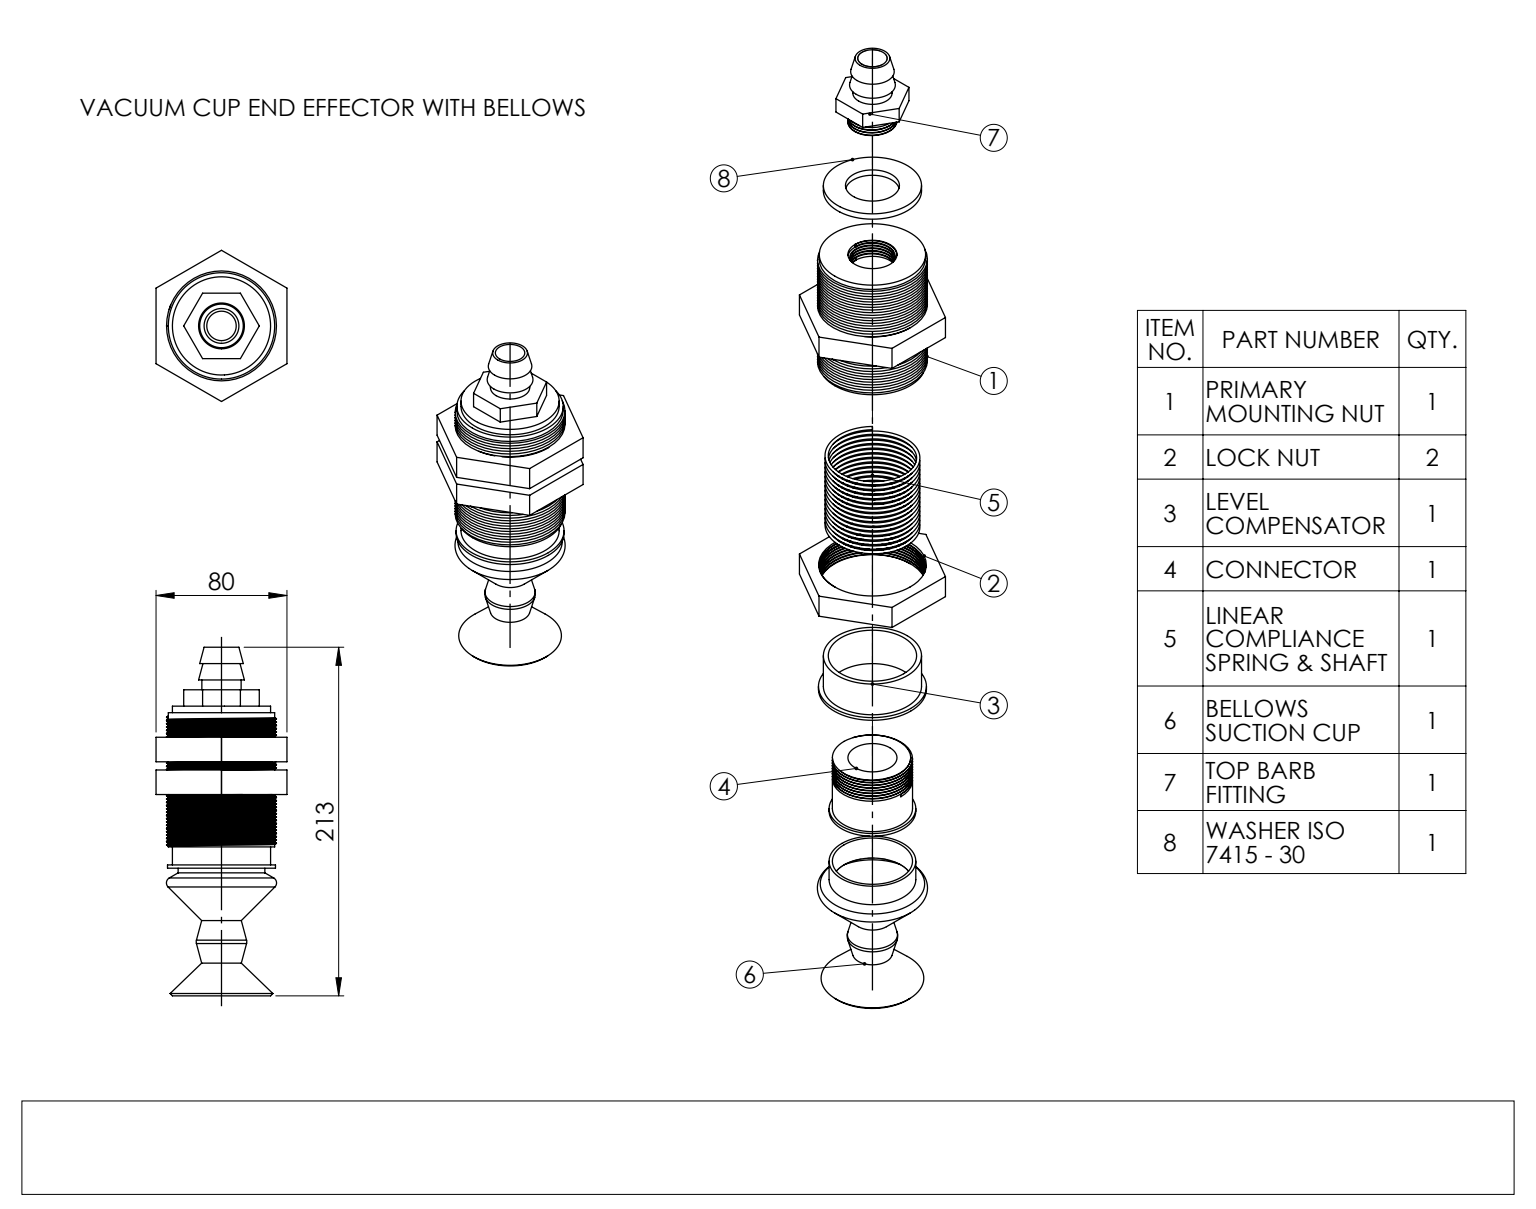
ISO-10303-21;
HEADER;
FILE_DESCRIPTION (('STEP AP214'),
    '1' );
FILE_NAME ('BR-007',
    '2026-10-02T18:08:48',
    ( '' ),
    ( '' ),
    'SwSTEP 2.0',
    'SolidWorks 2026',
    '' );
FILE_SCHEMA (( 'AUTOMOTIVE_DESIGN' ));
ENDSEC;

DATA;
#1 = CARTESIAN_POINT ( 'NONE',  ( -2.584737979205441561E-13, 22.74218749999999645, -30.02300923189239512 ) ) ;
#2 = CARTESIAN_POINT ( 'NONE',  ( 20.75514604977249178, 32.07500000273117990, 28.56700777964553950 ) ) ;
#3 = CARTESIAN_POINT ( 'NONE',  ( 7.236395654485760609, 11.52499999726880375, -22.27133577429736633 ) ) ;
#4 = ORIENTED_EDGE ( 'NONE', *, *, #32426, .T. ) ;
#5 = CARTESIAN_POINT ( 'NONE',  ( 0.04044903254992426173, 37.93006916759064495, -30.02300923189239867 ) ) ;
#6 = B_SPLINE_CURVE_WITH_KNOTS ( 'NONE', 3,
 ( #2746, #31563, #23520, #5150, #31895, #33979, #26595, #13563, #7891, #10812, #8061, #21292, #8391, #3092, #18876, #13210, #18378, #13388, #5322, #18546, #24026, #325, #29325, #15802, #5827, #26258, #31732, #495, #23687, #16306, #152, #15636, #2584, #10642 ),
 .UNSPECIFIED., .F., .F.,
 ( 4, 2, 2, 2, 2, 2, 2, 2, 2, 2, 2, 2, 2, 2, 2, 2, 4 ),
 ( 6.762863467562367515E-16, 0.001783076374787156146, 0.003566152749573635750, 0.007132305499146594091, 0.008023843686539834652, 0.008915381873933073478, 0.01069845824871955460, 0.01248153462350603572, 0.01426461099829251858, 0.01604768737307899970, 0.01783076374786548429, 0.02139691649743844307, 0.02228845468483168710, 0.02317999287222492766, 0.02496306924701141225, 0.02674614562179789337, 0.02852922199658437796 ),
 .UNSPECIFIED. ) ;
#7 = CARTESIAN_POINT ( 'NONE',  ( -32.50000000000000000, 22.50000000546238610, 0.000000000000000000 ) ) ;
#8 = CARTESIAN_POINT ( 'NONE',  ( -2.584737979205441561E-13, 43.36718749999999289, -30.02300923189239512 ) ) ;
#9 = CARTESIAN_POINT ( 'NONE',  ( -23.09401076758502924, 96.00000000000002842, 5.354274672883389237E-15 ) ) ;
#10 = CARTESIAN_POINT ( 'NONE',  ( -2.162160676586881955E-15, 52.87500000273119838, -35.31076352940723240 ) ) ;
#11 = CARTESIAN_POINT ( 'NONE',  ( -2.092463501923844636E-15, 58.00000000546235412, -34.17252228774368916 ) ) ;
#12 = PRODUCT ( 'top barb fitting', 'top barb fitting', '', ( #25356 ) ) ;
#13 = CARTESIAN_POINT ( 'NONE',  ( 15.14183272437242067, 5.449999994537614967, 20.84094480462498211 ) ) ;
#14 = CARTESIAN_POINT ( 'NONE',  ( -2.162160676586881955E-15, 42.62500000273119838, -35.31076352940723240 ) ) ;
#15 = CARTESIAN_POINT ( 'NONE',  ( -4.635254915624208216, 72.40000000000001990, 14.26584774442730463 ) ) ;
#16 = CARTESIAN_POINT ( 'NONE',  ( 33.58253175000000113, 68.47500000273119269, -10.91162601494193751 ) ) ;
#17 =( REPRESENTATION_RELATIONSHIP ('NONE','NONE', #5873, #19696 ) REPRESENTATION_RELATIONSHIP_WITH_TRANSFORMATION ( #15926 )SHAPE_REPRESENTATION_RELATIONSHIP( ) );
#18 = CARTESIAN_POINT ( 'NONE',  ( 13.91687918246660871, 74.00000000000008527, 0.9182373085827880699 ) ) ;
#19 = CARTESIAN_POINT ( 'NONE',  ( 10.37757302488624767, 61.72500000273119269, 31.93888565452638417 ) ) ;
#20 = CARTESIAN_POINT ( 'NONE',  ( 28.01184896238290278, 23.45833333333333215, -7.505752307973347470 ) ) ;
#21 = CARTESIAN_POINT ( 'NONE',  ( 6.277390505771533514E-15, 44.49999999999999289, 34.17252228774368916 ) ) ;
#22 = CARTESIAN_POINT ( 'NONE',  ( 14.47279130897151589, 4.324999997268801799, 19.92008829642072953 ) ) ;
#23 = CARTESIAN_POINT ( 'NONE',  ( -10.37757302488624411, 12.97500000273119092, -31.93888565452638417 ) ) ;
#24 = CARTESIAN_POINT ( 'NONE',  ( -10.04305231718579172, 66.10000000546239107, -30.90933677959248982 ) ) ;
#25 = CARTESIAN_POINT ( 'NONE',  ( -13.94119854578892514, 33.62201416574269075, 24.22776226481266448 ) ) ;
#26 = LINE ( 'NONE', #5703, #33612 ) ;
#27 = CARTESIAN_POINT ( 'NONE',  ( 15.00000000000000355, 75.15000000546237402, 4.873795443493592394 ) ) ;
#28 = CARTESIAN_POINT ( 'NONE',  ( 0.000000000000000000, 82.00000000000001421, 0.000000000000000000 ) ) ;
#29 = CARTESIAN_POINT ( 'NONE',  ( 20.75514604977249178, 76.07500000273118701, 28.56700777964553950 ) ) ;
#30 = EDGE_LOOP ( 'NONE', ( #10708, #16576, #32789, #18480 ) ) ;
#31 = DIRECTION ( 'NONE',  ( 0.000000000000000000, -1.000000000000000000, 0.000000000000000000 ) ) ;
#32 = CARTESIAN_POINT ( 'NONE',  ( -26.07999730980477437, 56.11458333333332860, 6.988114217768305103 ) ) ;
#33 = EDGE_CURVE ( 'NONE', #10375, #21334, #32773, .T. ) ;
#34 = CARTESIAN_POINT ( 'NONE',  ( 20.75514604977248467, 54.42500000273117422, -28.56700777964554305 ) ) ;
#35 = CARTESIAN_POINT ( 'NONE',  ( 33.58253175000000113, 14.37500000273118950, -4.112674001490185761E-15 ) ) ;
#36 = CARTESIAN_POINT ( 'NONE',  ( 10.37757302488624056, 4.775000002731191628, -31.93888565452638417 ) ) ;
#37 = CARTESIAN_POINT ( 'NONE',  ( -6.988114217767819270, 38.35416666666666430, 26.07999730980490583 ) ) ;
#38 = CARTESIAN_POINT ( 'NONE',  ( 30.02300923189239867, 28.47694416759064495, 0.04044903254992252006 ) ) ;
#39 = CARTESIAN_POINT ( 'NONE',  ( 7.543491769121922985, 16.00482666574268720, 28.00173670424535644 ) ) ;
#40 = CARTESIAN_POINT ( 'NONE',  ( -26.29305231718578995, 76.70000000546238539, 19.10302069950538595 ) ) ;
#41 =( BOUNDED_CURVE ( )  B_SPLINE_CURVE ( 2, ( #27655, #11863, #29882, #19433, #17198, #32453, #30382, #1391, #9453, #17026, #24905, #17535, #22341 ),
 .UNSPECIFIED., .F., .T. ) 
 B_SPLINE_CURVE_WITH_KNOTS ( ( 3, 2, 2, 2, 2, 2, 3 ),
 ( 0.2756410256410256610, 0.2769230769230769384, 0.2794871794871794934, 0.2820512820512820484, 0.2846153846153846034, 0.2871794871794871584, 0.2884615384615384914 ),
 .UNSPECIFIED. ) 
 CURVE ( )  GEOMETRIC_REPRESENTATION_ITEM ( )  RATIONAL_B_SPLINE_CURVE ( ( 0.9755282581475768211, 0.9755282581475768211, 1.000000000000000000, 0.9510565162951535312, 1.000000000000000000, 0.9510565162951535312, 1.000000000000000000, 0.9510565162951535312, 1.000000000000000000, 0.9510565162951535312, 1.000000000000000000, 0.9755282581475762660, 0.9755282581475768211 ) ) 
 REPRESENTATION_ITEM ( '' )  );
#42 = CARTESIAN_POINT ( 'NONE',  ( 1.353501352685244852, 52.00000000000004263, -32.52334280248234677 ) ) ;
#43 = CARTESIAN_POINT ( 'NONE',  ( 27.16883889988623935, 38.32500000273120122, -19.73931689729374384 ) ) ;
#44 = CARTESIAN_POINT ( 'NONE',  ( -14.01125832528328985, 48.51784749907601935, -24.18731323226223040 ) ) ;
#45 = CARTESIAN_POINT ( 'NONE',  ( -14.47279130897151589, 9.324999997268816898, -19.92008829642072598 ) ) ;
#46 = CARTESIAN_POINT ( 'NONE',  ( -5.147494310547430452, 2.051254287009222299, -32.49999999999999289 ) ) ;
#47 = ORIENTED_EDGE ( 'NONE', *, *, #4310, .T. ) ;
#48 = CARTESIAN_POINT ( 'NONE',  ( -33.58253175000000113, 53.27500000273117564, -10.91162601494193218 ) ) ;
#49 = CARTESIAN_POINT ( 'NONE',  ( -12.13525491562420910, 70.45000000546237118, 8.816778784387098611 ) ) ;
#50 = CARTESIAN_POINT ( 'NONE',  ( -24.22776226481240514, 43.65923583425730925, 13.94119854578937812 ) ) ;
#51 = CARTESIAN_POINT ( 'NONE',  ( 10.37757302488624056, 76.77500000273118985, -31.93888565452638417 ) ) ;
#52 = VERTEX_POINT ( 'NONE', #19751 ) ;
#53 = CARTESIAN_POINT ( 'NONE',  ( -10.37757302488624411, 22.72500000273118559, -31.93888565452638417 ) ) ;
#54 = CARTESIAN_POINT ( 'NONE',  ( 15.01150461594596308, 19.59114583333332149, -26.00068869287367335 ) ) ;
#55 = EDGE_LOOP ( 'NONE', ( #23841, #28367, #25851, #31674 ) ) ;
#56 = LINE ( 'NONE', #23253, #28638 ) ;
#57 = CARTESIAN_POINT ( 'NONE',  ( -2.162160676586881955E-15, 60.62500000273117706, -35.31076352940723240 ) ) ;
#58 = CARTESIAN_POINT ( 'NONE',  ( -7.505752307973343918, 46.66145833333332860, -28.01184896238290989 ) ) ;
#59 = CARTESIAN_POINT ( 'NONE',  ( -5.147494310547423346, 66.94874572391552192, 32.50000000000000000 ) ) ;
#60 = CARTESIAN_POINT ( 'NONE',  ( 14.47279130897151767, 8.824999997268804464, 19.92008829642072953 ) ) ;
#61 = CARTESIAN_POINT ( 'NONE',  ( 27.16883889988624290, 1.925000002731186433, 19.73931689729373673 ) ) ;
#62 = CARTESIAN_POINT ( 'NONE',  ( -1.778240108872766143E-15, 8.000000005462370112, -32.49999999999999289 ) ) ;
#63 = CARTESIAN_POINT ( 'NONE',  ( 7.543491769121922985, 64.12982666574268364, 28.00173670424535644 ) ) ;
#64 = B_SPLINE_CURVE_WITH_KNOTS ( 'NONE', 3,
 ( #12577, #7079, #6739, #22702, #12751, #9302, #25452, #17563, #30235, #33154 ),
 .UNSPECIFIED., .F., .F.,
 ( 4, 2, 2, 2, 4 ),
 ( 0.000000000000000000, 0.006590582801587737370, 0.01318116560317547474, 0.01977174840476321124, 0.02636233120635094948 ),
 .UNSPECIFIED. ) ;
#65 = CARTESIAN_POINT ( 'NONE',  ( -15.00000000000000000, 80.25000000546239676, 0.000000000000000000 ) ) ;
#66 = CARTESIAN_POINT ( 'NONE',  ( 1.093617666956751375E-13, 66.00000000546238255, -32.50000000000000711 ) ) ;
#67 = CARTESIAN_POINT ( 'NONE',  ( -5.147494310547423346, 4.448745718453162468, 32.50000000000000000 ) ) ;
#68 = CARTESIAN_POINT ( 'NONE',  ( -10.04305231718579172, 13.59999999999998721, -30.90933677959248982 ) ) ;
#69 = CARTESIAN_POINT ( 'NONE',  ( 27.95245687107223276, 61.41406250000000711, -2.463307335887066074E-13 ) ) ;
#70 = CARTESIAN_POINT ( 'NONE',  ( -15.14183272437242600, 17.04999999453762527, 20.84094480462497856 ) ) ;
#71 = CARTESIAN_POINT ( 'NONE',  ( 9.270509831248423538, 73.55000000546237970, -12.75976212528059861 ) ) ;
#72 = CARTESIAN_POINT ( 'NONE',  ( 24.20753774853731244, 30.19010416666665719, -13.97622843553632599 ) ) ;
#73 = CARTESIAN_POINT ( 'NONE',  ( 6.486482029760649416E-15, 29.62500000273120193, 35.31076352940723240 ) ) ;
#74 = CARTESIAN_POINT ( 'NONE',  ( -27.16883889988624290, 70.92500000273120975, -19.73931689729374028 ) ) ;
#75 = AXIS2_PLACEMENT_3D ( 'NONE', #28014, #5016, #30577 ) ;
#76 = CARTESIAN_POINT ( 'NONE',  ( -33.58253175000000113, 33.37500000273117706, 0.000000000000000000 ) ) ;
#77 = CARTESIAN_POINT ( 'NONE',  ( -2.162160676586882350E-15, 12.87500000273117884, -35.31076352940722529 ) ) ;
#78 = PRODUCT_DEFINITION ( 'UNKNOWN', '', #3307, #996 ) ;
#79 = CARTESIAN_POINT ( 'NONE',  ( -10.04305231718579172, 63.59999999999998721, -30.90933677959248982 ) ) ;
#80 = CARTESIAN_POINT ( 'NONE',  ( 13.94119854578937812, 56.54986083425731636, 24.22776226481240514 ) ) ;
#81 = CARTESIAN_POINT ( 'NONE',  ( -27.16883889988623935, 75.32500000273117280, 19.73931689729374739 ) ) ;
#82 = CARTESIAN_POINT ( 'NONE',  ( 3.880418787951153803, 7.551254281546842861, 24.49999999999999645 ) ) ;
#83 = CARTESIAN_POINT ( 'NONE',  ( -20.08610463437157989, 55.69999999999998863, -27.64615127144129758 ) ) ;
#84 = CARTESIAN_POINT ( 'NONE',  ( 1.507698388325705758E-15, 17.12499999726880517, -24.62258325217400312 ) ) ;
#85 = CARTESIAN_POINT ( 'NONE',  ( 33.58253175000000113, 58.12500000273118417, -4.112674001490185761E-15 ) ) ;
#86 = CARTESIAN_POINT ( 'NONE',  ( -7.236395654485757944, 9.724999997268806595, -22.27133577429736988 ) ) ;
#87 = ORIENTED_EDGE ( 'NONE', *, *, #10321, .T. ) ;
#88 = CARTESIAN_POINT ( 'NONE',  ( 10.37757302488624767, 71.97500000273120691, 31.93888565452638417 ) ) ;
#89 = CARTESIAN_POINT ( 'NONE',  ( 33.58253175000000113, 6.225000002731185589, -10.91162601494193574 ) ) ;
#90 = CARTESIAN_POINT ( 'NONE',  ( -7.236395654485763274, 16.52499999726880731, 22.27133577429736633 ) ) ;
#91 = CARTESIAN_POINT ( 'NONE',  ( -0.04044903254992426173, 15.58631916759064495, 27.95245687107223276 ) ) ;
#92 = EDGE_LOOP ( 'NONE', ( #2130, #17184, #1564 ) ) ;
#93 = CARTESIAN_POINT ( 'NONE',  ( 6.486482029760649416E-15, 43.62500000273116285, 35.31076352940723240 ) ) ;
#94 = ORIENTED_EDGE ( 'NONE', *, *, #21026, .F. ) ;
#95 = CARTESIAN_POINT ( 'NONE',  ( 7.505752307972854531, 43.51041666666666430, -28.01184896238303423 ) ) ;
#96 = DIRECTION ( 'NONE',  ( 0.000000000000000000, -1.000000000000000000, 0.000000000000000000 ) ) ;
#97 = CARTESIAN_POINT ( 'NONE',  ( -20.08610463437157989, 4.200000005462371178, -27.64615127144129758 ) ) ;
#98 = CARTESIAN_POINT ( 'NONE',  ( -20.75514604977248112, 77.42500000273119554, 28.56700777964554661 ) ) ;
#99 = CARTESIAN_POINT ( 'NONE',  ( 28.01184896238304134, 16.86979166666666075, 7.505752307972846538 ) ) ;
#100 = CARTESIAN_POINT ( 'NONE',  ( 1.577395562988744260E-15, 2.500000000000008882, -25.76082449383753925 ) ) ;
#101 = CARTESIAN_POINT ( 'NONE',  ( 27.16883889988623935, 12.57500000273120655, -19.73931689729374384 ) ) ;
#102 = CARTESIAN_POINT ( 'NONE',  ( 26.29305231718578995, 59.20000000000000284, -19.10302069950538240 ) ) ;
#103 = CARTESIAN_POINT ( 'NONE',  ( 10.04305231718578817, 73.90000000546237402, -30.90933677959249337 ) ) ;
#104 = CARTESIAN_POINT ( 'NONE',  ( -7.543491769121917656, 31.47357666574268364, -28.00173670424536354 ) ) ;
#105 = CARTESIAN_POINT ( 'NONE',  ( -11.25946833292375793, 75.57500000273120122, 8.180482586598737171 ) ) ;
#106 = CARTESIAN_POINT ( 'NONE',  ( 28.01184896238304134, 37.49479166666666430, 7.505752307972846538 ) ) ;
#107 = CARTESIAN_POINT ( 'NONE',  ( 0.000000000000000000, 82.00000000000001421, 0.000000000000000000 ) ) ;
#108 = CARTESIAN_POINT ( 'NONE',  ( -24.50000000000000000, 12.90000000000000036, -7.960532557706207157 ) ) ;
#109 = CARTESIAN_POINT ( 'NONE',  ( 32.50000000000000711, 4.899999999999989697, 10.55989012756945122 ) ) ;
#110 = CARTESIAN_POINT ( 'NONE',  ( 2.757615341152813402E-15, -45.51763809020504681, 0.000000000000000000 ) ) ;
#111 = CARTESIAN_POINT ( 'NONE',  ( -24.18731323226221974, 61.40847249907603356, 14.01125832528330406 ) ) ;
#112 = CARTESIAN_POINT ( 'NONE',  ( 27.16883889988624290, 47.92500000273120264, 19.73931689729373673 ) ) ;
#113 = CARTESIAN_POINT ( 'NONE',  ( 27.16883889988623935, 52.57500000273117280, -19.73931689729374384 ) ) ;
#114 = CARTESIAN_POINT ( 'NONE',  ( -27.16883889988623935, 33.57500000273120122, 19.73931689729374739 ) ) ;
#115 = CARTESIAN_POINT ( 'NONE',  ( 0.000000000000000000, 16.99999999999998579, -15.00000000000000000 ) ) ;
#116 = CARTESIAN_POINT ( 'NONE',  ( 26.07999730980477437, 16.58333333333333215, -6.988114217768290004 ) ) ;
#117 = CARTESIAN_POINT ( 'NONE',  ( 5.147494310547434893, 15.05125428700922541, 32.49999999999999289 ) ) ;
#118 = CARTESIAN_POINT ( 'NONE',  ( -1.778240108872766143E-15, 22.00000000546237899, -32.49999999999999289 ) ) ;
#119 = DIRECTION ( 'NONE',  ( -0.000000000000000000, 1.000000000000000000, -0.000000000000000000 ) ) ;
#120 = CARTESIAN_POINT ( 'NONE',  ( 6.486482029760649416E-15, 15.62500000273117884, 35.31076352940723240 ) ) ;
#121 = DIRECTION ( 'NONE',  ( -0.000000000000000000, 1.000000000000000000, -0.000000000000000000 ) ) ;
#122 = CARTESIAN_POINT ( 'NONE',  ( 0.000000000000000000, -21.99999999999999645, 0.000000000000000000 ) ) ;
#123 = ADVANCED_FACE ( 'NONE', ( #17350, #12018 ), #22832, .T. ) ;
#124 = CARTESIAN_POINT ( 'NONE',  ( -10.04305231718578462, 40.39999999999999147, 30.90933677959249337 ) ) ;
#125 = CARTESIAN_POINT ( 'NONE',  ( 24.22776226481265383, 22.45013916574269075, 13.94119854578893580 ) ) ;
#126 = CARTESIAN_POINT ( 'NONE',  ( 20.08610463437157279, 33.80000000546235839, -27.64615127144129758 ) ) ;
#127 = CARTESIAN_POINT ( 'NONE',  ( 5.779280353836490358E-15, 12.49999999999999112, 32.49999999999999289 ) ) ;
#128 = CARTESIAN_POINT ( 'NONE',  ( 10.37757302488624056, 26.52500000273119696, -31.93888565452638417 ) ) ;
#129 = CARTESIAN_POINT ( 'NONE',  ( -19.09188309203694445, 42.93750000000000000, -19.09188309203661049 ) ) ;
#130 = EDGE_LOOP ( 'NONE', ( #13807, #32440, #5639, #27881 ) ) ;
#131 = CARTESIAN_POINT ( 'NONE',  ( -33.58253175000000113, 63.02500000273118985, -10.91162601494193218 ) ) ;
#132 = EDGE_CURVE ( 'NONE', #774, #12058, #32938, .T. ) ;
#133 = ORIENTED_EDGE ( 'NONE', *, *, #14029, .F. ) ;
#134 = CARTESIAN_POINT ( 'NONE',  ( -15.04653450569291984, 63.99777750092396644, 25.98046417659859486 ) ) ;
#135 = CARTESIAN_POINT ( 'NONE',  ( -30.02300923189239867, 16.44569416759064140, -0.04044903254991731589 ) ) ;
#136 = CIRCLE ( 'NONE', #19335, 15.31593959127081384 ) ;
#137 = CARTESIAN_POINT ( 'NONE',  ( -20.75514604977248112, 3.425000002731186655, 28.56700777964554661 ) ) ;
#138 = CARTESIAN_POINT ( 'NONE',  ( -23.41746825000000243, 1.524999997268801755, -7.608796670333730638 ) ) ;
#139 = CARTESIAN_POINT ( 'NONE',  ( 33.58253175000000113, 32.37500000273119127, -4.112674001490185761E-15 ) ) ;
#140 = CARTESIAN_POINT ( 'NONE',  ( -32.50000000000000000, 36.40000000546236691, -10.55989012756945478 ) ) ;
#141 =( BOUNDED_CURVE ( )  B_SPLINE_CURVE ( 2, ( #20409, #30859, #4610, #33262, #20067, #17493, #25204, #17837, #11988, #19888, #1681, #4780, #33084 ),
 .UNSPECIFIED., .F., .T. ) 
 B_SPLINE_CURVE_WITH_KNOTS ( ( 3, 2, 2, 2, 2, 2, 3 ),
 ( 0.2243589743589743668, 0.2256410256410256443, 0.2282051282051281993, 0.2307692307692307820, 0.2333333333333333370, 0.2358974358974358920, 0.2371794871794871973 ),
 .UNSPECIFIED. ) 
 CURVE ( )  GEOMETRIC_REPRESENTATION_ITEM ( )  RATIONAL_B_SPLINE_CURVE ( ( 0.9755282581475768211, 0.9755282581475768211, 1.000000000000000000, 0.9510565162951535312, 1.000000000000000000, 0.9510565162951535312, 1.000000000000000000, 0.9510565162951535312, 1.000000000000000000, 0.9510565162951535312, 1.000000000000000000, 0.9755282581475764880, 0.9755282581475768211 ) ) 
 REPRESENTATION_ITEM ( '' )  );
#142 = CARTESIAN_POINT ( 'NONE',  ( -15.00000000000000000, 72.09999999999999432, 4.873795443493597723 ) ) ;
#143 = DIRECTION ( 'NONE',  ( -1.224646799147353454E-16, 1.000000000000000000, -0.000000000000000000 ) ) ;
#144 = CARTESIAN_POINT ( 'NONE',  ( 20.08610463437158344, 76.69999999999998863, 27.64615127144129403 ) ) ;
#145 = CARTESIAN_POINT ( 'NONE',  ( 27.16883889988623935, 50.57500000273118701, -19.73931689729374384 ) ) ;
#146 =( LENGTH_UNIT ( ) NAMED_UNIT ( * ) SI_UNIT ( .MILLI., .METRE. ) );
#147 = CARTESIAN_POINT ( 'NONE',  ( 6.277390505771533514E-15, 20.49999999999999289, 34.17252228774368916 ) ) ;
#148 = CARTESIAN_POINT ( 'NONE',  ( -32.50000000000000000, 18.09999999999998010, 10.55989012756946366 ) ) ;
#149 = CARTESIAN_POINT ( 'NONE',  ( 7.570916362186213000, 8.399999999999991473, -23.30088464923126423 ) ) ;
#150 = CARTESIAN_POINT ( 'NONE',  ( 20.75514604977248467, 68.42500000273120975, -28.56700777964554305 ) ) ;
#151 = CARTESIAN_POINT ( 'NONE',  ( -32.50000000000000000, 78.10000000000002274, 10.55989012756946366 ) ) ;
#152 = CARTESIAN_POINT ( 'NONE',  ( 11.86847005202517380, 74.00000000000004263, -7.471229617278120294 ) ) ;
#153 = CARTESIAN_POINT ( 'NONE',  ( 27.16883889988623935, 56.57500000273118701, -19.73931689729374384 ) ) ;
#154 = CARTESIAN_POINT ( 'NONE',  ( 20.08610463437158344, 72.70000000000000284, 27.64615127144129403 ) ) ;
#155 = CARTESIAN_POINT ( 'NONE',  ( -10.37757302488623701, 13.52500000273118630, 31.93888565452638417 ) ) ;
#156 = CARTESIAN_POINT ( 'NONE',  ( 0.04044903254993986036, 31.05506916759064495, -27.95245687107223986 ) ) ;
#157 = CARTESIAN_POINT ( 'NONE',  ( -6.410174973103736740, 66.99999999999995737, -32.88179426022560392 ) ) ;
#158 = AXIS2_PLACEMENT_3D ( 'NONE', #33870, #18769, #28713 ) ;
#159 = CARTESIAN_POINT ( 'NONE',  ( 33.58253175000000113, 2.475000002731187809, -10.91162601494193574 ) ) ;
#160 = CARTESIAN_POINT ( 'NONE',  ( -33.58253175000000113, 33.02500000273118275, -10.91162601494193218 ) ) ;
#161 = FACE_OUTER_BOUND ( 'NONE', #7601, .T. ) ;
#162 = CARTESIAN_POINT ( 'NONE',  ( 12.90513655866702081, 52.00000000000000711, 31.00393344628893288 ) ) ;
#163 = CARTESIAN_POINT ( 'NONE',  ( 8.601468415847520532, 79.57500000273117280, 11.83890561707634603 ) ) ;
#164 = CARTESIAN_POINT ( 'NONE',  ( -7.543491769121917656, 48.66107666574268364, -28.00173670424536354 ) ) ;
#165 = CARTESIAN_POINT ( 'NONE',  ( 20.08610463437158344, 53.20000000546237118, 27.64615127144129403 ) ) ;
#166 = CARTESIAN_POINT ( 'NONE',  ( 8.601468415847516980, 76.67500000273118133, -11.83890561707634781 ) ) ;
#167 = LINE ( 'NONE', #25929, #20571 ) ;
#168 = CARTESIAN_POINT ( 'NONE',  ( 27.95245687107222921, 20.16406249999999645, -2.463307335887066074E-13 ) ) ;
#169 = CARTESIAN_POINT ( 'NONE',  ( -23.41746825000000243, 8.024999997268801977, -7.608796670333730638 ) ) ;
#170 = CARTESIAN_POINT ( 'NONE',  ( 10.04305231718578817, 69.90000000546237402, -30.90933677959249337 ) ) ;
#171 = CARTESIAN_POINT ( 'NONE',  ( 15.01150461594596308, 19.59114583333332149, -26.00068869287367335 ) ) ;
#172 = CARTESIAN_POINT ( 'NONE',  ( 10.37757302488624767, 25.97500000273118914, 31.93888565452638417 ) ) ;
#173 = CARTESIAN_POINT ( 'NONE',  ( -4.523095164977117273E-15, 14.62499999726882649, 24.62258325217400312 ) ) ;
#174 = EDGE_LOOP ( 'NONE', ( #26748, #4103, #22808, #13833 ) ) ;
#175 = CARTESIAN_POINT ( 'NONE',  ( -0.04044903254990864921, 43.08631916759065916, 30.02300923189239867 ) ) ;
#176 = CARTESIAN_POINT ( 'NONE',  ( -20.08610463437156923, 14.80000000546238503, 27.64615127144130113 ) ) ;
#177 = CARTESIAN_POINT ( 'NONE',  ( -26.00068869287368756, 53.10677083333331439, -15.01150461594595775 ) ) ;
#178 = CARTESIAN_POINT ( 'NONE',  ( 31.22091420962414787, -23.06066017177981209, 3.823459265327032686E-15 ) ) ;
#179 = CARTESIAN_POINT ( 'NONE',  ( -33.58253175000000113, 53.37500000273118417, 0.000000000000000000 ) ) ;
#180 = CARTESIAN_POINT ( 'NONE',  ( -20.08610463437156923, 54.80000000546237260, 27.64615127144130113 ) ) ;
#181 = EDGE_CURVE ( 'NONE', #2430, #476, #12819, .T. ) ;
#182 = DIRECTION ( 'NONE',  ( -0.000000000000000000, -1.000000000000000000, -0.000000000000000000 ) ) ;
#183 = CARTESIAN_POINT ( 'NONE',  ( 6.486482029760649416E-15, 41.62500000273116996, 35.31076352940723240 ) ) ;
#184 = CARTESIAN_POINT ( 'NONE',  ( 12.13525491562420910, 73.45000000546237118, -8.816778784387098611 ) ) ;
#185 = CARTESIAN_POINT ( 'NONE',  ( 10.37757302488624056, 68.77500000273117564, -31.93888565452638417 ) ) ;
#186 = CARTESIAN_POINT ( 'NONE',  ( -32.50000000000000000, 0.6000000054623972900, 10.55989012756946366 ) ) ;
#187 = AXIS2_PLACEMENT_3D ( 'NONE', #2552, #20584, #13357 ) ;
#188 = CARTESIAN_POINT ( 'NONE',  ( 10.37757302488624056, 60.52500000273118275, -31.93888565452638417 ) ) ;
#189 = CARTESIAN_POINT ( 'NONE',  ( -7.505752307973343918, 26.03645833333333215, -28.01184896238290989 ) ) ;
#190 = CARTESIAN_POINT ( 'NONE',  ( 32.50000000000000000, 44.99999999999998579, -3.980102097228898626E-15 ) ) ;
#191 = CARTESIAN_POINT ( 'NONE',  ( -7.236395654485763274, 6.024999997268825958, 22.27133577429736633 ) ) ;
#192 = CARTESIAN_POINT ( 'NONE',  ( 20.75514604977249178, 14.07500000273119944, 28.56700777964553950 ) ) ;
#193 = CYLINDRICAL_SURFACE ( 'NONE', #6349, 32.50000000000000000 ) ;
#194 = CARTESIAN_POINT ( 'NONE',  ( 7.025853678916867295, 36.62982666574267654, 26.06988505166722803 ) ) ;
#195 = CARTESIAN_POINT ( 'NONE',  ( -4.300734207923759378, 74.97500000273119269, -13.23629886949340495 ) ) ;
#196 = CARTESIAN_POINT ( 'NONE',  ( -1.714505518806294835E-15, 102.0000000000000284, -14.00000000000000178 ) ) ;
#197 = CARTESIAN_POINT ( 'NONE',  ( -1.778240108872766143E-15, 21.50000000000000000, -32.49999999999999289 ) ) ;
#198 = CARTESIAN_POINT ( 'NONE',  ( -33.58253175000000113, 73.27500000273118985, -10.91162601494193218 ) ) ;
#199 = ORIENTED_EDGE ( 'NONE', *, *, #10938, .T. ) ;
#200 = FACE_OUTER_BOUND ( 'NONE', #19419, .T. ) ;
#201 = CARTESIAN_POINT ( 'NONE',  ( 19.09188309203694800, 58.40625000000000711, 19.09188309203660694 ) ) ;
#202 = CARTESIAN_POINT ( 'NONE',  ( 27.16883889988623935, 52.32500000273120122, -19.73931689729374384 ) ) ;
#203 = CARTESIAN_POINT ( 'NONE',  ( 33.58253175000000113, 16.37500000273119127, -4.112674001490185761E-15 ) ) ;
#204 = CARTESIAN_POINT ( 'NONE',  ( 33.58253175000000113, 6.475000002731178483, -10.91162601494193751 ) ) ;
#205 = CARTESIAN_POINT ( 'NONE',  ( -19.09188309203694445, 42.93750000000000000, -19.09188309203661049 ) ) ;
#206 = CARTESIAN_POINT ( 'NONE',  ( -20.47846945139902175, 34.06288166759063785, -20.53372385742072481 ) ) ;
#207 = CARTESIAN_POINT ( 'NONE',  ( -25.98046417659831420, 16.72097249907602290, 15.04653450569339945 ) ) ;
#208 = CARTESIAN_POINT ( 'NONE',  ( -26.29305231718579350, 76.30000000546237970, -19.10302069950537884 ) ) ;
#209 = CARTESIAN_POINT ( 'NONE',  ( 33.29860495311163504, 51.99999999999997868, -1.751800823569056309 ) ) ;
#210 = CLOSED_SHELL ( 'NONE', ( #8729, #14117, #31790, #11042, #12512, #8597, #17021, #15792, #28040, #1353, #2874, #26985, #12292, #25228, #17408, #25082, #11130, #24622, #12986, #14394, #9494, #16184, #21021, #7313, #8316, #7903, #7462, #29778, #24071, #10707, #8891, #2660, #1384, #1595, #31267, #2291, #15122, #887, #228, #13989, #650, #29273, #23959 ) ) ;
#211 = CARTESIAN_POINT ( 'NONE',  ( 33.58253175000000113, 40.12500000273119838, -4.112674001490185761E-15 ) ) ;
#212 = CARTESIAN_POINT ( 'NONE',  ( 19.11951029504797006, 43.21836833240935505, 19.06425588902558133 ) ) ;
#213 = CIRCLE ( 'NONE', #1854, 31.22091420962414787 ) ;
#214 = CARTESIAN_POINT ( 'NONE',  ( -4.523095164977116484E-15, 12.12499999726881406, 24.62258325217400312 ) ) ;
#215 = DIRECTION ( 'NONE',  ( 1.224646799147353454E-16, -1.000000000000000000, 0.000000000000000000 ) ) ;
#216 = ORIENTED_EDGE ( 'NONE', *, *, #8928, .T. ) ;
#217 = CARTESIAN_POINT ( 'NONE',  ( 27.16883889988623935, 46.57500000273119412, -19.73931689729374384 ) ) ;
#218 = CARTESIAN_POINT ( 'NONE',  ( -24.18731323226248264, 44.23215250092398065, -14.01125832528284931 ) ) ;
#219 = CARTESIAN_POINT ( 'NONE',  ( 33.58253175000000823, 72.27500000273118985, 10.91162601494192863 ) ) ;
#220 = VERTEX_POINT ( 'NONE', #33464 ) ;
#221 = CARTESIAN_POINT ( 'NONE',  ( -33.58253175000000113, 25.22500000273119625, 10.91162601494193929 ) ) ;
#222 = CARTESIAN_POINT ( 'NONE',  ( 15.01150461594643204, 27.61197916666666430, 26.00068869287340334 ) ) ;
#223 = EDGE_CURVE ( 'NONE', #23252, #23800, #3174, .T. ) ;
#224 = EDGE_LOOP ( 'NONE', ( #22388, #1047, #13319, #25437 ) ) ;
#225 = FACE_OUTER_BOUND ( 'NONE', #13152, .T. ) ;
#226 = CARTESIAN_POINT ( 'NONE',  ( 27.16883889988624290, 61.92500000273118133, 19.73931689729373673 ) ) ;
#227 = CARTESIAN_POINT ( 'NONE',  ( -7.505752307972844761, 48.66666666666666430, 28.01184896238304134 ) ) ;
#228 = ADVANCED_FACE ( 'NONE', ( #2232 ), #22152, .F. ) ;
#229 = DIRECTION ( 'NONE',  ( 0.7202789989107551971, -0.6936844842780615084, 0.000000000000000000 ) ) ;
#230 = CARTESIAN_POINT ( 'NONE',  ( 23.41746824999999887, 7.224999997268826135, -7.608796670333727974 ) ) ;
#231 =( GEOMETRIC_REPRESENTATION_CONTEXT ( 3 ) GLOBAL_UNCERTAINTY_ASSIGNED_CONTEXT ( ( #25969 ) ) GLOBAL_UNIT_ASSIGNED_CONTEXT ( ( #31394, #13204, #25908 ) ) REPRESENTATION_CONTEXT ( 'NONE', 'WORKASPACE' ) );
#232 = CARTESIAN_POINT ( 'NONE',  ( 33.58253175000000823, 4.025000002731196957, 10.91162601494192863 ) ) ;
#233 = CARTESIAN_POINT ( 'NONE',  ( -27.16883889988624290, 31.17500000273118488, -19.73931689729374028 ) ) ;
#234 = CARTESIAN_POINT ( 'NONE',  ( 32.50000000000000000, 5.600000005462384856, -10.55989012756945833 ) ) ;
#235 = CARTESIAN_POINT ( 'NONE',  ( -30.02300923189239867, 61.69493083240936926, 0.04044903255044988294 ) ) ;
#236 = CARTESIAN_POINT ( 'NONE',  ( -33.58253175000000113, 79.37500000273118417, 0.000000000000000000 ) ) ;
#237 = AXIS2_PLACEMENT_3D ( 'NONE', #10911, #18810, #13315 ) ;
#238 = CARTESIAN_POINT ( 'NONE',  ( -26.29305231718579350, 31.79999999999999361, -19.10302069950537884 ) ) ;
#239 = CARTESIAN_POINT ( 'NONE',  ( -1.778240108872766143E-15, 69.49999999999998579, -32.49999999999999289 ) ) ;
#240 = CARTESIAN_POINT ( 'NONE',  ( 32.50000000000000000, 19.00000000000000355, -3.980102097228898626E-15 ) ) ;
#241 = CARTESIAN_POINT ( 'NONE',  ( 13.97622843553589966, 57.40364583333332860, -24.20753774853756113 ) ) ;
#242 = CARTESIAN_POINT ( 'NONE',  ( 7.236395654485755280, 2.724999997268801266, 22.27133577429736988 ) ) ;
#243 = CARTESIAN_POINT ( 'NONE',  ( -4.300734207923755825, 79.27500000273118985, 13.23629886949340673 ) ) ;
#244 = CARTESIAN_POINT ( 'NONE',  ( -27.95245687107222921, 32.19531250000000000, 2.498001805406602216E-13 ) ) ;
#245 =( BOUNDED_CURVE ( )  B_SPLINE_CURVE ( 2, ( #20282, #2248, #31077, #20802, #5337, #28338, #4995 ),
 .UNSPECIFIED., .F., .T. ) 
 B_SPLINE_CURVE_WITH_KNOTS ( ( 3, 2, 2, 3 ),
 ( 0.000000000000000000, 0.01111111111111111154, 0.02222222222222222307, 0.02777777777777777971 ),
 .UNSPECIFIED. ) 
 CURVE ( )  GEOMETRIC_REPRESENTATION_ITEM ( )  RATIONAL_B_SPLINE_CURVE ( ( 1.000000000000000000, 0.9510565162951535312, 1.000000000000000000, 0.9510565162951535312, 1.000000000000000000, 0.9755282581475768211, 0.9755282581475768211 ) ) 
 REPRESENTATION_ITEM ( '' )  );
#246 = CARTESIAN_POINT ( 'NONE',  ( 10.37757302488624767, 21.72500000273119980, 31.93888565452638417 ) ) ;
#247 = CARTESIAN_POINT ( 'NONE',  ( 33.58253175000000113, 76.12500000273118417, -4.112674001490185761E-15 ) ) ;
#248 = CARTESIAN_POINT ( 'NONE',  ( 27.16883889988623935, 38.57500000273118701, -19.73931689729374384 ) ) ;
#249 = CARTESIAN_POINT ( 'NONE',  ( -10.37757302488624411, 12.97500000273119092, -31.93888565452638417 ) ) ;
#250 = CARTESIAN_POINT ( 'NONE',  ( -20.08610463437156923, 64.29999999999996874, 27.64615127144130113 ) ) ;
#251 = CARTESIAN_POINT ( 'NONE',  ( -13.94119854578936923, 54.83111083425730214, -24.22776226481241224 ) ) ;
#252 = CARTESIAN_POINT ( 'NONE',  ( 27.16883889988623935, 70.32500000273117280, -19.73931689729374384 ) ) ;
#253 = LINE ( 'NONE', #21716, #27788 ) ;
#254 = CARTESIAN_POINT ( 'NONE',  ( -10.04305231718578462, 56.39999999999999147, 30.90933677959249337 ) ) ;
#255 = CARTESIAN_POINT ( 'NONE',  ( 15.00000000000000355, 79.15000000546238823, 4.873795443493592394 ) ) ;
#256 = CARTESIAN_POINT ( 'NONE',  ( 20.75514604977249178, 55.82500000273118701, 28.56700777964553950 ) ) ;
#257 = CARTESIAN_POINT ( 'NONE',  ( -14.47279130897151589, 7.824999997268807128, -19.92008829642072598 ) ) ;
#258 = ORIENTED_EDGE ( 'NONE', *, *, #24258, .F. ) ;
#259 = CARTESIAN_POINT ( 'NONE',  ( 10.37757302488624056, 70.77500000273118985, -31.93888565452638417 ) ) ;
#260 = CARTESIAN_POINT ( 'NONE',  ( 20.75514604977248467, 2.425000002731188875, -28.56700777964554305 ) ) ;
#261 = CARTESIAN_POINT ( 'NONE',  ( 23.41746825000000243, 19.02499999726880375, 7.608796670333735079 ) ) ;
#262 = CARTESIAN_POINT ( 'NONE',  ( 19.06425588902592239, 11.71913166759064318, 19.11951029504763611 ) ) ;
#263 = ORIENTED_EDGE ( 'NONE', *, *, #29784, .F. ) ;
#264 = CARTESIAN_POINT ( 'NONE',  ( 10.37757302488624767, 45.72500000273120691, 31.93888565452638417 ) ) ;
#265 = DIRECTION ( 'NONE',  ( 1.224646799147353454E-16, -1.000000000000000000, 0.000000000000000000 ) ) ;
#266 = ORIENTED_EDGE ( 'NONE', *, *, #7688, .T. ) ;
#267 = CARTESIAN_POINT ( 'NONE',  ( 28.01184896238290278, 44.08333333333332860, -7.505752307973347470 ) ) ;
#268 = CARTESIAN_POINT ( 'NONE',  ( 10.04305231718579705, 11.10000000546237864, 30.90933677959248982 ) ) ;
#269 = CARTESIAN_POINT ( 'NONE',  ( 10.04305231718578817, 5.900000005462382902, -30.90933677959249337 ) ) ;
#270 = CARTESIAN_POINT ( 'NONE',  ( -32.50000000000000000, 72.00000000000001421, 0.000000000000000000 ) ) ;
#271 = CARTESIAN_POINT ( 'NONE',  ( -28.01184896238304134, 25.46354166666666430, -7.505752307972844761 ) ) ;
#272 = CARTESIAN_POINT ( 'NONE',  ( 7.570916362186213000, 0.4000000000000114575, -23.30088464923126423 ) ) ;
#273 = CARTESIAN_POINT ( 'NONE',  ( -20.75514604977248112, 11.67500000273118843, 28.56700777964554661 ) ) ;
#274 = CARTESIAN_POINT ( 'NONE',  ( 32.50000000000000711, 60.89999999999999147, 10.55989012756945122 ) ) ;
#275 = CARTESIAN_POINT ( 'NONE',  ( -11.25946833292375793, 77.07500000273121543, 8.180482586598737171 ) ) ;
#276 = CARTESIAN_POINT ( 'NONE',  ( 32.50000000000000711, 73.40000000546235981, 10.55989012756945122 ) ) ;
#277 = CARTESIAN_POINT ( 'NONE',  ( -20.53372385742107653, 31.18711833240935150, -20.47846945139867003 ) ) ;
#278 = CARTESIAN_POINT ( 'NONE',  ( 13.91746825000000065, 76.27500000273118985, 4.522059556121114987 ) ) ;
#279 = CARTESIAN_POINT ( 'NONE',  ( -20.50609665441004736, 53.25000000000000000, -20.50609665440969565 ) ) ;
#280 = PRODUCT_CONTEXT ( 'NONE', #6136, 'mechanical' ) ;
#281 = FACE_OUTER_BOUND ( 'NONE', #10068, .T. ) ;
#282 = CARTESIAN_POINT ( 'NONE',  ( 4.445600272181915325E-13, 15.49999999999999822, -32.50000000000000000 ) ) ;
#283 = CARTESIAN_POINT ( 'NONE',  ( -20.08610463437156923, 4.300000000000009592, 27.64615127144130113 ) ) ;
#284 = DIRECTION ( 'NONE',  ( -1.224646799147353454E-16, 1.000000000000000000, -0.000000000000000000 ) ) ;
#285 = CARTESIAN_POINT ( 'NONE',  ( 6.950374756619257965, 62.69753499907601224, -26.09010956794244507 ) ) ;
#286 = CARTESIAN_POINT ( 'NONE',  ( -10.37757302488623701, 43.52500000273118275, 31.93888565452638417 ) ) ;
#287 = CARTESIAN_POINT ( 'NONE',  ( 15.00000000000000355, 71.15000000546237402, 4.873795443493592394 ) ) ;
#288 = CARTESIAN_POINT ( 'NONE',  ( 27.16883889988623935, 56.57500000273117990, -19.73931689729374384 ) ) ;
#289 = CARTESIAN_POINT ( 'NONE',  ( -27.16883889988624290, 35.17500000273118843, -19.73931689729374028 ) ) ;
#290 = CARTESIAN_POINT ( 'NONE',  ( 32.50000000000000000, 24.99999999999999289, -3.980102097228898626E-15 ) ) ;
#291 = CARTESIAN_POINT ( 'NONE',  ( -19.09188309203660694, 18.01562499999999645, 19.09188309203694800 ) ) ;
#292 = CARTESIAN_POINT ( 'NONE',  ( -19.82091636218621389, 9.199999999999985079, 14.40073868116558842 ) ) ;
#293 = ADVANCED_FACE ( 'NONE', ( #15638 ), #7725, .F. ) ;
#294 = CARTESIAN_POINT ( 'NONE',  ( 5.270191272235265068, 16.99999999999999645, -22.91526030449972851 ) ) ;
#295 = CARTESIAN_POINT ( 'NONE',  ( -26.29305231718578995, 76.20000000000000284, 19.10302069950538595 ) ) ;
#296 = CARTESIAN_POINT ( 'NONE',  ( -33.58253175000000113, 15.22500000273119447, 10.91162601494193929 ) ) ;
#297 = CARTESIAN_POINT ( 'NONE',  ( 14.47279130897151944, 0.9249999972688209837, -19.92008829642072598 ) ) ;
#298 = CARTESIAN_POINT ( 'NONE',  ( -32.50000000000000000, 39.89999999999999147, -10.55989012756945300 ) ) ;
#299 = CARTESIAN_POINT ( 'NONE',  ( -7.025853678916861966, 17.72357666574268720, -26.06988505166722803 ) ) ;
#300 = CARTESIAN_POINT ( 'NONE',  ( -2.092463501923844636E-15, 36.00000000546238255, -34.17252228774368916 ) ) ;
#301 = DIRECTION ( 'NONE',  ( 0.000000000000000000, 0.000000000000000000, -1.000000000000000000 ) ) ;
#302 = CARTESIAN_POINT ( 'NONE',  ( -20.75514604977248112, 21.42500000273119909, 28.56700777964554661 ) ) ;
#303 = CARTESIAN_POINT ( 'NONE',  ( 19.09188309203694800, 48.09375000000000000, 19.09188309203660694 ) ) ;
#304 = EDGE_LOOP ( 'NONE', ( #18948, #25383, #642, #30344 ) ) ;
#305 = CARTESIAN_POINT ( 'NONE',  ( 27.16883889988623935, 62.32500000273120833, -19.73931689729374384 ) ) ;
#306 = ORIENTED_EDGE ( 'NONE', *, *, #17553, .T. ) ;
#307 = CARTESIAN_POINT ( 'NONE',  ( -30.02300923189239512, 15.00781249999999467, 2.654126918244515359E-13 ) ) ;
#308 = CARTESIAN_POINT ( 'NONE',  ( -25.98046417659859486, 13.29465250092397532, -15.04653450569291628 ) ) ;
#309 = CARTESIAN_POINT ( 'NONE',  ( 10.37757302488624767, 3.725000002731182480, 31.93888565452638417 ) ) ;
#310 = ORIENTED_EDGE ( 'NONE', *, *, #3089, .T. ) ;
#311 = DIRECTION ( 'NONE',  ( -0.000000000000000000, -1.000000000000000000, -0.000000000000000000 ) ) ;
#312 = CARTESIAN_POINT ( 'NONE',  ( 20.75514604977248467, 26.67500000273118133, -28.56700777964554305 ) ) ;
#313 = CARTESIAN_POINT ( 'NONE',  ( -32.50000000000000000, 36.50000000546238255, 0.000000000000000000 ) ) ;
#314 = MECHANICAL_DESIGN_GEOMETRIC_PRESENTATION_REPRESENTATION (  '', ( #29900 ), #24959 ) ;
#315 = DIRECTION ( 'NONE',  ( -0.000000000000000000, -1.000000000000000000, -0.000000000000000000 ) ) ;
#316 = CARTESIAN_POINT ( 'NONE',  ( 5.779280353836490358E-15, 76.49999999999998579, 32.49999999999999289 ) ) ;
#317 = CARTESIAN_POINT ( 'NONE',  ( 10.37757302488624767, 39.97500000273118559, 31.93888565452638417 ) ) ;
#318 = SURFACE_SIDE_STYLE ('',( #28646 ) ) ;
#319 = ADVANCED_FACE ( 'NONE', ( #18042 ), #31233, .T. ) ;
#320 = CARTESIAN_POINT ( 'NONE',  ( -32.50000000000000000, 19.90000000000001279, -10.55989012756945478 ) ) ;
#321 = CARTESIAN_POINT ( 'NONE',  ( -32.50000000000000000, 23.90000000000000213, -10.55989012756945478 ) ) ;
#322 = CARTESIAN_POINT ( 'NONE',  ( -7.570916362186215665, 7.399999999999989697, 23.30088464923126423 ) ) ;
#323 = CARTESIAN_POINT ( 'NONE',  ( 27.16883889988623935, 68.32500000273117280, -19.73931689729374384 ) ) ;
#324 = CARTESIAN_POINT ( 'NONE',  ( -20.18813247507404185, 67.00000000000005684, 25.94218825114890237 ) ) ;
#325 = CARTESIAN_POINT ( 'NONE',  ( 6.987025175984479475, 74.00000000000002842, -12.51940829596972016 ) ) ;
#326 = CARTESIAN_POINT ( 'NONE',  ( -2.162160676586882350E-15, 54.87500000273119838, -35.31076352940722529 ) ) ;
#327 = CARTESIAN_POINT ( 'NONE',  ( -23.41746824999999887, 1.624999997268811169, -2.867812753649727150E-15 ) ) ;
#328 = ADVANCED_FACE ( 'NONE', ( #23862 ), #25917, .T. ) ;
#329 = CARTESIAN_POINT ( 'NONE',  ( 32.50000000000000000, 7.500000005462359454, -3.980102097228898626E-15 ) ) ;
#330 = CARTESIAN_POINT ( 'NONE',  ( 20.75514604977249178, 11.82500000273118346, 28.56700777964553950 ) ) ;
#331 = CARTESIAN_POINT ( 'NONE',  ( 13.94119854578937812, 25.61236083425731636, 24.22776226481240514 ) ) ;
#332 = CARTESIAN_POINT ( 'NONE',  ( 2.357955684373970406, 67.00000000000001421, -33.24972188832315823 ) ) ;
#333 = DIRECTION ( 'NONE',  ( -0.000000000000000000, -1.000000000000000000, -0.000000000000000000 ) ) ;
#334 = CARTESIAN_POINT ( 'NONE',  ( -33.58253175000000113, 37.12500000273118417, 0.000000000000000000 ) ) ;
#335 = CARTESIAN_POINT ( 'NONE',  ( 0.000000000000000000, 74.00000000000001421, 0.000000000000000000 ) ) ;
#336 = PLANE ( 'NONE',  #21046 ) ;
#337 = EDGE_CURVE ( 'NONE', #9595, #9120, #6660, .T. ) ;
#338 = CARTESIAN_POINT ( 'NONE',  ( -4.300734207923759378, 76.47500000273116427, -13.23629886949340495 ) ) ;
#339 = CARTESIAN_POINT ( 'NONE',  ( 30.02300923189239867, 42.78868083240935505, -0.04044903255044467877 ) ) ;
#340 = CARTESIAN_POINT ( 'NONE',  ( 32.50000000000000000, 51.60000000546239107, -10.55989012756945833 ) ) ;
#341 = CARTESIAN_POINT ( 'NONE',  ( -13.91746824999999887, 75.37500000273116996, 0.000000000000000000 ) ) ;
#342 = SURFACE_STYLE_FILL_AREA ( #7570 ) ;
#343 = CARTESIAN_POINT ( 'NONE',  ( 13.97622843553633665, 13.86197916666666430, 24.20753774853730889 ) ) ;
#344 =( BOUNDED_CURVE ( )  B_SPLINE_CURVE ( 2, ( #18329, #28774, #33583, #26207, #28942, #8342, #10762, #18832, #29443, #10593, #13679, #5610, #16585 ),
 .UNSPECIFIED., .F., .T. ) 
 B_SPLINE_CURVE_WITH_KNOTS ( ( 3, 2, 2, 2, 2, 2, 3 ),
 ( 0.2628205128205128305, 0.2641025641025641080, 0.2666666666666666630, 0.2692307692307692180, 0.2717948717948717730, 0.2743589743589743835, 0.2756410256410256610 ),
 .UNSPECIFIED. ) 
 CURVE ( )  GEOMETRIC_REPRESENTATION_ITEM ( )  RATIONAL_B_SPLINE_CURVE ( ( 0.9755282581475768211, 0.9755282581475768211, 1.000000000000000000, 0.9510565162951535312, 1.000000000000000000, 0.9510565162951535312, 1.000000000000000000, 0.9510565162951535312, 1.000000000000000000, 0.9510565162951535312, 1.000000000000000000, 0.9755282581475768211, 0.9755282581475768211 ) ) 
 REPRESENTATION_ITEM ( '' )  );
#345 = CARTESIAN_POINT ( 'NONE',  ( -2.092463501923844636E-15, 68.00000000546236834, -34.17252228774368916 ) ) ;
#346 = CARTESIAN_POINT ( 'NONE',  ( -7.505752307972844761, 21.16666666666666430, 28.01184896238304134 ) ) ;
#347 = CARTESIAN_POINT ( 'NONE',  ( -20.75514604977248112, 27.67500000273118133, 28.56700777964554661 ) ) ;
#348 =( BOUNDED_CURVE ( )  B_SPLINE_CURVE ( 2, ( #28685, #12736, #2613, #13, #28179, #10501, #4666, #28512, #9994, #20980, #17898, #2090, #20467 ),
 .UNSPECIFIED., .F., .T. ) 
 B_SPLINE_CURVE_WITH_KNOTS ( ( 3, 2, 2, 2, 2, 2, 3 ),
 ( 0.1944444444444444475, 0.2000000000000000111, 0.2111111111111111105, 0.2222222222222222099, 0.2333333333333333370, 0.2444444444444444364, 0.2500000000000000000 ),
 .UNSPECIFIED. ) 
 CURVE ( )  GEOMETRIC_REPRESENTATION_ITEM ( )  RATIONAL_B_SPLINE_CURVE ( ( 0.9755282581475768211, 0.9755282581475768211, 1.000000000000000000, 0.9510565162951535312, 1.000000000000000000, 0.9510565162951535312, 1.000000000000000000, 0.9510565162951535312, 1.000000000000000000, 0.9510565162951535312, 1.000000000000000000, 0.9755282581475767101, 0.9755282581475768211 ) ) 
 REPRESENTATION_ITEM ( '' )  );
#349 = CYLINDRICAL_SURFACE ( 'NONE', #12439, 32.50000000000000000 ) ;
#350 = ORIENTED_EDGE ( 'NONE', *, *, #18271, .F. ) ;
#351 = CARTESIAN_POINT ( 'NONE',  ( -26.02091320914849959, 36.78423583425730214, 14.97647472619947528 ) ) ;
#352 = CARTESIAN_POINT ( 'NONE',  ( -20.08610463437157989, 16.20000000546237118, -27.64615127144129758 ) ) ;
#353 = CARTESIAN_POINT ( 'NONE',  ( -28.01184896238304134, 52.96354166666666430, -7.505752307972844761 ) ) ;
#354 = CARTESIAN_POINT ( 'NONE',  ( -10.04305231718579172, 35.59999999999999432, -30.90933677959248982 ) ) ;
#355 = CARTESIAN_POINT ( 'NONE',  ( 6.486482029760649416E-15, 51.87500000273119127, 35.31076352940723240 ) ) ;
#356 = CARTESIAN_POINT ( 'NONE',  ( -20.08610463437157989, 58.20000000546238539, -27.64615127144129758 ) ) ;
#357 = CARTESIAN_POINT ( 'NONE',  ( -11.25946833292375793, 77.17500000273119554, -8.180482586598733619 ) ) ;
#358 = CARTESIAN_POINT ( 'NONE',  ( -20.75514604977248823, 32.82500000273118701, -28.56700777964554305 ) ) ;
#359 = CARTESIAN_POINT ( 'NONE',  ( 5.779280353836490358E-15, 54.49999999999999289, 32.49999999999999289 ) ) ;
#360 = CARTESIAN_POINT ( 'NONE',  ( 10.37757302488624056, 60.77500000273117564, -31.93888565452638417 ) ) ;
#361 =( LENGTH_UNIT ( ) NAMED_UNIT ( * ) SI_UNIT ( .MILLI., .METRE. ) );
#362 = CARTESIAN_POINT ( 'NONE',  ( -2.162160676586882350E-15, 52.62500000273117706, -35.31076352940722529 ) ) ;
#363 = CARTESIAN_POINT ( 'NONE',  ( 7.505752307972854531, 22.88541666666666430, -28.01184896238303423 ) ) ;
#364 = CARTESIAN_POINT ( 'NONE',  ( -10.04305231718579172, 37.59999999999999432, -30.90933677959248982 ) ) ;
#365 = CARTESIAN_POINT ( 'NONE',  ( -23.41746825000000243, 7.524999997268816188, -7.608796670333730638 ) ) ;
#366 = CARTESIAN_POINT ( 'NONE',  ( 27.16883889988624290, 8.175000002731191984, 19.73931689729373673 ) ) ;
#367 = CARTESIAN_POINT ( 'NONE',  ( 32.50000000000000711, 35.40000000546237402, 10.55989012756945122 ) ) ;
#368 = CARTESIAN_POINT ( 'NONE',  ( -0.04044903255042732459, 35.05430583240935505, -27.95245687107223986 ) ) ;
#369 = CARTESIAN_POINT ( 'NONE',  ( -4.300734207923759378, 72.97500000273119269, -13.23629886949340495 ) ) ;
#370 = CARTESIAN_POINT ( 'NONE',  ( -10.37757302488623701, 71.77500000273117564, 31.93888565452638417 ) ) ;
#371 = CARTESIAN_POINT ( 'NONE',  ( -4.000000000000003553, 0.000000000000000000, 16.50000000000002842 ) ) ;
#372 = CARTESIAN_POINT ( 'NONE',  ( 27.16883889988623935, 68.57500000273118701, -19.73931689729374384 ) ) ;
#373 = ORIENTED_EDGE ( 'NONE', *, *, #30700, .F. ) ;
#374 = CIRCLE ( 'NONE', #19015, 10.72870458603808075 ) ;
#375 = CARTESIAN_POINT ( 'NONE',  ( 7.236395654485755280, 18.72499999726881370, 22.27133577429736988 ) ) ;
#376 = CARTESIAN_POINT ( 'NONE',  ( -24.20753774853730889, 62.84635416666667851, 13.97622843553633842 ) ) ;
#377 = CARTESIAN_POINT ( 'NONE',  ( -33.58253175000000113, 55.22500000273117848, 10.91162601494193929 ) ) ;
#378 = CARTESIAN_POINT ( 'NONE',  ( -20.75514604977248823, 15.07500000273116747, -28.56700777964554305 ) ) ;
#379 = CARTESIAN_POINT ( 'NONE',  ( 33.58253175000000113, 4.475000002731183812, -10.91162601494193751 ) ) ;
#380 = CARTESIAN_POINT ( 'NONE',  ( -27.95245687107223276, 42.50781249999998579, 2.498001805406602216E-13 ) ) ;
#381 = CARTESIAN_POINT ( 'NONE',  ( 0.04044903254992426173, 31.05506916759064495, -30.02300923189239867 ) ) ;
#382 = AXIS2_PLACEMENT_3D ( 'NONE', #6259, #3850, #8998 ) ;
#383 = CARTESIAN_POINT ( 'NONE',  ( -20.47846945139866648, 23.45274333240935150, 20.53372385742108008 ) ) ;
#384 = CARTESIAN_POINT ( 'NONE',  ( -2.092463501923844636E-15, 74.00000000546236834, -34.17252228774368916 ) ) ;
#385 = CARTESIAN_POINT ( 'NONE',  ( -10.04305231718578462, 56.90000000546238823, 30.90933677959249337 ) ) ;
#386 = CARTESIAN_POINT ( 'NONE',  ( 20.75514604977248467, 40.42500000273118133, -28.56700777964554305 ) ) ;
#387 = CARTESIAN_POINT ( 'NONE',  ( -19.06425588902558133, 44.07774333240935505, 19.11951029504797006 ) ) ;
#388 = FACE_OUTER_BOUND ( 'NONE', #6392, .T. ) ;
#389 = CYLINDRICAL_SURFACE ( 'NONE', #32540, 24.50000000000000000 ) ;
#390 = VERTEX_POINT ( 'NONE', #7896 ) ;
#391 = CARTESIAN_POINT ( 'NONE',  ( 6.486482029760649416E-15, 47.87500000273117706, 35.31076352940723240 ) ) ;
#392 = CARTESIAN_POINT ( 'NONE',  ( 5.147494310547426899, 51.44874571845315359, -32.50000000000000000 ) ) ;
#393 = CARTESIAN_POINT ( 'NONE',  ( 26.09010956794232428, 52.39621500092398065, -6.950374756619718042 ) ) ;
#394 = CARTESIAN_POINT ( 'NONE',  ( 33.58253175000000113, 68.37500000273119838, -4.112674001490185761E-15 ) ) ;
#395 = ORIENTED_EDGE ( 'NONE', *, *, #27322, .F. ) ;
#396 = CARTESIAN_POINT ( 'NONE',  ( -33.58253175000000113, 19.22500000273118204, 10.91162601494193929 ) ) ;
#397 = CARTESIAN_POINT ( 'NONE',  ( -7.505752307972844761, 28.04166666666666075, 28.01184896238304134 ) ) ;
#398 = ORIENTED_EDGE ( 'NONE', *, *, #26853, .F. ) ;
#399 = CARTESIAN_POINT ( 'NONE',  ( 33.58253175000000113, 60.12500000273119127, -4.112674001490185761E-15 ) ) ;
#400 = CARTESIAN_POINT ( 'NONE',  ( -15.01150461594595775, 45.37239583333333570, 26.00068869287368756 ) ) ;
#401 = CONICAL_SURFACE ( 'NONE', #22876, 24.50000000000000000, 0.7853981633974463916 ) ;
#402 = CARTESIAN_POINT ( 'NONE',  ( 26.29305231718578995, 19.70000000546237473, -19.10302069950538240 ) ) ;
#403 = CARTESIAN_POINT ( 'NONE',  ( 24.50000000000000355, 16.09999999999998366, -7.960532557706203605 ) ) ;
#404 = CARTESIAN_POINT ( 'NONE',  ( -18.94512977948575738, 7.924999997268811214, -13.76444248337723231 ) ) ;
#405 = CARTESIAN_POINT ( 'NONE',  ( 10.37757302488624767, 29.97500000273117848, 31.93888565452638417 ) ) ;
#406 = CARTESIAN_POINT ( 'NONE',  ( -1.053607264507113999E-13, 64.50000000000000000, 32.50000000000000711 ) ) ;
#407 = CARTESIAN_POINT ( 'NONE',  ( -26.02091320914878025, 65.41888916574268364, -14.97647472619899389 ) ) ;
#408 = CARTESIAN_POINT ( 'NONE',  ( -1.137977401836464321E-14, 52.00000000000000711, 46.18802153517007270 ) ) ;
#409 = CARTESIAN_POINT ( 'NONE',  ( 11.25946833292375793, 78.07500000273121543, -8.180482586598735395 ) ) ;
#410 = CARTESIAN_POINT ( 'NONE',  ( 5.779280353836490358E-15, 4.500000000000003553, 32.49999999999999289 ) ) ;
#411 = CARTESIAN_POINT ( 'NONE',  ( -10.04305231718578462, 16.40000000000001279, 30.90933677959249337 ) ) ;
#412 = CARTESIAN_POINT ( 'NONE',  ( -6.988114217767819270, 62.41666666666666430, 26.07999730980490583 ) ) ;
#413 = CARTESIAN_POINT ( 'NONE',  ( -18.94512977948576093, 2.324999997268817342, 13.76444248337722698 ) ) ;
#414 = CARTESIAN_POINT ( 'NONE',  ( -8.960552108402742093E-16, 78.37500000273116996, -14.63369212191046387 ) ) ;
#415 = CARTESIAN_POINT ( 'NONE',  ( -6.988114217767819270, 31.47916666666666075, 26.07999730980490583 ) ) ;
#416 = CARTESIAN_POINT ( 'NONE',  ( 20.75514604977248467, 24.42500000273119554, -28.56700777964554305 ) ) ;
#417 = CARTESIAN_POINT ( 'NONE',  ( -20.75514604977248112, 71.42500000273119554, 28.56700777964554661 ) ) ;
#418 = CARTESIAN_POINT ( 'NONE',  ( 33.58253175000000113, 36.37500000273118417, -4.112674001490185761E-15 ) ) ;
#419 = CARTESIAN_POINT ( 'NONE',  ( -10.37757302488623701, 17.77500000273118985, 31.93888565452638417 ) ) ;
#420 = CARTESIAN_POINT ( 'NONE',  ( -26.06988505166735237, 54.40142333425730925, -7.025853678916388567 ) ) ;
#421 = CARTESIAN_POINT ( 'NONE',  ( 10.37757302488624056, 72.52500000273120406, -31.93888565452638417 ) ) ;
#422 = CARTESIAN_POINT ( 'NONE',  ( 32.50000000000000000, 3.600000005462360431, -10.55989012756945833 ) ) ;
#423 = EDGE_CURVE ( 'NONE', #5175, #29096, #19145, .T. ) ;
#424 = CARTESIAN_POINT ( 'NONE',  ( 20.08610463437157279, 51.29999999999997584, -27.64615127144129758 ) ) ;
#425 = CYLINDRICAL_SURFACE ( 'NONE', #30310, 32.50000000000000000 ) ;
#426 = CARTESIAN_POINT ( 'NONE',  ( 33.58253175000000823, 58.02500000273117564, 10.91162601494192685 ) ) ;
#427 = EDGE_CURVE ( 'NONE', #23800, #20505, #26160, .T. ) ;
#428 = CARTESIAN_POINT ( 'NONE',  ( 18.94512977948575738, 14.92499999726881654, 13.76444248337723408 ) ) ;
#429 = CIRCLE ( 'NONE', #33304, 4.000000000000014211 ) ;
#430 = EDGE_LOOP ( 'NONE', ( #16909, #1055, #4151, #23333 ) ) ;
#431 = CARTESIAN_POINT ( 'NONE',  ( -33.58253175000000113, 67.37500000273121259, 0.000000000000000000 ) ) ;
#432 = CARTESIAN_POINT ( 'NONE',  ( 1.836970198721029589E-15, 86.00000000000001421, -15.00000000000000000 ) ) ;
#433 = CARTESIAN_POINT ( 'NONE',  ( 23.41746825000000243, 2.724999997268822138, -7.608796670333727974 ) ) ;
#434 = CARTESIAN_POINT ( 'NONE',  ( 27.95245687107223986, 25.03944416759064495, 0.04044903254993640479 ) ) ;
#435 = ORIENTED_EDGE ( 'NONE', *, *, #9249, .F. ) ;
#436 = CARTESIAN_POINT ( 'NONE',  ( -20.75514604977248823, 38.82500000273120122, -28.56700777964554305 ) ) ;
#437 = CARTESIAN_POINT ( 'NONE',  ( -10.04305231718579172, 42.10000000546237686, -30.90933677959248982 ) ) ;
#438 = VERTEX_POINT ( 'NONE', #27093 ) ;
#439 = CARTESIAN_POINT ( 'NONE',  ( -28.01184896238304134, 46.08854166666666430, -7.505752307972844761 ) ) ;
#440 = CARTESIAN_POINT ( 'NONE',  ( 32.50000000000000000, 11.60000000546236976, -10.55989012756945833 ) ) ;
#441 = CARTESIAN_POINT ( 'NONE',  ( -4.223320258572819786E-15, 3.499999999999996891, 24.50000000000000000 ) ) ;
#442 = CARTESIAN_POINT ( 'NONE',  ( -7.505752307973343918, 19.16145833333332860, -28.01184896238290989 ) ) ;
#443 = CARTESIAN_POINT ( 'NONE',  ( -15.14183272437241889, 0.7000000000000070610, -20.84094480462497856 ) ) ;
#444 = CARTESIAN_POINT ( 'NONE',  ( 33.58253175000000113, 10.47500000273119802, -10.91162601494193751 ) ) ;
#445 =( BOUNDED_CURVE ( )  B_SPLINE_CURVE ( 2, ( #6317, #10970, #27082, #6487, #8556, #26754, #24016, #26913, #19534, #11627, #31888, #19040, #21445 ),
 .UNSPECIFIED., .F., .T. ) 
 B_SPLINE_CURVE_WITH_KNOTS ( ( 3, 2, 2, 2, 2, 2, 3 ),
 ( 0.5192307692307692735, 0.5205128205128205510, 0.5230769230769231060, 0.5256410256410256610, 0.5282051282051282159, 0.5307692307692307709, 0.5320512820512820484 ),
 .UNSPECIFIED. ) 
 CURVE ( )  GEOMETRIC_REPRESENTATION_ITEM ( )  RATIONAL_B_SPLINE_CURVE ( ( 0.9755282581475768211, 0.9755282581475768211, 1.000000000000000000, 0.9510565162951535312, 1.000000000000000000, 0.9510565162951535312, 1.000000000000000000, 0.9510565162951535312, 1.000000000000000000, 0.9510565162951535312, 1.000000000000000000, 0.9755282581475768211, 0.9755282581475768211 ) ) 
 REPRESENTATION_ITEM ( '' )  );
#446 = CARTESIAN_POINT ( 'NONE',  ( 26.29305231718579350, 60.79999999999999005, 19.10302069950537529 ) ) ;
#447 = CARTESIAN_POINT ( 'NONE',  ( 11.25946833292375793, 78.07500000273121543, -8.180482586598735395 ) ) ;
#448 = CARTESIAN_POINT ( 'NONE',  ( 3.000384657911015469E-15, 0.000000000000000000, -24.50000000000000000 ) ) ;
#449 = CARTESIAN_POINT ( 'NONE',  ( -7.468012846824272799, 36.91628499907601224, 28.02196122052058413 ) ) ;
#450 = CARTESIAN_POINT ( 'NONE',  ( -11.25946833292375793, 77.57500000273121543, 8.180482586598737171 ) ) ;
#451 = CARTESIAN_POINT ( 'NONE',  ( -26.00068869287340334, 49.09635416666666430, 15.01150461594643559 ) ) ;
#452 = CONTEXT_DEPENDENT_SHAPE_REPRESENTATION ( #10566, #17237 ) ;
#453 = LINE ( 'NONE', #5276, #30284 ) ;
#454 = CARTESIAN_POINT ( 'NONE',  ( 32.50000000000000000, 65.10000000000000853, -10.55989012756945833 ) ) ;
#455 = CARTESIAN_POINT ( 'NONE',  ( -33.58253175000000113, 79.37500000273118417, 0.000000000000000000 ) ) ;
#456 = CARTESIAN_POINT ( 'NONE',  ( -5.147494310547430452, 54.05125428700921475, -32.49999999999999289 ) ) ;
#457 = CARTESIAN_POINT ( 'NONE',  ( 26.06988505166722803, 63.27045166574269075, -7.025853678916862854 ) ) ;
#458 = CARTESIAN_POINT ( 'NONE',  ( -10.37757302488624411, 44.72500000273119269, -31.93888565452638417 ) ) ;
#459 = CARTESIAN_POINT ( 'NONE',  ( 2.688165632520823219E-15, 79.37500000273116996, 14.63369212191046387 ) ) ;
#460 = CARTESIAN_POINT ( 'NONE',  ( -2.162160676586881955E-15, 56.87500000273117706, -35.31076352940723240 ) ) ;
#461 = CARTESIAN_POINT ( 'NONE',  ( 20.75514604977249178, 36.07500000273117990, 28.56700777964553950 ) ) ;
#462 = CARTESIAN_POINT ( 'NONE',  ( 20.08610463437157279, 23.80000000546236194, -27.64615127144129758 ) ) ;
#463 = CARTESIAN_POINT ( 'NONE',  ( 19.09188309203694800, 24.03124999999999645, 19.09188309203660694 ) ) ;
#464 = DIRECTION ( 'NONE',  ( -1.000000000000000000, 0.000000000000000000, 0.000000000000000000 ) ) ;
#465 = CARTESIAN_POINT ( 'NONE',  ( -32.50000000000000000, 44.40000000546238113, -10.55989012756945300 ) ) ;
#466 = CARTESIAN_POINT ( 'NONE',  ( 26.29305231718579350, 74.80000000000002558, 19.10302069950537529 ) ) ;
#467 = CARTESIAN_POINT ( 'NONE',  ( 20.75514604977248467, 6.425000002731192872, -28.56700777964554305 ) ) ;
#468 = CARTESIAN_POINT ( 'NONE',  ( -14.47279130897152299, 5.924999997268808549, 19.92008829642072243 ) ) ;
#469 = CARTESIAN_POINT ( 'NONE',  ( -24.50000000000000000, 10.74999999453762811, -3.000384657911015469E-15 ) ) ;
#470 = CARTESIAN_POINT ( 'NONE',  ( -19.06425588902558133, 26.89024333240934439, 19.11951029504797006 ) ) ;
#471 = CARTESIAN_POINT ( 'NONE',  ( -15.00000000000000000, 76.25000000546239676, 0.000000000000000000 ) ) ;
#472 = CARTESIAN_POINT ( 'NONE',  ( 20.75514604977248467, 20.42500000273120264, -28.56700777964554305 ) ) ;
#473 = CARTESIAN_POINT ( 'NONE',  ( -13.97622843553588901, 48.80989583333332860, 24.20753774853756823 ) ) ;
#474 = ORIENTED_EDGE ( 'NONE', *, *, #17841, .F. ) ;
#475 = CARTESIAN_POINT ( 'NONE',  ( -10.37757302488624411, 60.72500000273119269, -31.93888565452638417 ) ) ;
#476 = VERTEX_POINT ( 'NONE', #13893 ) ;
#477 = CARTESIAN_POINT ( 'NONE',  ( 28.01184896238304134, 16.86979166666666075, 7.505752307972846538 ) ) ;
#478 = CARTESIAN_POINT ( 'NONE',  ( -7.543491769121417612, 15.72954833425730925, 28.00173670424549499 ) ) ;
#479 = CARTESIAN_POINT ( 'NONE',  ( 27.16883889988623935, 2.325000002731183901, -19.73931689729374384 ) ) ;
#480 = EDGE_CURVE ( 'NONE', #3734, #23926, #32237, .T. ) ;
#481 = ORIENTED_EDGE ( 'NONE', *, *, #22056, .T. ) ;
#482 = CARTESIAN_POINT ( 'NONE',  ( -18.94512977948576093, 1.824999997268816898, 13.76444248337722698 ) ) ;
#483 = CARTESIAN_POINT ( 'NONE',  ( -20.75514604977248112, 25.67500000273118488, 28.56700777964554661 ) ) ;
#484 =( BOUNDED_CURVE ( )  B_SPLINE_CURVE ( 2, ( #8782, #6212, #1213, #29708, #6384, #19601, #24574, #27149, #3642, #11694, #1046, #11526, #32454 ),
 .UNSPECIFIED., .F., .F. ) 
 B_SPLINE_CURVE_WITH_KNOTS ( ( 3, 2, 2, 2, 2, 2, 3 ),
 ( 0.9166666666666666297, 0.9222222222222222765, 0.9333333333333333481, 0.9444444444444444198, 0.9555555555555556024, 0.9666666666666666741, 0.9722222222222222099 ),
 .UNSPECIFIED. ) 
 CURVE ( )  GEOMETRIC_REPRESENTATION_ITEM ( )  RATIONAL_B_SPLINE_CURVE ( ( 0.9755282581475768211, 0.9755282581475765991, 1.000000000000000000, 0.9510565162951535312, 1.000000000000000000, 0.9510565162951535312, 1.000000000000000000, 0.9510565162951535312, 1.000000000000000000, 0.9510565162951535312, 1.000000000000000000, 0.9755282581475768211, 0.9755282581475768211 ) ) 
 REPRESENTATION_ITEM ( '' )  );
#485 = CARTESIAN_POINT ( 'NONE',  ( -26.29305231718579350, 32.30000000546237260, -19.10302069950537884 ) ) ;
#486 = CARTESIAN_POINT ( 'NONE',  ( -15.00000000000000000, 72.00000000000001421, 0.000000000000000000 ) ) ;
#487 = CARTESIAN_POINT ( 'NONE',  ( 26.29305231718579350, 52.80000000000001137, 19.10302069950537529 ) ) ;
#488 = CARTESIAN_POINT ( 'NONE',  ( -24.50000000000000711, 11.09999999999999787, 7.960532557706201828 ) ) ;
#489 = CARTESIAN_POINT ( 'NONE',  ( 10.37757302488624056, 44.77500000273118275, -31.93888565452638417 ) ) ;
#490 = CARTESIAN_POINT ( 'NONE',  ( 32.50000000000000000, 25.09999999999999432, -10.55989012756945833 ) ) ;
#491 = CARTESIAN_POINT ( 'NONE',  ( -2.092463501923844636E-15, 21.49999999999998934, -34.17252228774368916 ) ) ;
#492 = CARTESIAN_POINT ( 'NONE',  ( -24.50000000000000000, 5.000000000000004441, -3.000384657911015469E-15 ) ) ;
#493 = CARTESIAN_POINT ( 'NONE',  ( 20.75514604977248467, 64.42500000273116711, -28.56700777964554305 ) ) ;
#494 = CARTESIAN_POINT ( 'NONE',  ( -31.53731130704430541, 66.99999999999997158, -11.55439184653567253 ) ) ;
#495 = CARTESIAN_POINT ( 'NONE',  ( 10.52536686629071916, 74.00000000000000000, -9.403734997071314439 ) ) ;
#496 = CARTESIAN_POINT ( 'NONE',  ( 10.37757302488624056, 50.77500000273118985, -31.93888565452638417 ) ) ;
#497 = CARTESIAN_POINT ( 'NONE',  ( -23.41746824999999887, 5.624999997268814944, -2.867812753649727150E-15 ) ) ;
#498 = CARTESIAN_POINT ( 'NONE',  ( 6.001560367445586717E-15, 3.249999994537631665, 24.50000000000000000 ) ) ;
#499 = CARTESIAN_POINT ( 'NONE',  ( -27.16883889988623935, 5.325000002731172799, 19.73931689729374739 ) ) ;
#500 = CARTESIAN_POINT ( 'NONE',  ( -26.09010956794232428, 36.92746500092395934, 6.950374756619732253 ) ) ;
#501 = DIRECTION ( 'NONE',  ( -0.8660254037844385966, 0.000000000000000000, 0.5000000000000000000 ) ) ;
#502 = CARTESIAN_POINT ( 'NONE',  ( -4.374313548017133790, 52.00000000000000000, 33.03144926559792083 ) ) ;
#503 = CARTESIAN_POINT ( 'NONE',  ( -33.58253175000000113, 27.02500000273119696, -10.91162601494193218 ) ) ;
#504 = CARTESIAN_POINT ( 'NONE',  ( 10.04305231718578817, 65.40000000000000568, -30.90933677959249337 ) ) ;
#505 = CYLINDRICAL_SURFACE ( 'NONE', #10621, 24.50000000000000000 ) ;
#506 = PRODUCT_RELATED_PRODUCT_CATEGORY ( 'part', '', ( #32094 ) ) ;
#507 = CARTESIAN_POINT ( 'NONE',  ( 4.300734207923761154, 77.47500000273116427, 13.23629886949340495 ) ) ;
#508 = CARTESIAN_POINT ( 'NONE',  ( 26.02091320914876960, 53.38763916574269786, 14.97647472619900455 ) ) ;
#509 = CARTESIAN_POINT ( 'NONE',  ( 32.50000000000000000, 55.60000000546238397, -10.55989012756945833 ) ) ;
#510 = CARTESIAN_POINT ( 'NONE',  ( 11.25946833292375793, 72.17500000273119554, 8.180482586598731842 ) ) ;
#511 = CARTESIAN_POINT ( 'NONE',  ( 1.093617666956751375E-13, 61.50000000000000000, -32.50000000000000711 ) ) ;
#512 = CARTESIAN_POINT ( 'NONE',  ( 19.09188309203694800, 13.71874999999999467, 19.09188309203660694 ) ) ;
#513 = CARTESIAN_POINT ( 'NONE',  ( -10.04305231718578462, 70.90000000546237402, 30.90933677959249337 ) ) ;
#514 = CARTESIAN_POINT ( 'NONE',  ( -15.01150461594595775, 17.87239583333332149, 26.00068869287368756 ) ) ;
#515 = CARTESIAN_POINT ( 'NONE',  ( -4.523095164977117273E-15, 16.62499999726881583, 24.62258325217400312 ) ) ;
#516 = ORIENTED_EDGE ( 'NONE', *, *, #16090, .F. ) ;
#517 = CARTESIAN_POINT ( 'NONE',  ( 28.02196122052045268, 42.08371500092398065, -7.468012846824774620 ) ) ;
#518 = CARTESIAN_POINT ( 'NONE',  ( -20.08610463437157989, 18.20000000546239605, -27.64615127144129758 ) ) ;
#519 = CARTESIAN_POINT ( 'NONE',  ( 28.01184896238304134, 51.24479166666666430, 7.505752307972846538 ) ) ;
#520 = CARTESIAN_POINT ( 'NONE',  ( -26.00068869287340334, 66.28385416666662877, 15.01150461594643382 ) ) ;
#521 = CARTESIAN_POINT ( 'NONE',  ( -10.37757302488623701, 47.77500000273118985, 31.93888565452638417 ) ) ;
#522 = CARTESIAN_POINT ( 'NONE',  ( -32.50000000000000000, 56.40000000546238113, -10.55989012756945478 ) ) ;
#523 = CARTESIAN_POINT ( 'NONE',  ( 11.25946833292375793, 78.17500000273119554, 8.180482586598731842 ) ) ;
#524 = CARTESIAN_POINT ( 'NONE',  ( 33.58253175000000113, 36.22500000273119980, -10.91162601494193751 ) ) ;
#525 = CARTESIAN_POINT ( 'NONE',  ( 10.04305231718579705, 54.59999999999998010, 30.90933677959248982 ) ) ;
#526 = CARTESIAN_POINT ( 'NONE',  ( -27.16883889988623935, 61.57500000273119412, 19.73931689729374739 ) ) ;
#527 = CARTESIAN_POINT ( 'NONE',  ( 13.03261263866114206, 74.00000000000001421, 4.904499419084999090 ) ) ;
#528 = CARTESIAN_POINT ( 'NONE',  ( -10.37757302488623701, 57.52500000273118275, 31.93888565452638417 ) ) ;
#529 = CARTESIAN_POINT ( 'NONE',  ( 7.505752307973351023, 20.88020833333333215, 28.01184896238290278 ) ) ;
#530 = CARTESIAN_POINT ( 'NONE',  ( -32.50000000000000000, 41.89999999999999147, -10.55989012756945478 ) ) ;
#531 = CARTESIAN_POINT ( 'NONE',  ( -7.236395654485763274, 8.024999997268828622, 22.27133577429736633 ) ) ;
#532 = CARTESIAN_POINT ( 'NONE',  ( -10.37757302488624411, 4.975000002731183812, -31.93888565452638417 ) ) ;
#533 = CARTESIAN_POINT ( 'NONE',  ( 10.04305231718579705, 35.10000000546236976, 30.90933677959248982 ) ) ;
#534 = LINE ( 'NONE', #11021, #18280 ) ;
#535 = CARTESIAN_POINT ( 'NONE',  ( -27.16883889988624290, 71.17500000273119554, -19.73931689729374028 ) ) ;
#536 = CARTESIAN_POINT ( 'NONE',  ( 0.000000000000000000, 80.00000000000001421, -32.50000000000000000 ) ) ;
#537 = CARTESIAN_POINT ( 'NONE',  ( -33.58253175000000113, 67.47500000273117848, 10.91162601494193929 ) ) ;
#538 = ORIENTED_EDGE ( 'NONE', *, *, #24194, .T. ) ;
#539 = CARTESIAN_POINT ( 'NONE',  ( 14.47279130897151767, 17.42499999726882365, -19.92008829642072598 ) ) ;
#540 = CARTESIAN_POINT ( 'NONE',  ( -2.428612866367529427E-13, 60.55468749999999289, -27.95245687107222921 ) ) ;
#541 = CARTESIAN_POINT ( 'NONE',  ( 10.37757302488624056, 52.52500000273117564, -31.93888565452638417 ) ) ;
#542 = CARTESIAN_POINT ( 'NONE',  ( -20.75514604977248112, 11.67500000273118843, 28.56700777964554661 ) ) ;
#543 = CARTESIAN_POINT ( 'NONE',  ( 6.486482029760649416E-15, 5.875000002731183280, 35.31076352940723240 ) ) ;
#544 = CARTESIAN_POINT ( 'NONE',  ( -19.09188309203660694, 42.07812499999999289, 19.09188309203694800 ) ) ;
#545 =( BOUNDED_CURVE ( )  B_SPLINE_CURVE ( 2, ( #31536, #23134, #8029, #31023, #13353, #23827, #28284, #20753, #2715, #28961, #5457, #117, #10438 ),
 .UNSPECIFIED., .F., .T. ) 
 B_SPLINE_CURVE_WITH_KNOTS ( ( 3, 2, 2, 2, 2, 2, 3 ),
 ( 0.8012820512820513219, 0.8025641025641025994, 0.8051282051282051544, 0.8076923076923077094, 0.8102564102564102644, 0.8128205128205128194, 0.8141025641025640969 ),
 .UNSPECIFIED. ) 
 CURVE ( )  GEOMETRIC_REPRESENTATION_ITEM ( )  RATIONAL_B_SPLINE_CURVE ( ( 0.9755282581475768211, 0.9755282581475768211, 1.000000000000000000, 0.9510565162951535312, 1.000000000000000000, 0.9510565162951535312, 1.000000000000000000, 0.9510565162951535312, 1.000000000000000000, 0.9510565162951535312, 1.000000000000000000, 0.9755282581475768211, 0.9755282581475768211 ) ) 
 REPRESENTATION_ITEM ( '' )  );
#546 = CARTESIAN_POINT ( 'NONE',  ( -14.97647472619946285, 30.76861083425731280, -26.02091320914851025 ) ) ;
#547 = CARTESIAN_POINT ( 'NONE',  ( 7.468012846824281681, 18.01003499907601935, -28.02196122052058058 ) ) ;
#548 = CARTESIAN_POINT ( 'NONE',  ( -20.08610463437156923, 72.80000000546239391, 27.64615127144130113 ) ) ;
#549 = EDGE_CURVE ( 'NONE', #23152, #22342, #16936, .T. ) ;
#550 = CARTESIAN_POINT ( 'NONE',  ( -11.25946833292375793, 80.67500000273119554, -8.180482586598733619 ) ) ;
#551 =( BOUNDED_CURVE ( )  B_SPLINE_CURVE ( 2, ( #8336, #3034, #11096, #13507, #32180, #11259, #29937, #3529, #27205, #21735, #3205, #16579, #13673 ),
 .UNSPECIFIED., .F., .T. ) 
 B_SPLINE_CURVE_WITH_KNOTS ( ( 3, 2, 2, 2, 2, 2, 3 ),
 ( 0.2628205128205128305, 0.2641025641025641080, 0.2666666666666666630, 0.2692307692307692180, 0.2717948717948717730, 0.2743589743589743835, 0.2756410256410256610 ),
 .UNSPECIFIED. ) 
 CURVE ( )  GEOMETRIC_REPRESENTATION_ITEM ( )  RATIONAL_B_SPLINE_CURVE ( ( 0.9755282581475768211, 0.9755282581475768211, 1.000000000000000000, 0.9510565162951535312, 1.000000000000000000, 0.9510565162951535312, 1.000000000000000000, 0.9510565162951535312, 1.000000000000000000, 0.9510565162951535312, 1.000000000000000000, 0.9755282581475768211, 0.9755282581475768211 ) ) 
 REPRESENTATION_ITEM ( '' )  );
#552 = CARTESIAN_POINT ( 'NONE',  ( -2.162160676586882350E-15, 36.62500000273119127, -35.31076352940722529 ) ) ;
#553 = CARTESIAN_POINT ( 'NONE',  ( 0.04044903255044120238, 47.08555583240935505, 27.95245687107223276 ) ) ;
#554 = CARTESIAN_POINT ( 'NONE',  ( 1.507698388325705758E-15, 15.12499999726880873, -24.62258325217400312 ) ) ;
#555 = FACE_OUTER_BOUND ( 'NONE', #3316, .T. ) ;
#556 = ORIENTED_EDGE ( 'NONE', *, *, #8453, .F. ) ;
#557 = CARTESIAN_POINT ( 'NONE',  ( 10.37757302488624056, 44.77500000273119696, -31.93888565452638417 ) ) ;
#558 = CARTESIAN_POINT ( 'NONE',  ( -5.147494310547531704, 50.94874572391553613, 32.49999999999996447 ) ) ;
#559 = CARTESIAN_POINT ( 'NONE',  ( -24.22776226481240514, 50.53423583425731636, 13.94119854578937812 ) ) ;
#560 = CARTESIAN_POINT ( 'NONE',  ( -27.16883889988623935, 69.57500000273120122, 19.73931689729374739 ) ) ;
#561 = ORIENTED_EDGE ( 'NONE', *, *, #13358, .F. ) ;
#562 = CARTESIAN_POINT ( 'NONE',  ( 27.16883889988623935, 16.32500000273116925, -19.73931689729374384 ) ) ;
#563 = CARTESIAN_POINT ( 'NONE',  ( -20.50609665440969209, 24.89062500000000000, 20.50609665441005092 ) ) ;
#564 = VERTEX_POINT ( 'NONE', #663 ) ;
#565 = DIRECTION ( 'NONE',  ( -0.000000000000000000, -1.000000000000000000, -0.000000000000000000 ) ) ;
#566 = CARTESIAN_POINT ( 'NONE',  ( 33.58253175000000113, 56.22500000273117138, -10.91162601494193751 ) ) ;
#567 = CARTESIAN_POINT ( 'NONE',  ( -7.505752307973343918, 50.09895833333332860, -28.01184896238290989 ) ) ;
#568 = CARTESIAN_POINT ( 'NONE',  ( 32.50000000000000711, 17.40000000546238823, 10.55989012756945122 ) ) ;
#569 = CARTESIAN_POINT ( 'NONE',  ( 0.000000000000000000, 80.00000000000001421, -32.50000000000000000 ) ) ;
#570 = CARTESIAN_POINT ( 'NONE',  ( -23.41746825000000243, 6.224999997268827912, 7.608796670333725309 ) ) ;
#571 = CARTESIAN_POINT ( 'NONE',  ( 20.75514604977249178, 30.07500000273118701, 28.56700777964553950 ) ) ;
#572 = CARTESIAN_POINT ( 'NONE',  ( 3.980102097228898626E-15, 80.00000000000001421, 32.50000000000000000 ) ) ;
#573 = CARTESIAN_POINT ( 'NONE',  ( -7.543491769121917656, 58.97357666574269786, -28.00173670424536354 ) ) ;
#574 = CARTESIAN_POINT ( 'NONE',  ( 13.91746824999999887, 77.87500000273116996, -1.704398294459741270E-15 ) ) ;
#575 = CARTESIAN_POINT ( 'NONE',  ( 5.779280353836490358E-15, 8.500000000000000000, 32.49999999999999289 ) ) ;
#576 = CARTESIAN_POINT ( 'NONE',  ( 32.50000000000000000, 7.099999999999993427, -10.55989012756945833 ) ) ;
#577 = CARTESIAN_POINT ( 'NONE',  ( -19.09188309203694445, 63.56249999999999289, -19.09188309203661049 ) ) ;
#578 = CARTESIAN_POINT ( 'NONE',  ( 24.50000000000000355, 17.84999999453763309, -7.960532557706203605 ) ) ;
#579 = CARTESIAN_POINT ( 'NONE',  ( -8.960552108402742093E-16, 76.37500000273116996, -14.63369212191046387 ) ) ;
#580 = CARTESIAN_POINT ( 'NONE',  ( -24.20753774853756823, 29.04427083333332504, -13.97622843553588723 ) ) ;
#581 = CARTESIAN_POINT ( 'NONE',  ( 27.16883889988624290, 23.92500000273117777, 19.73931689729373673 ) ) ;
#582 = CARTESIAN_POINT ( 'NONE',  ( 33.58253175000000823, 76.02500000273118985, 10.91162601494192863 ) ) ;
#583 = CARTESIAN_POINT ( 'NONE',  ( 10.37757302488624056, 30.77500000273118630, -31.93888565452638417 ) ) ;
#584 = CARTESIAN_POINT ( 'NONE',  ( -27.16883889988624290, 17.17500000273119909, -19.73931689729374028 ) ) ;
#585 = CARTESIAN_POINT ( 'NONE',  ( 27.95245687107223986, 59.41444416759064495, 0.04044903254993640479 ) ) ;
#586 = CARTESIAN_POINT ( 'NONE',  ( 10.37757302488624767, 67.72500000273117848, 31.93888565452638417 ) ) ;
#587 = LINE ( 'NONE', #26690, #24962 ) ;
#588 = CARTESIAN_POINT ( 'NONE',  ( 32.50000000000000711, 52.89999999999999147, 10.55989012756945122 ) ) ;
#589 = VECTOR ( 'NONE', #16460, 1000.000000000000000 ) ;
#590 = CARTESIAN_POINT ( 'NONE',  ( -33.58253175000000113, 55.22500000273117848, 10.91162601494193929 ) ) ;
#591 = CARTESIAN_POINT ( 'NONE',  ( -18.94512977948575738, 11.92499999726881477, -13.76444248337723231 ) ) ;
#592 = ORIENTED_EDGE ( 'NONE', *, *, #5855, .F. ) ;
#593 = CARTESIAN_POINT ( 'NONE',  ( 6.486482029760649416E-15, 69.87500000273121259, 35.31076352940723240 ) ) ;
#594 = FACE_OUTER_BOUND ( 'NONE', #26488, .T. ) ;
#595 = CARTESIAN_POINT ( 'NONE',  ( 1.507698388325705758E-15, 9.124999997268822938, -24.62258325217400312 ) ) ;
#596 = CARTESIAN_POINT ( 'NONE',  ( 26.06988505166735592, 25.18267333425730214, 7.025853678916393896 ) ) ;
#597 = ORIENTED_EDGE ( 'NONE', *, *, #28712, .F. ) ;
#598 = CARTESIAN_POINT ( 'NONE',  ( -10.37757302488623701, 39.52500000273119696, 31.93888565452638417 ) ) ;
#599 = CARTESIAN_POINT ( 'NONE',  ( -10.04305231718578462, 68.90000000546237402, 30.90933677959249337 ) ) ;
#600 = AXIS2_PLACEMENT_3D ( 'NONE', #12178, #2052, #12527 ) ;
#601 = VERTEX_POINT ( 'NONE', #830 ) ;
#602 = CARTESIAN_POINT ( 'NONE',  ( -30.02300923189239512, 56.25781249999997868, 2.654126918244515359E-13 ) ) ;
#603 = CARTESIAN_POINT ( 'NONE',  ( 20.08610463437158344, 11.20000000546238184, 27.64615127144129403 ) ) ;
#604 = CARTESIAN_POINT ( 'NONE',  ( -19.82091636218621034, 2.799999999999997158, -14.40073868116559552 ) ) ;
#605 = CARTESIAN_POINT ( 'NONE',  ( -10.37757302488624411, 76.72500000273119269, -31.93888565452638417 ) ) ;
#606 = CARTESIAN_POINT ( 'NONE',  ( 20.50609665441005092, 24.03124999999999645, 20.50609665440969209 ) ) ;
#607 = CARTESIAN_POINT ( 'NONE',  ( -7.570916362186215665, 7.399999999999989697, 23.30088464923126423 ) ) ;
#608 = CARTESIAN_POINT ( 'NONE',  ( -20.75514604977248823, 11.07500000273117813, -28.56700777964554305 ) ) ;
#609 = EDGE_CURVE ( 'NONE', #1393, #3518, #27447, .T. ) ;
#610 = CARTESIAN_POINT ( 'NONE',  ( 10.37757302488624056, 24.52500000273119696, -31.93888565452638417 ) ) ;
#611 = CARTESIAN_POINT ( 'NONE',  ( -8.601468415847515203, 77.17500000273120975, 11.83890561707634959 ) ) ;
#612 = CARTESIAN_POINT ( 'NONE',  ( -1.089172066684569321E-14, 76.75000000546238255, 15.00000000000000000 ) ) ;
#613 = AXIS2_PLACEMENT_3D ( 'NONE', #20476, #12571, #28521 ) ;
#614 = CARTESIAN_POINT ( 'NONE',  ( -28.02196122052058413, 30.90065999907601579, -7.468012846824272799 ) ) ;
#615 = AXIS2_PLACEMENT_3D ( 'NONE', #16459, #8052, #21610 ) ;
#616 = CARTESIAN_POINT ( 'NONE',  ( -8.601468415847518756, 77.07500000273117280, -11.83890561707634781 ) ) ;
#617 = CARTESIAN_POINT ( 'NONE',  ( -15.01150461594595775, 45.37239583333332860, 26.00068869287368756 ) ) ;
#618 = EDGE_CURVE ( 'NONE', #4913, #19128, #19343, .T. ) ;
#619 = CARTESIAN_POINT ( 'NONE',  ( -19.82091636218621389, 11.19999999999998863, 14.40073868116558842 ) ) ;
#620 = CARTESIAN_POINT ( 'NONE',  ( -10.04305231718578462, 54.90000000546239534, 30.90933677959249337 ) ) ;
#621 = CARTESIAN_POINT ( 'NONE',  ( -14.01125832528328985, 62.26784749907602645, -24.18731323226223040 ) ) ;
#622 = CARTESIAN_POINT ( 'NONE',  ( -2.162160676586881955E-15, 42.62500000273119838, -35.31076352940723240 ) ) ;
#623 = CARTESIAN_POINT ( 'NONE',  ( -8.601468415847518756, 78.57500000273120122, -11.83890561707634781 ) ) ;
#624 = CARTESIAN_POINT ( 'NONE',  ( -20.75514604977248112, 53.67500000273119554, 28.56700777964554661 ) ) ;
#625 = CARTESIAN_POINT ( 'NONE',  ( 33.58253175000000823, 34.27500000273116854, 10.91162601494192685 ) ) ;
#626 = CARTESIAN_POINT ( 'NONE',  ( -1.778240108872766143E-15, 16.00000000546237899, -32.49999999999999289 ) ) ;
#627 = CARTESIAN_POINT ( 'NONE',  ( 24.20753774853731244, 23.31510416666666430, -13.97622843553633132 ) ) ;
#628 = DIRECTION ( 'NONE',  ( -1.224646799147353454E-16, 1.000000000000000000, -0.000000000000000000 ) ) ;
#629 = CARTESIAN_POINT ( 'NONE',  ( -7.579748464070167083E-14, 12.24999999453762456, -24.50000000000000000 ) ) ;
#630 = CARTESIAN_POINT ( 'NONE',  ( 20.08610463437157279, 75.30000000000001137, -27.64615127144129758 ) ) ;
#631 = CARTESIAN_POINT ( 'NONE',  ( -20.75514604977248112, 9.425000002731184878, 28.56700777964554661 ) ) ;
#632 = CARTESIAN_POINT ( 'NONE',  ( 23.41746824999999887, 2.624999997268812280, 0.000000000000000000 ) ) ;
#633 = B_SPLINE_CURVE_WITH_KNOTS ( 'NONE', 3,
 ( #5996, #16472, #16149, #29654, #14063, #13570, #10819, #16643, #26602, #24033, #24364, #502, #10987, #21459, #995, #834, #21793, #24526, #31739, #11480, #2925, #19384, #5497, #26926, #5834, #29160, #15976, #26433, #13395, #5667, #31902, #8397, #29333, #26769, #3260, #4261, #16811, #4092, #27601, #14735, #27267, #32571, #20059, #6666 ),
 .UNSPECIFIED., .F., .F.,
 ( 4, 2, 2, 2, 2, 2, 2, 2, 2, 2, 2, 2, 2, 2, 2, 2, 2, 2, 2, 2, 2, 4 ),
 ( 0.000000000000000000, 0.004064997385822698324, 0.008129994771645396648, 0.01219499215746809584, 0.01422749085037944457, 0.01625998954329079330, 0.02032498692911348381, 0.02235748562202483428, 0.02438998431493618127, 0.02845498170075888567, 0.03251997908658158659, 0.03455247777949293359, 0.03658497647240428752, 0.04064997385822698150, 0.04471497124404968243, 0.04877996862987238336, 0.05081246732278373035, 0.05284496601569507734, 0.05690996340151777827, 0.05894246209442912526, 0.06097496078734047226, 0.06503995817316317318 ),
 .UNSPECIFIED. ) ;
#634 = CARTESIAN_POINT ( 'NONE',  ( 7.025853678916867295, 29.75482666574269075, 26.06988505166722803 ) ) ;
#635 = CARTESIAN_POINT ( 'NONE',  ( -32.50000000000000000, 66.10000000000000853, 10.55989012756946366 ) ) ;
#636 = CARTESIAN_POINT ( 'NONE',  ( -27.16883889988623935, 21.32500000273118701, 19.73931689729374739 ) ) ;
#637 = MECHANICAL_DESIGN_GEOMETRIC_PRESENTATION_REPRESENTATION (  '', ( #24223 ), #24742 ) ;
#638 = CARTESIAN_POINT ( 'NONE',  ( -26.07999730980490583, 52.96354166666666430, -6.988114217767815717 ) ) ;
#639 = ORIENTED_EDGE ( 'NONE', *, *, #18179, .T. ) ;
#640 = CARTESIAN_POINT ( 'NONE',  ( -10.37757302488624411, 56.72500000273118559, -31.93888565452638417 ) ) ;
#641 =( BOUNDED_CURVE ( )  B_SPLINE_CURVE ( 2, ( #9073, #30506, #22800, #33255, #4263, #16979, #33077, #4432, #7006, #20237, #14568, #27436, #17488 ),
 .UNSPECIFIED., .F., .F. ) 
 B_SPLINE_CURVE_WITH_KNOTS ( ( 3, 2, 2, 2, 2, 2, 3 ),
 ( 0.1602564102564102699, 0.1615384615384615474, 0.1641025641025641024, 0.1666666666666666574, 0.1692307692307692402, 0.1717948717948717952, 0.1730769230769230727 ),
 .UNSPECIFIED. ) 
 CURVE ( )  GEOMETRIC_REPRESENTATION_ITEM ( )  RATIONAL_B_SPLINE_CURVE ( ( 0.9755282581475768211, 0.9755282581475770431, 1.000000000000000000, 0.9510565162951535312, 1.000000000000000000, 0.9510565162951535312, 1.000000000000000000, 0.9510565162951535312, 1.000000000000000000, 0.9510565162951535312, 1.000000000000000000, 0.9755282581475768211, 0.9755282581475768211 ) ) 
 REPRESENTATION_ITEM ( '' )  );
#642 = ORIENTED_EDGE ( 'NONE', *, *, #21531, .T. ) ;
#643 = CARTESIAN_POINT ( 'NONE',  ( 26.00068869287340334, 19.87760416666666430, -15.01150461594642316 ) ) ;
#644 = CARTESIAN_POINT ( 'NONE',  ( -20.53372385742071771, 19.45350666759063785, 20.47846945139902530 ) ) ;
#645 = CARTESIAN_POINT ( 'NONE',  ( 20.08610463437158344, 38.69999999999999574, 27.64615127144129403 ) ) ;
#646 = ORIENTED_EDGE ( 'NONE', *, *, #15565, .T. ) ;
#647 = CARTESIAN_POINT ( 'NONE',  ( 1.836970198721029589E-15, 74.00000000000001421, -15.00000000000000000 ) ) ;
#648 = CARTESIAN_POINT ( 'NONE',  ( -20.75514604977248823, 27.07500000273119412, -28.56700777964554305 ) ) ;
#649 = CARTESIAN_POINT ( 'NONE',  ( 32.50000000000000711, 31.40000000546238823, 10.55989012756945122 ) ) ;
#650 = ADVANCED_FACE ( 'NONE', ( #26598 ), #1853, .T. ) ;
#651 = CARTESIAN_POINT ( 'NONE',  ( -12.13525491562420910, 72.19999999999998863, 8.816778784387098611 ) ) ;
#652 = CARTESIAN_POINT ( 'NONE',  ( -5.147494310547423346, 54.94874572391552903, 32.50000000000000000 ) ) ;
#653 = CARTESIAN_POINT ( 'NONE',  ( 4.635254915624212657, 72.59999999999999432, 14.26584774442730286 ) ) ;
#654 = CARTESIAN_POINT ( 'NONE',  ( 33.58253175000000823, 44.27500000273120406, 10.91162601494192863 ) ) ;
#655 = EDGE_CURVE ( 'NONE', #33572, #1522, #5309, .T. ) ;
#656 = CARTESIAN_POINT ( 'NONE',  ( 32.50000000000000711, 24.90000000000000213, 10.55989012756945122 ) ) ;
#657 = CARTESIAN_POINT ( 'NONE',  ( 32.50000000000000711, 18.90000000000001634, 10.55989012756945122 ) ) ;
#658 = CARTESIAN_POINT ( 'NONE',  ( 7.570916362186213000, 10.39999999999999325, -23.30088464923126423 ) ) ;
#659 = CARTESIAN_POINT ( 'NONE',  ( 20.75514604977248467, 62.42500000273118133, -28.56700777964554305 ) ) ;
#660 = CARTESIAN_POINT ( 'NONE',  ( -15.14183272437241889, 8.449999994537634507, -20.84094480462497856 ) ) ;
#661 = CARTESIAN_POINT ( 'NONE',  ( 20.75514604977248467, 54.67500000273119554, -28.56700777964554305 ) ) ;
#662 = CARTESIAN_POINT ( 'NONE',  ( 23.41746824999999887, 10.62499999726881938, 0.000000000000000000 ) ) ;
#663 = CARTESIAN_POINT ( 'NONE',  ( -8.891200544363830713E-16, 75.75000000546236834, -15.00000000000000000 ) ) ;
#664 = CARTESIAN_POINT ( 'NONE',  ( -27.16883889988624290, 6.925000002731191096, -19.73931689729374028 ) ) ;
#665 = CARTESIAN_POINT ( 'NONE',  ( -14.01125832528285109, 43.37277750092397355, 24.18731323226248264 ) ) ;
#666 = CARTESIAN_POINT ( 'NONE',  ( 23.41705066890375520, 16.99999999999998934, -0.7769985253002599235 ) ) ;
#667 = CARTESIAN_POINT ( 'NONE',  ( -32.50000000000000000, 20.10000000000000497, 10.55989012756946366 ) ) ;
#668 = CARTESIAN_POINT ( 'NONE',  ( -10.37757302488623701, 25.52500000273118275, 31.93888565452638417 ) ) ;
#669 = CARTESIAN_POINT ( 'NONE',  ( 32.50000000000000711, 56.90000000000000568, 10.55989012756945122 ) ) ;
#670 = CARTESIAN_POINT ( 'NONE',  ( 32.50000000000000711, 61.40000000546236691, 10.55989012756945122 ) ) ;
#671 = CARTESIAN_POINT ( 'NONE',  ( 20.08610463437157279, 1.800000005462388364, -27.64615127144129758 ) ) ;
#672 = CARTESIAN_POINT ( 'NONE',  ( -26.02091320914878025, 58.54388916574269075, -14.97647472619899389 ) ) ;
#673 = CARTESIAN_POINT ( 'NONE',  ( 6.277390505771533514E-15, 49.00000000546238965, 34.17252228774368916 ) ) ;
#674 = CARTESIAN_POINT ( 'NONE',  ( 5.147494310547434893, 48.55125428154685352, 32.49999999999999289 ) ) ;
#675 = CARTESIAN_POINT ( 'NONE',  ( 0.000000000000000000, 80.00000000000001421, -32.50000000000000000 ) ) ;
#676 = AXIS2_PLACEMENT_3D ( 'NONE', #19715, #30162, #1674 ) ;
#677 = CIRCLE ( 'NONE', #3964, 30.50000000000000000 ) ;
#678 = CARTESIAN_POINT ( 'NONE',  ( 6.988114217768294445, 24.31770833333332504, 26.07999730980477437 ) ) ;
#679 = VERTEX_POINT ( 'NONE', #27771 ) ;
#680 = VECTOR ( 'NONE', #25652, 1000.000000000000000 ) ;
#681 = CARTESIAN_POINT ( 'NONE',  ( 27.16883889988623935, 74.32500000273118701, -19.73931689729374384 ) ) ;
#682 = CARTESIAN_POINT ( 'NONE',  ( -15.01150461594642138, 32.76822916666666430, -26.00068869287340334 ) ) ;
#683 = CARTESIAN_POINT ( 'NONE',  ( 18.94512977948575738, 12.92499999726881654, 13.76444248337723408 ) ) ;
#684 = VERTEX_POINT ( 'NONE', #9066 ) ;
#685 = CARTESIAN_POINT ( 'NONE',  ( 30.02300923189239867, 42.22694416759065206, 0.04044903254992252006 ) ) ;
#686 = CARTESIAN_POINT ( 'NONE',  ( -26.29305231718579350, 16.30000000546237615, -19.10302069950537884 ) ) ;
#687 = CARTESIAN_POINT ( 'NONE',  ( 20.50609665441005092, 51.53124999999999289, 20.50609665440969209 ) ) ;
#688 = CARTESIAN_POINT ( 'NONE',  ( 2.740863092043355209E-13, 65.71093749999997158, 30.02300923189239512 ) ) ;
#689 = CARTESIAN_POINT ( 'NONE',  ( -10.37757302488624411, 48.97500000273119269, -31.93888565452638417 ) ) ;
#690 = CARTESIAN_POINT ( 'NONE',  ( 32.50000000000000711, 53.40000000546238823, 10.55989012756945122 ) ) ;
#691 = CARTESIAN_POINT ( 'NONE',  ( -11.25946833292375793, 79.57500000273121543, 8.180482586598737171 ) ) ;
#692 = CARTESIAN_POINT ( 'NONE',  ( -10.37757302488623701, 37.52500000273117564, 31.93888565452638417 ) ) ;
#693 = CARTESIAN_POINT ( 'NONE',  ( 0.000000000000000000, -10.99999999999999645, 30.00000000000000000 ) ) ;
#694 = CARTESIAN_POINT ( 'NONE',  ( -20.75514604977248112, 63.67500000273116711, 28.56700777964554661 ) ) ;
#695 = CARTESIAN_POINT ( 'NONE',  ( -1.053607264507113999E-13, 63.00000000546238255, 32.50000000000000711 ) ) ;
#696 = CARTESIAN_POINT ( 'NONE',  ( -32.50000000000000000, 39.89999999999999858, -10.55989012756945478 ) ) ;
#697 = CARTESIAN_POINT ( 'NONE',  ( 7.236395654485755280, 12.22499999726881015, 22.27133577429736988 ) ) ;
#698 = CARTESIAN_POINT ( 'NONE',  ( -33.58253175000000113, 5.275000002731187188, -10.91162601494193218 ) ) ;
#699 = VECTOR ( 'NONE', #19060, 1000.000000000000000 ) ;
#700 = CARTESIAN_POINT ( 'NONE',  ( 26.29305231718579350, 12.79999999999997762, 19.10302069950537529 ) ) ;
#701 = CARTESIAN_POINT ( 'NONE',  ( -4.300734207923755825, 73.77500000273118985, 13.23629886949340673 ) ) ;
#702 = CARTESIAN_POINT ( 'NONE',  ( -2.162160676586882350E-15, 72.87500000273115575, -35.31076352940722529 ) ) ;
#703 = CARTESIAN_POINT ( 'NONE',  ( 7.570916362186213000, 4.149999994537633796, -23.30088464923126423 ) ) ;
#704 = CARTESIAN_POINT ( 'NONE',  ( 33.58253175000000113, 70.37500000273121259, -4.112674001490185761E-15 ) ) ;
#705 = EDGE_LOOP ( 'NONE', ( #26640, #8768, #26705, #27002 ) ) ;
#706 = CARTESIAN_POINT ( 'NONE',  ( 2.757615341152813402E-15, -45.51763809020504681, 0.000000000000000000 ) ) ;
#707 = CARTESIAN_POINT ( 'NONE',  ( 26.09010956794232428, 14.58371500092397710, -6.950374756619718042 ) ) ;
#708 = DIRECTION ( 'NONE',  ( 0.000000000000000000, -0.000000000000000000, -1.000000000000000000 ) ) ;
#709 = CARTESIAN_POINT ( 'NONE',  ( 27.16883889988624290, 47.92500000273118843, 19.73931689729373673 ) ) ;
#710 = CARTESIAN_POINT ( 'NONE',  ( 33.58253175000000113, 12.37500000273118772, -4.112674001490185761E-15 ) ) ;
#711 = CARTESIAN_POINT ( 'NONE',  ( 10.37757302488624767, 59.97500000273119269, 31.93888565452638417 ) ) ;
#712 = CARTESIAN_POINT ( 'NONE',  ( -13.97622843553632777, 53.39322916666665719, -24.20753774853731599 ) ) ;
#713 = CARTESIAN_POINT ( 'NONE',  ( -15.04653450569291984, 33.06027750092398776, 25.98046417659859486 ) ) ;
#714 = CARTESIAN_POINT ( 'NONE',  ( 28.02196122052058413, 32.61940999907601224, 7.468012846824272799 ) ) ;
#715 = CARTESIAN_POINT ( 'NONE',  ( -10.04305231718578462, 76.90000000546235981, 30.90933677959249337 ) ) ;
#716 = CARTESIAN_POINT ( 'NONE',  ( -13.91746824999999887, 78.87500000273118417, 0.000000000000000000 ) ) ;
#717 = CARTESIAN_POINT ( 'NONE',  ( 27.16883889988624290, 39.92500000273119554, 19.73931689729373673 ) ) ;
#718 = CARTESIAN_POINT ( 'NONE',  ( 24.22776226481265383, 43.07513916574269786, 13.94119854578893580 ) ) ;
#719 = CARTESIAN_POINT ( 'NONE',  ( -18.94512977948576093, 15.82499999726880091, 13.76444248337722698 ) ) ;
#720 = CARTESIAN_POINT ( 'NONE',  ( 4.445600272181915325E-13, 14.00000000546237544, -32.50000000000000000 ) ) ;
#721 = ORIENTED_EDGE ( 'NONE', *, *, #5519, .F. ) ;
#722 = CARTESIAN_POINT ( 'NONE',  ( 27.16883889988624290, 46.17500000273118133, 19.73931689729373673 ) ) ;
#723 = DIRECTION ( 'NONE',  ( -0.000000000000000000, 1.000000000000000000, -0.000000000000000000 ) ) ;
#724 = CARTESIAN_POINT ( 'NONE',  ( 26.09010956794232428, 48.95871500092396644, -6.950374756619718042 ) ) ;
#725 = CARTESIAN_POINT ( 'NONE',  ( 27.16883889988624290, 68.17500000273119554, 19.73931689729373673 ) ) ;
#726 = VERTEX_POINT ( 'NONE', #9227 ) ;
#727 = CARTESIAN_POINT ( 'NONE',  ( 27.16883889988623935, 18.32500000273119767, -19.73931689729374384 ) ) ;
#728 = AXIS2_PLACEMENT_3D ( 'NONE', #8070, #26267, #31742 ) ;
#729 = CARTESIAN_POINT ( 'NONE',  ( 30.02300923189239512, 23.60156250000000000, -2.619432448724977703E-13 ) ) ;
#730 = ORIENTED_EDGE ( 'NONE', *, *, #3699, .F. ) ;
#731 = LINE ( 'NONE', #16213, #1228 ) ;
#732 = CARTESIAN_POINT ( 'NONE',  ( 33.58253175000000113, 54.12500000273118417, -4.112674001490185761E-15 ) ) ;
#733 = CARTESIAN_POINT ( 'NONE',  ( 26.00068869287340334, 57.69010416666667140, -15.01150461594642316 ) ) ;
#734 = CARTESIAN_POINT ( 'NONE',  ( -32.50000000000000000, 20.50000000546237189, 0.000000000000000000 ) ) ;
#735 = CYLINDRICAL_SURFACE ( 'NONE', #19090, 24.50000000000000000 ) ;
#736 = CARTESIAN_POINT ( 'NONE',  ( -18.94512977948576093, 6.324999997268820451, 13.76444248337722698 ) ) ;
#737 = CARTESIAN_POINT ( 'NONE',  ( 33.58253175000000823, 24.27500000273120051, 10.91162601494192863 ) ) ;
#738 = CARTESIAN_POINT ( 'NONE',  ( -13.94119854578892514, 16.43451416574268720, 24.22776226481266448 ) ) ;
#739 = CARTESIAN_POINT ( 'NONE',  ( 23.41746824999999887, 19.12499999726882649, 0.000000000000000000 ) ) ;
#740 =( BOUNDED_CURVE ( )  B_SPLINE_CURVE ( 2, ( #17852, #9600, #28472, #17505, #1696, #12172, #20082, #14927, #28305, #4967, #15102, #7193, #18196 ),
 .UNSPECIFIED., .F., .T. ) 
 B_SPLINE_CURVE_WITH_KNOTS ( ( 3, 2, 2, 2, 2, 2, 3 ),
 ( 0.4294871794871795156, 0.4307692307692307931, 0.4333333333333333481, 0.4358974358974359031, 0.4384615384615384581, 0.4410256410256410131, 0.4423076923076922906 ),
 .UNSPECIFIED. ) 
 CURVE ( )  GEOMETRIC_REPRESENTATION_ITEM ( )  RATIONAL_B_SPLINE_CURVE ( ( 0.9755282581475768211, 0.9755282581475772652, 1.000000000000000000, 0.9510565162951535312, 1.000000000000000000, 0.9510565162951535312, 1.000000000000000000, 0.9510565162951535312, 1.000000000000000000, 0.9510565162951535312, 1.000000000000000000, 0.9755282581475768211, 0.9755282581475768211 ) ) 
 REPRESENTATION_ITEM ( '' )  );
#741 = EDGE_CURVE ( 'NONE', #30741, #33572, #33071, .T. ) ;
#742 = CARTESIAN_POINT ( 'NONE',  ( 6.277390505771533514E-15, 12.49999999999999645, 34.17252228774368916 ) ) ;
#743 = ORIENTED_EDGE ( 'NONE', *, *, #12358, .F. ) ;
#744 = CARTESIAN_POINT ( 'NONE',  ( -19.82091636218621389, 18.94999999453764161, 14.40073868116558842 ) ) ;
#745 = CARTESIAN_POINT ( 'NONE',  ( -8.601468415847515203, 77.17500000273120975, 11.83890561707634959 ) ) ;
#746 = CARTESIAN_POINT ( 'NONE',  ( 13.97622843553589966, 40.21614583333332860, -24.20753774853756113 ) ) ;
#747 = CARTESIAN_POINT ( 'NONE',  ( 20.75514604977249178, 25.82500000273117280, 28.56700777964553950 ) ) ;
#748 = CARTESIAN_POINT ( 'NONE',  ( 20.75514604977248467, 64.42500000273116711, -28.56700777964554305 ) ) ;
#749 = CARTESIAN_POINT ( 'NONE',  ( -20.75514604977248823, 27.07500000273119412, -28.56700777964554305 ) ) ;
#750 = AXIS2_PLACEMENT_3D ( 'NONE', #9964, #23009, #11849 ) ;
#751 = CARTESIAN_POINT ( 'NONE',  ( 33.58253175000000113, 18.47500000273117848, -10.91162601494193751 ) ) ;
#752 = CARTESIAN_POINT ( 'NONE',  ( -27.16883889988624290, 11.17500000273119554, -19.73931689729374028 ) ) ;
#753 = CARTESIAN_POINT ( 'NONE',  ( 7.025853678916403666, 55.26079833425730214, -26.06988505166735237 ) ) ;
#754 = AXIS2_PLACEMENT_3D ( 'NONE', #32475, #1069, #27509 ) ;
#755 = EDGE_CURVE ( 'NONE', #26901, #13370, #4599, .T. ) ;
#756 = CARTESIAN_POINT ( 'NONE',  ( -33.58253175000000113, 71.22500000273117848, 10.91162601494193929 ) ) ;
#757 = EDGE_CURVE ( 'NONE', #12435, #15614, #30959, .T. ) ;
#758 = CARTESIAN_POINT ( 'NONE',  ( -15.01150461594642138, 53.39322916666665009, -26.00068869287340334 ) ) ;
#759 = DIRECTION ( 'NONE',  ( -0.000000000000000000, 1.000000000000000000, -0.000000000000000000 ) ) ;
#760 = CARTESIAN_POINT ( 'NONE',  ( -8.960552108402744065E-16, 76.87500000273115575, -14.63369212191046209 ) ) ;
#761 = CARTESIAN_POINT ( 'NONE',  ( -26.29305231718579350, 53.79999999999999716, -19.10302069950537884 ) ) ;
#762 = CARTESIAN_POINT ( 'NONE',  ( 2.445080149700053643E-15, 72.75000000546238255, 15.00000000000000000 ) ) ;
#763 = CARTESIAN_POINT ( 'NONE',  ( -27.16883889988623935, 55.32500000273118701, 19.73931689729374739 ) ) ;
#764 = CARTESIAN_POINT ( 'NONE',  ( 14.47279130897151767, 15.42499999726879878, -19.92008829642072598 ) ) ;
#765 = EDGE_CURVE ( 'NONE', #2905, #6717, #4427, .T. ) ;
#766 = ORIENTED_EDGE ( 'NONE', *, *, #17973, .F. ) ;
#767 = CARTESIAN_POINT ( 'NONE',  ( -27.16883889988623935, 69.57500000273118701, 19.73931689729374739 ) ) ;
#768 = CARTESIAN_POINT ( 'NONE',  ( -33.58253175000000113, 3.225000002731193138, 10.91162601494193929 ) ) ;
#769 = CARTESIAN_POINT ( 'NONE',  ( -23.41746824999999887, 7.624999997268816720, -2.867812753649727150E-15 ) ) ;
#770 = CARTESIAN_POINT ( 'NONE',  ( -6.950374756619716266, 24.03684000092397000, -26.09010956794232428 ) ) ;
#771 = VERTEX_POINT ( 'NONE', #7000 ) ;
#772 = CARTESIAN_POINT ( 'NONE',  ( 33.58253175000000113, 38.12500000273118417, -4.112674001490185761E-15 ) ) ;
#773 = CARTESIAN_POINT ( 'NONE',  ( -5.147494310547450880, 68.94874572391553613, 32.49999999999999289 ) ) ;
#774 = VERTEX_POINT ( 'NONE', #17482 ) ;
#775 = CARTESIAN_POINT ( 'NONE',  ( -28.01184896238290278, 52.67708333333333570, 7.505752307973363457 ) ) ;
#776 = CARTESIAN_POINT ( 'NONE',  ( 27.16883889988623935, 66.57500000273118701, -19.73931689729374384 ) ) ;
#777 = CARTESIAN_POINT ( 'NONE',  ( 15.00000000000000000, 75.35000000546236265, -4.873795443493596835 ) ) ;
#778 = CARTESIAN_POINT ( 'NONE',  ( 6.486482029760649416E-15, 71.62500000273119838, 35.31076352940723240 ) ) ;
#779 = CARTESIAN_POINT ( 'NONE',  ( -26.00068869287368756, 25.60677083333332149, -15.01150461594595775 ) ) ;
#780 = CARTESIAN_POINT ( 'NONE',  ( 15.14183272437241889, 5.699999999999993960, 20.84094480462498211 ) ) ;
#781 = CARTESIAN_POINT ( 'NONE',  ( 10.37757302488624767, 7.975000002731186477, 31.93888565452638417 ) ) ;
#782 = CARTESIAN_POINT ( 'NONE',  ( -2.162160676586881955E-15, 18.62500000273117351, -35.31076352940723240 ) ) ;
#783 = CARTESIAN_POINT ( 'NONE',  ( -11.25946833292375793, 76.67500000273119554, -8.180482586598733619 ) ) ;
#784 = CARTESIAN_POINT ( 'NONE',  ( -8.891200544363830713E-16, 77.75000000546235412, -15.00000000000000000 ) ) ;
#785 = CARTESIAN_POINT ( 'NONE',  ( -7.468012846824272799, 40.35378499907601935, 28.02196122052058413 ) ) ;
#786 = CARTESIAN_POINT ( 'NONE',  ( -9.270509831248425314, 81.70000000000001705, -12.75976212528059861 ) ) ;
#787 = CARTESIAN_POINT ( 'NONE',  ( -28.01184896238290278, 49.23958333333332860, 7.505752307973363457 ) ) ;
#788 = CARTESIAN_POINT ( 'NONE',  ( 26.29305231718578995, 53.70000000546236407, -19.10302069950538240 ) ) ;
#789 = CARTESIAN_POINT ( 'NONE',  ( -10.04305231718579172, 54.10000000546237686, -30.90933677959248982 ) ) ;
#790 = CARTESIAN_POINT ( 'NONE',  ( 0.04044903255044120238, 60.83555583240935505, 27.95245687107223276 ) ) ;
#791 = CARTESIAN_POINT ( 'NONE',  ( -33.58253175000000113, 43.12500000273116996, 0.000000000000000000 ) ) ;
#792 = CARTESIAN_POINT ( 'NONE',  ( 8.601468415847516980, 80.17500000273113869, -11.83890561707634781 ) ) ;
#793 = CARTESIAN_POINT ( 'NONE',  ( 27.16883889988624290, 50.17500000273118843, 19.73931689729373673 ) ) ;
#794 = CARTESIAN_POINT ( 'NONE',  ( 10.37757302488624767, 35.97500000273118559, 31.93888565452638417 ) ) ;
#795 = CARTESIAN_POINT ( 'NONE',  ( -3.331698596277962388, 16.99999999999997868, 23.93330680440991998 ) ) ;
#796 = CARTESIAN_POINT ( 'NONE',  ( 13.97622843553589966, 19.59114583333332504, -24.20753774853756113 ) ) ;
#797 = CARTESIAN_POINT ( 'NONE',  ( -15.00000000000000000, 80.15000000546237402, -4.873795443493594171 ) ) ;
#798 = AXIS2_PLACEMENT_3D ( 'NONE', #23124, #10089, #20568 ) ;
#799 = CARTESIAN_POINT ( 'NONE',  ( 32.50000000000000000, 31.00000000000000000, -3.980102097228898626E-15 ) ) ;
#800 = CARTESIAN_POINT ( 'NONE',  ( -20.08610463437156923, 74.30000000000001137, 27.64615127144130113 ) ) ;
#801 = CARTESIAN_POINT ( 'NONE',  ( -33.58253175000000113, 11.22500000273118559, 10.91162601494193929 ) ) ;
#802 = CARTESIAN_POINT ( 'NONE',  ( 14.47279130897151767, 2.324999997268806240, 19.92008829642072953 ) ) ;
#803 = CARTESIAN_POINT ( 'NONE',  ( -26.29305231718578995, 52.70000000546237828, 19.10302069950538595 ) ) ;
#804 = CARTESIAN_POINT ( 'NONE',  ( 19.06425588902558133, 28.60899333240935150, -19.11951029504797006 ) ) ;
#805 = EDGE_CURVE ( 'NONE', #16083, #1686, #6827, .T. ) ;
#806 = DIRECTION ( 'NONE',  ( 1.000000000000000000, 0.000000000000000000, 0.000000000000000000 ) ) ;
#807 = CARTESIAN_POINT ( 'NONE',  ( 33.58253175000000113, 18.12500000273117706, -4.112674001490185761E-15 ) ) ;
#808 = CARTESIAN_POINT ( 'NONE',  ( 14.47279130897151767, 3.424999997268800112, -19.92008829642072598 ) ) ;
#809 = CARTESIAN_POINT ( 'NONE',  ( 6.988114217767829928, 50.38541666666666430, -26.07999730980489872 ) ) ;
#810 = EDGE_LOOP ( 'NONE', ( #13911, #21012, #6429, #7622 ) ) ;
#811 = CARTESIAN_POINT ( 'NONE',  ( -27.16883889988624290, 58.92500000273119554, -19.73931689729374028 ) ) ;
#812 = EDGE_LOOP ( 'NONE', ( #32829, #8494, #29549, #33668 ) ) ;
#813 = CARTESIAN_POINT ( 'NONE',  ( 26.00068869287340334, 26.75260416666666430, -15.01150461594642316 ) ) ;
#814 = CARTESIAN_POINT ( 'NONE',  ( -15.04653450569291984, 22.74777750092397355, 25.98046417659859486 ) ) ;
#815 = CARTESIAN_POINT ( 'NONE',  ( -1.778240108872766143E-15, 9.499999999999992895, -32.49999999999999289 ) ) ;
#816 = CARTESIAN_POINT ( 'NONE',  ( -14.47279130897151589, 7.324999997268822227, -19.92008829642072598 ) ) ;
#817 = CARTESIAN_POINT ( 'NONE',  ( -20.75514604977248823, 29.07500000273119056, -28.56700777964554305 ) ) ;
#818 = COLOUR_RGB ( '', 0.40784314, 0.44705882, 0.49803922) ;
#819 = CARTESIAN_POINT ( 'NONE',  ( -20.08610463437156923, 32.80000000546237260, 27.64615127144130113 ) ) ;
#820 = CARTESIAN_POINT ( 'NONE',  ( -20.08610463437156923, 76.30000000000001137, 27.64615127144130113 ) ) ;
#821 = CARTESIAN_POINT ( 'NONE',  ( 26.29305231718579350, 33.30000000546237970, 19.10302069950537529 ) ) ;
#822 = CARTESIAN_POINT ( 'NONE',  ( 15.00000000000000355, 72.89999999999999147, 4.873795443493592394 ) ) ;
#823 = CARTESIAN_POINT ( 'NONE',  ( 10.37757302488624767, 41.97500000273118559, 31.93888565452638417 ) ) ;
#824 = CARTESIAN_POINT ( 'NONE',  ( 10.04305231718578817, 25.39999999999999147, -30.90933677959249337 ) ) ;
#825 = CARTESIAN_POINT ( 'NONE',  ( 32.50000000000000000, 22.99999999999999289, -3.980102097228898626E-15 ) ) ;
#826 = CARTESIAN_POINT ( 'NONE',  ( -24.50000000000000000, 9.000000000000007105, -3.000384657911015469E-15 ) ) ;
#827 = CARTESIAN_POINT ( 'NONE',  ( -10.37757302488624411, 62.72500000273117848, -31.93888565452638417 ) ) ;
#828 = CARTESIAN_POINT ( 'NONE',  ( 6.486482029760648627E-15, 53.87500000273119127, 35.31076352940722529 ) ) ;
#829 = CARTESIAN_POINT ( 'NONE',  ( 14.47279130897151767, 12.32499999726880802, 19.92008829642072953 ) ) ;
#830 = CARTESIAN_POINT ( 'NONE',  ( 2.067204126564591252E-14, 2.500000000000004885, -24.50000000000000000 ) ) ;
#831 = CARTESIAN_POINT ( 'NONE',  ( -2.162160676586881955E-15, 6.625000002731173510, -35.31076352940723240 ) ) ;
#832 = CARTESIAN_POINT ( 'NONE',  ( -27.95245687107223986, 37.07069416759063785, -0.04044903254993292840 ) ) ;
#833 = DIRECTION ( 'NONE',  ( 0.000000000000000000, 1.000000000000000000, 0.000000000000000000 ) ) ;
#834 = CARTESIAN_POINT ( 'NONE',  ( -9.638965394428050004, 52.00000000000000000, 31.78062433674932308 ) ) ;
#835 = CARTESIAN_POINT ( 'NONE',  ( -27.16883889988624290, 26.92500000273119554, -19.73931689729374028 ) ) ;
#836 = CARTESIAN_POINT ( 'NONE',  ( -20.08610463437156923, 56.80000000546240102, 27.64615127144130113 ) ) ;
#837 = CARTESIAN_POINT ( 'NONE',  ( -20.08610463437156923, 58.80000000546239391, 27.64615127144130113 ) ) ;
#838 = CARTESIAN_POINT ( 'NONE',  ( 3.880418787951134707, 13.55125428154684997, 24.50000000000000000 ) ) ;
#839 = CARTESIAN_POINT ( 'NONE',  ( -7.468012846824272799, 54.10378499907602645, 28.02196122052058413 ) ) ;
#840 = CARTESIAN_POINT ( 'NONE',  ( 10.04305231718579705, 49.10000000546236976, 30.90933677959248982 ) ) ;
#841 = EDGE_CURVE ( 'NONE', #4493, #3462, #27944, .T. ) ;
#842 = CYLINDRICAL_SURFACE ( 'NONE', #18274, 32.50000000000000000 ) ;
#843 =( BOUNDED_CURVE ( )  B_SPLINE_CURVE ( 2, ( #8736, #29835, #998, #836, #5669, #11157, #16474, #18887, #11482, #8902, #19386, #16151, #24366 ),
 .UNSPECIFIED., .F., .T. ) 
 B_SPLINE_CURVE_WITH_KNOTS ( ( 3, 2, 2, 2, 2, 2, 3 ),
 ( 0.2756410256410256610, 0.2769230769230769384, 0.2794871794871794934, 0.2820512820512820484, 0.2846153846153846034, 0.2871794871794871584, 0.2884615384615384914 ),
 .UNSPECIFIED. ) 
 CURVE ( )  GEOMETRIC_REPRESENTATION_ITEM ( )  RATIONAL_B_SPLINE_CURVE ( ( 0.9755282581475768211, 0.9755282581475768211, 1.000000000000000000, 0.9510565162951535312, 1.000000000000000000, 0.9510565162951535312, 1.000000000000000000, 0.9510565162951535312, 1.000000000000000000, 0.9510565162951535312, 1.000000000000000000, 0.9755282581475762660, 0.9755282581475768211 ) ) 
 REPRESENTATION_ITEM ( '' )  );
#844 = CARTESIAN_POINT ( 'NONE',  ( -19.82091636218621034, 16.80000000000000782, -14.40073868116559552 ) ) ;
#845 = CARTESIAN_POINT ( 'NONE',  ( -27.95245687107222921, 28.75781249999999645, 2.498001805406602216E-13 ) ) ;
#846 = EDGE_CURVE ( 'NONE', #5395, #23148, #33249, .T. ) ;
#847 = CARTESIAN_POINT ( 'NONE',  ( -10.37757302488624411, 74.72500000273117848, -31.93888565452638417 ) ) ;
#848 = CARTESIAN_POINT ( 'NONE',  ( -7.505752307972844761, 28.04166666666666075, 28.01184896238304134 ) ) ;
#849 = CYLINDRICAL_SURFACE ( 'NONE', #14082, 24.50000000000000000 ) ;
#850 = ORIENTED_EDGE ( 'NONE', *, *, #11450, .F. ) ;
#851 = CARTESIAN_POINT ( 'NONE',  ( -28.00173670424549499, 50.96392333425730925, -7.543491769121417612 ) ) ;
#852 = AXIS2_PLACEMENT_3D ( 'NONE', #3223, #24155, #11436 ) ;
#853 = CARTESIAN_POINT ( 'NONE',  ( -26.29305231718578995, 14.70000000546238539, 19.10302069950538595 ) ) ;
#854 = CARTESIAN_POINT ( 'NONE',  ( -28.01184896238290278, 56.11458333333332860, 7.505752307973363457 ) ) ;
#855 = DIRECTION ( 'NONE',  ( 0.000000000000000000, -1.000000000000000000, 0.000000000000000000 ) ) ;
#856 = CARTESIAN_POINT ( 'NONE',  ( 6.486482029760649416E-15, 45.87500000273117706, 35.31076352940723240 ) ) ;
#857 = CARTESIAN_POINT ( 'NONE',  ( -20.08610463437157989, 52.20000000546236407, -27.64615127144129758 ) ) ;
#858 = CARTESIAN_POINT ( 'NONE',  ( -8.601468415847518756, 81.07500000273115859, -11.83890561707634781 ) ) ;
#859 = CARTESIAN_POINT ( 'NONE',  ( -27.16883889988624290, 36.92500000273118843, -19.73931689729374028 ) ) ;
#860 = CARTESIAN_POINT ( 'NONE',  ( 5.779280353836490358E-15, 24.50000000000000711, 32.49999999999999289 ) ) ;
#861 = CARTESIAN_POINT ( 'NONE',  ( 33.58253175000000823, 62.27500000273118275, 10.91162601494192863 ) ) ;
#862 = CARTESIAN_POINT ( 'NONE',  ( -10.04305231718578462, 40.39999999999999147, 30.90933677959249337 ) ) ;
#863 = CARTESIAN_POINT ( 'NONE',  ( 18.94512977948575738, 12.42499999726881477, 13.76444248337723408 ) ) ;
#864 = CARTESIAN_POINT ( 'NONE',  ( 27.16883889988624290, 6.175000002731190207, 19.73931689729373673 ) ) ;
#865 = DIRECTION ( 'NONE',  ( -0.5000000000000002220, 0.000000000000000000, -0.8660254037844384856 ) ) ;
#866 = CARTESIAN_POINT ( 'NONE',  ( -11.25946833292375793, 75.57500000273120122, 8.180482586598737171 ) ) ;
#867 = CARTESIAN_POINT ( 'NONE',  ( -20.75514604977248823, 73.07500000273115859, -28.56700777964554305 ) ) ;
#868 = FACE_OUTER_BOUND ( 'NONE', #18191, .T. ) ;
#869 = APPLICATION_CONTEXT ( 'automotive_design' ) ;
#870 = CARTESIAN_POINT ( 'NONE',  ( -33.58253175000000113, 71.47500000273119269, 10.91162601494193929 ) ) ;
#871 = VERTEX_POINT ( 'NONE', #20231 ) ;
#872 = CARTESIAN_POINT ( 'NONE',  ( 24.50000000000000355, 1.849999994537612436, -7.960532557706203605 ) ) ;
#873 = CARTESIAN_POINT ( 'NONE',  ( -6.950374756619716266, 13.72434000092397532, -26.09010956794232428 ) ) ;
#874 = CARTESIAN_POINT ( 'NONE',  ( -14.45873412499999944, 81.68750000136559208, 0.000000000000000000 ) ) ;
#875 = AXIS2_PLACEMENT_3D ( 'NONE', #13004, #5617, #5447 ) ;
#876 = CARTESIAN_POINT ( 'NONE',  ( 33.58253175000000113, 50.22500000273118559, -10.91162601494193751 ) ) ;
#877 = CARTESIAN_POINT ( 'NONE',  ( 27.16883889988624290, 10.17500000273117955, 19.73931689729373673 ) ) ;
#878 = CARTESIAN_POINT ( 'NONE',  ( 33.58253175000000823, 62.27500000273118985, 10.91162601494192685 ) ) ;
#879 = CARTESIAN_POINT ( 'NONE',  ( 19.09188309203661049, 54.10937499999999289, -19.09188309203694445 ) ) ;
#880 = CARTESIAN_POINT ( 'NONE',  ( -20.53372385742071771, 43.51600666759065206, 20.47846945139902530 ) ) ;
#881 = CARTESIAN_POINT ( 'NONE',  ( 28.02196122052058413, 25.74440999907601935, 7.468012846824272799 ) ) ;
#882 = CARTESIAN_POINT ( 'NONE',  ( -32.50000000000000000, 66.60000000546236265, 10.55989012756946366 ) ) ;
#883 = CARTESIAN_POINT ( 'NONE',  ( -11.25946833292375793, 79.07500000273121543, 8.180482586598737171 ) ) ;
#884 = CARTESIAN_POINT ( 'NONE',  ( 13.94119854578893580, 59.40326416574269075, -24.22776226481265383 ) ) ;
#885 = CARTESIAN_POINT ( 'NONE',  ( 7.236395654485760609, 13.02499999726880375, -22.27133577429736633 ) ) ;
#886 = ADVANCED_FACE ( 'NONE', ( #6499 ), #15076, .T. ) ;
#887 = ADVANCED_FACE ( 'NONE', ( #25022 ), #29271, .F. ) ;
#888 = ORIENTED_EDGE ( 'NONE', *, *, #28451, .T. ) ;
#889 = CARTESIAN_POINT ( 'NONE',  ( -27.16883889988623935, 49.57500000273120122, 19.73931689729374739 ) ) ;
#890 = CARTESIAN_POINT ( 'NONE',  ( -14.47279130897152299, 4.424999997268826313, 19.92008829642072243 ) ) ;
#891 = CARTESIAN_POINT ( 'NONE',  ( -24.22776226481240514, 47.09673583425730214, 13.94119854578937812 ) ) ;
#892 = CARTESIAN_POINT ( 'NONE',  ( -27.16883889988623935, 67.57500000273120122, 19.73931689729374739 ) ) ;
#893 = EDGE_LOOP ( 'NONE', ( #32042, #24575 ) ) ;
#894 = CARTESIAN_POINT ( 'NONE',  ( -10.37757302488623701, 19.52500000273120406, 31.93888565452638417 ) ) ;
#895 = CARTESIAN_POINT ( 'NONE',  ( -30.02300923189239512, 25.32031250000000000, 2.654126918244515359E-13 ) ) ;
#896 = ORIENTED_EDGE ( 'NONE', *, *, #24751, .F. ) ;
#897 = CARTESIAN_POINT ( 'NONE',  ( 5.147494310547481966, 65.94874572391552192, -32.49999999999998579 ) ) ;
#898 = CARTESIAN_POINT ( 'NONE',  ( 10.37757302488624767, 57.72500000273117848, 31.93888565452638417 ) ) ;
#899 = CARTESIAN_POINT ( 'NONE',  ( -26.00068869287368756, 56.54427083333332149, -15.01150461594595775 ) ) ;
#900 = CARTESIAN_POINT ( 'NONE',  ( 32.50000000000000711, 13.40000000546237047, 10.55989012756945122 ) ) ;
#901 = CARTESIAN_POINT ( 'NONE',  ( -20.08610463437157989, 66.20000000546238539, -27.64615127144129758 ) ) ;
#902 = CARTESIAN_POINT ( 'NONE',  ( 23.41746824999999887, 17.02499999726880731, 7.608796670333735079 ) ) ;
#903 = CARTESIAN_POINT ( 'NONE',  ( 33.58253175000000113, 24.37500000273118417, -4.112674001490185761E-15 ) ) ;
#904 = CARTESIAN_POINT ( 'NONE',  ( -10.04305231718578462, 24.90000000546238468, 30.90933677959249337 ) ) ;
#905 = CARTESIAN_POINT ( 'NONE',  ( -6.950374756619247307, 16.29128499907601579, 26.09010956794245217 ) ) ;
#906 = CARTESIAN_POINT ( 'NONE',  ( 32.50000000000000000, 65.50000000546239676, -3.980102097228898626E-15 ) ) ;
#907 = CARTESIAN_POINT ( 'NONE',  ( 0.000000000000000000, -12.99999999999999822, 0.000000000000000000 ) ) ;
#908 = VECTOR ( 'NONE', #32914, 1000.000000000000000 ) ;
#909 = CARTESIAN_POINT ( 'NONE',  ( 20.08610463437157279, 13.29999999999998650, -27.64615127144129758 ) ) ;
#910 = ORIENTED_EDGE ( 'NONE', *, *, #33041, .T. ) ;
#911 = CARTESIAN_POINT ( 'NONE',  ( 7.236395654485760609, 9.524999997268828622, -22.27133577429736633 ) ) ;
#912 = CARTESIAN_POINT ( 'NONE',  ( 13.91746824999999887, 75.87500000273116996, -1.704398294459741270E-15 ) ) ;
#913 = CARTESIAN_POINT ( 'NONE',  ( -6.988114217768288228, 43.22395833333332860, -26.07999730980477437 ) ) ;
#914 = CARTESIAN_POINT ( 'NONE',  ( 20.75514604977248467, 22.42500000273119909, -28.56700777964554305 ) ) ;
#915 = CARTESIAN_POINT ( 'NONE',  ( -33.58253175000000113, 69.22500000273117848, 10.91162601494193929 ) ) ;
#916 = CARTESIAN_POINT ( 'NONE',  ( 10.37757302488624767, 31.97500000273119269, 31.93888565452638417 ) ) ;
#917 = CARTESIAN_POINT ( 'NONE',  ( -27.16883889988623935, 19.57500000273119767, 19.73931689729374739 ) ) ;
#918 = CARTESIAN_POINT ( 'NONE',  ( 6.486482029760648627E-15, 9.875000002731187720, 35.31076352940722529 ) ) ;
#919 = CARTESIAN_POINT ( 'NONE',  ( -14.97647472619946285, 10.14361083425730925, -26.02091320914851025 ) ) ;
#920 = CARTESIAN_POINT ( 'NONE',  ( 28.01184896238304134, 54.68229166666665719, 7.505752307972846538 ) ) ;
#921 = CARTESIAN_POINT ( 'NONE',  ( 0.000000000000000000, 111.9999999999999858, 0.000000000000000000 ) ) ;
#922 = CARTESIAN_POINT ( 'NONE',  ( 8.601468415847520532, 78.07500000273118701, 11.83890561707634603 ) ) ;
#923 = CARTESIAN_POINT ( 'NONE',  ( 26.29305231718579350, 50.79999999999999716, 19.10302069950537529 ) ) ;
#924 = DIRECTION ( 'NONE',  ( 0.000000000000000000, 0.000000000000000000, -1.000000000000000000 ) ) ;
#925 = CARTESIAN_POINT ( 'NONE',  ( -27.16883889988624290, 48.92500000273120264, -19.73931689729374028 ) ) ;
#926 = CARTESIAN_POINT ( 'NONE',  ( -7.236395654485763274, 14.52499999726880553, 22.27133577429736633 ) ) ;
#927 = VERTEX_POINT ( 'NONE', #25192 ) ;
#928 = CARTESIAN_POINT ( 'NONE',  ( 20.75514604977249178, 68.07500000273118701, 28.56700777964553950 ) ) ;
#929 = CARTESIAN_POINT ( 'NONE',  ( -5.147494310547423346, 16.44874571845315359, 32.50000000000000000 ) ) ;
#930 = CARTESIAN_POINT ( 'NONE',  ( -14.47279130897152122, 5.924999997268808549, 19.92008829642072243 ) ) ;
#931 = CARTESIAN_POINT ( 'NONE',  ( 24.22776226481241224, 21.31548583425730925, -13.94119854578936923 ) ) ;
#932 = ORIENTED_EDGE ( 'NONE', *, *, #13358, .T. ) ;
#933 = AXIS2_PLACEMENT_3D ( 'NONE', #24052, #13238, #23712 ) ;
#934 = CARTESIAN_POINT ( 'NONE',  ( 20.75514604977248467, 34.42500000273117422, -28.56700777964554305 ) ) ;
#935 = CARTESIAN_POINT ( 'NONE',  ( -3.880418787951137816, 0.5512542815468468582, -24.49999999999999645 ) ) ;
#936 = ORIENTED_EDGE ( 'NONE', *, *, #9999, .F. ) ;
#937 = CARTESIAN_POINT ( 'NONE',  ( -7.505752307972844761, 48.66666666666666430, 28.01184896238304134 ) ) ;
#938 = CARTESIAN_POINT ( 'NONE',  ( -27.16883889988623935, 59.57500000273119412, 19.73931689729374739 ) ) ;
#939 = CARTESIAN_POINT ( 'NONE',  ( 5.147494310547426899, 69.94874572391553613, -32.50000000000000000 ) ) ;
#940 = CARTESIAN_POINT ( 'NONE',  ( -33.58253175000000113, 75.22500000273119269, 10.91162601494193929 ) ) ;
#941 = CARTESIAN_POINT ( 'NONE',  ( 20.50609665441005092, 30.90624999999999645, 20.50609665440969209 ) ) ;
#942 = CARTESIAN_POINT ( 'NONE',  ( -24.50000000000001066, 5.100000000000012967, 7.960532557706201828 ) ) ;
#943 = CARTESIAN_POINT ( 'NONE',  ( -2.162160676586881955E-15, 10.87500000273118417, -35.31076352940723240 ) ) ;
#944 = CARTESIAN_POINT ( 'NONE',  ( -33.58253175000000113, 17.12500000273120548, 0.000000000000000000 ) ) ;
#945 = CARTESIAN_POINT ( 'NONE',  ( -13.91746824999999532, 72.77500000273118985, -4.522059556121115875 ) ) ;
#946 = CARTESIAN_POINT ( 'NONE',  ( 26.02091320914876960, 39.63763916574268364, 14.97647472619900455 ) ) ;
#947 = CARTESIAN_POINT ( 'NONE',  ( -8.601468415847515203, 71.67500000273116711, 11.83890561707634959 ) ) ;
#948 = CARTESIAN_POINT ( 'NONE',  ( 26.00068869287367690, 44.51302083333332860, 15.01150461594596486 ) ) ;
#949 = EDGE_CURVE ( 'NONE', #9615, #21053, #27598, .T. ) ;
#950 = CARTESIAN_POINT ( 'NONE',  ( -26.29305231718579350, 54.30000000546237970, -19.10302069950537884 ) ) ;
#951 = CARTESIAN_POINT ( 'NONE',  ( -6.988114217768288228, 15.72395833333332860, -26.07999730980477437 ) ) ;
#952 = CARTESIAN_POINT ( 'NONE',  ( -33.58253175000000113, 45.12500000273117706, 0.000000000000000000 ) ) ;
#953 = CARTESIAN_POINT ( 'NONE',  ( 11.25946833292375793, 75.67500000273119554, 8.180482586598731842 ) ) ;
#954 = CARTESIAN_POINT ( 'NONE',  ( 27.16883889988624290, 46.17500000273118133, 19.73931689729373673 ) ) ;
#955 = CARTESIAN_POINT ( 'NONE',  ( -20.75514604977248112, 27.67500000273117777, 28.56700777964554661 ) ) ;
#956 = CARTESIAN_POINT ( 'NONE',  ( -6.700584085799521361, 16.99999999999998934, 23.28199799329060582 ) ) ;
#957 = CARTESIAN_POINT ( 'NONE',  ( -6.988114217767819270, 24.60416666666666430, 26.07999730980490583 ) ) ;
#958 = DIRECTION ( 'NONE',  ( -1.000000000000000000, 0.000000000000000000, 0.000000000000000000 ) ) ;
#959 = CARTESIAN_POINT ( 'NONE',  ( -12.13525491562421088, 75.80000000000001137, -8.816778784387096835 ) ) ;
#960 = CARTESIAN_POINT ( 'NONE',  ( 32.50000000000000000, 68.99999999999998579, -3.980102097228898626E-15 ) ) ;
#961 = CARTESIAN_POINT ( 'NONE',  ( -33.58253175000000113, 11.12500000273118594, 0.000000000000000000 ) ) ;
#962 = CARTESIAN_POINT ( 'NONE',  ( -7.236395654485757944, 7.224999997268804819, -22.27133577429736988 ) ) ;
#963 = CARTESIAN_POINT ( 'NONE',  ( -3.880418787951156023, 10.30125427608447453, -24.49999999999999645 ) ) ;
#964 = CARTESIAN_POINT ( 'NONE',  ( 27.95245687107223276, 32.47618083240936215, -0.04044903255042905932 ) ) ;
#965 = CARTESIAN_POINT ( 'NONE',  ( -9.270509831248419985, 76.55000000546239391, 12.75976212528060039 ) ) ;
#966 = CARTESIAN_POINT ( 'NONE',  ( -27.16883889988624290, 16.92500000273117067, -19.73931689729374028 ) ) ;
#967 = CARTESIAN_POINT ( 'NONE',  ( -4.523095164977116484E-15, 4.624999997268820273, 24.62258325217400312 ) ) ;
#968 = CARTESIAN_POINT ( 'NONE',  ( 27.95245687107222921, 51.10156249999998579, -2.463307335887066074E-13 ) ) ;
#969 = VERTEX_POINT ( 'NONE', #14731 ) ;
#970 = CARTESIAN_POINT ( 'NONE',  ( 10.37757302488624056, 58.52500000273118275, -31.93888565452638417 ) ) ;
#971 = CARTESIAN_POINT ( 'NONE',  ( -33.58253175000000113, 29.27500000273118630, -10.91162601494193218 ) ) ;
#972 = ORIENTED_EDGE ( 'NONE', *, *, #6119, .F. ) ;
#973 = CARTESIAN_POINT ( 'NONE',  ( -20.50609665440969209, 24.89062500000000000, 20.50609665441005092 ) ) ;
#974 = CARTESIAN_POINT ( 'NONE',  ( 7.468012846824777284, 22.31809000092397000, 28.02196122052045268 ) ) ;
#975 = CARTESIAN_POINT ( 'NONE',  ( 24.50000000000000000, 15.84999999453763664, -7.960532557706203605 ) ) ;
#976 = CARTESIAN_POINT ( 'NONE',  ( -24.50000000000000000, 16.74999999453763522, -3.000384657911015469E-15 ) ) ;
#977 = CARTESIAN_POINT ( 'NONE',  ( -18.94512977948575738, 5.424999997268809437, -13.76444248337723231 ) ) ;
#978 = CARTESIAN_POINT ( 'NONE',  ( -10.37757302488624411, 30.97500000273117848, -31.93888565452638417 ) ) ;
#979 = CARTESIAN_POINT ( 'NONE',  ( -32.50000000000000000, 28.40000000546235981, -10.55989012756945478 ) ) ;
#980 = CARTESIAN_POINT ( 'NONE',  ( -26.29305231718579350, 73.80000000000001137, -19.10302069950537884 ) ) ;
#981 = CARTESIAN_POINT ( 'NONE',  ( -7.570916362186210335, 10.59999999999999787, -23.30088464923126779 ) ) ;
#982 = CARTESIAN_POINT ( 'NONE',  ( -7.468012846824771955, 58.41184000092398065, -28.02196122052045624 ) ) ;
#983 = CARTESIAN_POINT ( 'NONE',  ( -33.58253175000000113, 43.37500000273119838, 0.000000000000000000 ) ) ;
#984 = CARTESIAN_POINT ( 'NONE',  ( -14.47279130897152122, 12.42499999726880766, 19.92008829642072243 ) ) ;
#985 = CARTESIAN_POINT ( 'NONE',  ( 32.50000000000000000, 13.00000000000001066, -3.980102097228898626E-15 ) ) ;
#986 = CARTESIAN_POINT ( 'NONE',  ( -24.50000000000000355, 14.89999999999999680, -7.960532557706207157 ) ) ;
#987 = CARTESIAN_POINT ( 'NONE',  ( -0.04044903255042732459, 41.92930583240936215, -27.95245687107223986 ) ) ;
#988 = CARTESIAN_POINT ( 'NONE',  ( 27.16883889988624290, 63.92500000273118843, 19.73931689729373673 ) ) ;
#989 = CARTESIAN_POINT ( 'NONE',  ( -10.37757302488623701, 45.77500000273118985, 31.93888565452638417 ) ) ;
#990 = CARTESIAN_POINT ( 'NONE',  ( -7.236395654485763274, 10.02499999726880198, 22.27133577429736633 ) ) ;
#991 = CARTESIAN_POINT ( 'NONE',  ( -1.756012107511856980E-14, 4.499999999999997335, -24.50000000000000000 ) ) ;
#992 = CARTESIAN_POINT ( 'NONE',  ( -33.58253175000000113, 3.225000002731193138, 10.91162601494193929 ) ) ;
#993 = CARTESIAN_POINT ( 'NONE',  ( -14.01125832528285109, 39.93527750092397355, 24.18731323226248264 ) ) ;
#994 = CARTESIAN_POINT ( 'NONE',  ( 19.05376897654620194, 16.99999999999997868, -13.63518129362208953 ) ) ;
#995 = CARTESIAN_POINT ( 'NONE',  ( -8.342407680043393725, 52.00000000000000711, 32.16802901964487660 ) ) ;
#996 = PRODUCT_DEFINITION_CONTEXT ( 'detailed design', #19086, 'design' ) ;
#997 = CARTESIAN_POINT ( 'NONE',  ( -33.58253175000000113, 29.22500000273118914, 10.91162601494193929 ) ) ;
#998 = CARTESIAN_POINT ( 'NONE',  ( -10.04305231718578462, 56.90000000546240244, 30.90933677959249337 ) ) ;
#999 = CARTESIAN_POINT ( 'NONE',  ( 5.147494310547426899, 61.94874572391552192, -32.50000000000000000 ) ) ;
#1000 = DIRECTION ( 'NONE',  ( -1.224646799147353454E-16, 1.000000000000000000, -0.000000000000000000 ) ) ;
#1001 = CARTESIAN_POINT ( 'NONE',  ( 7.543491769121922985, 57.25482666574269075, 28.00173670424535644 ) ) ;
#1002 = CARTESIAN_POINT ( 'NONE',  ( 32.50000000000000000, 49.50000000546238255, -3.980102097228898626E-15 ) ) ;
#1003 = CARTESIAN_POINT ( 'NONE',  ( -4.300734207923755825, 71.77500000273117564, 13.23629886949340673 ) ) ;
#1004 = DIRECTION ( 'NONE',  ( -0.000000000000000000, -1.000000000000000000, -0.000000000000000000 ) ) ;
#1005 = CARTESIAN_POINT ( 'NONE',  ( 26.07999730980477437, 26.89583333333332860, -6.988114217768290004 ) ) ;
#1006 = CARTESIAN_POINT ( 'NONE',  ( 27.16883889988623935, 76.32500000273120122, -19.73931689729374384 ) ) ;
#1007 = CARTESIAN_POINT ( 'NONE',  ( 15.01150461594596308, 29.90364583333332504, -26.00068869287367335 ) ) ;
#1008 = DIRECTION ( 'NONE',  ( 0.000000000000000000, -1.000000000000000000, 0.000000000000000000 ) ) ;
#1009 = EDGE_LOOP ( 'NONE', ( #6385, #19811, #24661, #9041 ) ) ;
#1010 = CARTESIAN_POINT ( 'NONE',  ( 26.02091320914851025, 48.81548583425731636, -14.97647472619946463 ) ) ;
#1011 = CARTESIAN_POINT ( 'NONE',  ( -32.50000000000000000, 10.40000000546237935, -10.55989012756945478 ) ) ;
#1012 = CARTESIAN_POINT ( 'NONE',  ( -30.02300923189239512, 63.13281250000000000, 2.654126918244515359E-13 ) ) ;
#1013 = CARTESIAN_POINT ( 'NONE',  ( 20.08610463437158344, 20.69999999999998508, 27.64615127144129403 ) ) ;
#1014 = CARTESIAN_POINT ( 'NONE',  ( -33.58253175000000113, 49.27500000273118985, -10.91162601494193218 ) ) ;
#1015 = CARTESIAN_POINT ( 'NONE',  ( 10.04305231718579705, 47.10000000546238397, 30.90933677959248982 ) ) ;
#1016 = CARTESIAN_POINT ( 'NONE',  ( -12.13525491562421088, 81.79999999999998295, -8.816778784387096835 ) ) ;
#1017 = CARTESIAN_POINT ( 'NONE',  ( -20.75514604977248823, 36.82500000273117990, -28.56700777964554305 ) ) ;
#1018 = CARTESIAN_POINT ( 'NONE',  ( -10.04305231718579172, 62.10000000546238397, -30.90933677959248982 ) ) ;
#1019 = CARTESIAN_POINT ( 'NONE',  ( 27.16883889988624290, 60.17500000273118133, 19.73931689729373673 ) ) ;
#1020 = SURFACE_STYLE_USAGE ( .BOTH. , #4120 ) ;
#1021 = CARTESIAN_POINT ( 'NONE',  ( 26.29305231718578995, 37.19999999999999574, -19.10302069950538240 ) ) ;
#1022 = CARTESIAN_POINT ( 'NONE',  ( 10.04305231718579705, 40.59999999999999432, 30.90933677959248982 ) ) ;
#1023 = CARTESIAN_POINT ( 'NONE',  ( 18.94512977948576093, 12.82499999726882578, -13.76444248337722875 ) ) ;
#1024 = EDGE_CURVE ( 'NONE', #11003, #21772, #28714, .T. ) ;
#1025 = CARTESIAN_POINT ( 'NONE',  ( -33.58253175000000113, 1.375000002731191495, 0.000000000000000000 ) ) ;
#1026 = CARTESIAN_POINT ( 'NONE',  ( -8.761981113183991350E-16, -15.84529946162075298, 0.000000000000000000 ) ) ;
#1027 = CARTESIAN_POINT ( 'NONE',  ( -13.91746824999999887, 79.37500000273118417, 0.000000000000000000 ) ) ;
#1028 = CARTESIAN_POINT ( 'NONE',  ( -27.16883889988623935, 71.57500000273120122, 19.73931689729374739 ) ) ;
#1029 = FACE_OUTER_BOUND ( 'NONE', #7707, .T. ) ;
#1030 = EDGE_CURVE ( 'NONE', #9545, #23066, #12266, .T. ) ;
#1031 = CARTESIAN_POINT ( 'NONE',  ( 20.75514604977249178, 66.07500000273118701, 28.56700777964553950 ) ) ;
#1032 = ORIENTED_EDGE ( 'NONE', *, *, #9068, .F. ) ;
#1033 = CARTESIAN_POINT ( 'NONE',  ( 24.50000000000000000, 5.749999994537624559, 0.000000000000000000 ) ) ;
#1034 = CARTESIAN_POINT ( 'NONE',  ( -26.09010956794232428, 16.30246500092397355, 6.950374756619732253 ) ) ;
#1035 = CARTESIAN_POINT ( 'NONE',  ( 2.445080149700053643E-15, 74.50000000000001421, 15.00000000000000000 ) ) ;
#1036 = CARTESIAN_POINT ( 'NONE',  ( 33.58253175000000823, 50.02500000273118985, 10.91162601494192863 ) ) ;
#1037 = CARTESIAN_POINT ( 'NONE',  ( 20.75514604977249178, 14.07500000273119944, 28.56700777964553950 ) ) ;
#1038 = CARTESIAN_POINT ( 'NONE',  ( 33.58253175000000113, 60.47500000273118559, -10.91162601494193574 ) ) ;
#1039 = CARTESIAN_POINT ( 'NONE',  ( 26.07999730980477437, 47.52083333333332860, -6.988114217768290004 ) ) ;
#1040 = CARTESIAN_POINT ( 'NONE',  ( -7.543491769121417612, 36.35454833425730925, 28.00173670424549499 ) ) ;
#1041 = CARTESIAN_POINT ( 'NONE',  ( -26.02091320914878025, 24.16888916574269075, -14.97647472619899389 ) ) ;
#1042 = CARTESIAN_POINT ( 'NONE',  ( 26.29305231718579350, 67.30000000546236549, 19.10302069950537529 ) ) ;
#1043 = CARTESIAN_POINT ( 'NONE',  ( 8.601468415847520532, 77.57500000273115859, 11.83890561707634781 ) ) ;
#1044 = CARTESIAN_POINT ( 'NONE',  ( 24.22776226481265383, 60.26263916574269786, 13.94119854578893580 ) ) ;
#1045 = FACE_OUTER_BOUND ( 'NONE', #30735, .T. ) ;
#1046 = CARTESIAN_POINT ( 'NONE',  ( -7.570916362186215665, 17.39999999999999858, 23.30088464923126423 ) ) ;
#1047 = ORIENTED_EDGE ( 'NONE', *, *, #18602, .T. ) ;
#1048 = CARTESIAN_POINT ( 'NONE',  ( 10.37757302488624767, 41.97500000273117138, 31.93888565452638417 ) ) ;
#1049 = CARTESIAN_POINT ( 'NONE',  ( -23.41746825000000243, 4.224999997268803931, 7.608796670333725309 ) ) ;
#1050 = CARTESIAN_POINT ( 'NONE',  ( 6.277390505771533514E-15, 33.00000000546238255, 34.17252228774368916 ) ) ;
#1051 = ORIENTED_EDGE ( 'NONE', *, *, #15985, .F. ) ;
#1052 = CARTESIAN_POINT ( 'NONE',  ( 10.37757302488624767, 17.72500000273118204, 31.93888565452638417 ) ) ;
#1053 = CARTESIAN_POINT ( 'NONE',  ( -28.01184896238290278, 32.05208333333332860, 7.505752307973363457 ) ) ;
#1054 = ORIENTED_EDGE ( 'NONE', *, *, #1897, .T. ) ;
#1055 = ORIENTED_EDGE ( 'NONE', *, *, #4319, .F. ) ;
#1056 = CARTESIAN_POINT ( 'NONE',  ( -20.08610463437156923, 48.80000000546236549, 27.64615127144130113 ) ) ;
#1057 = CARTESIAN_POINT ( 'NONE',  ( 27.16883889988624290, 53.92500000273120264, 19.73931689729373673 ) ) ;
#1058 = CARTESIAN_POINT ( 'NONE',  ( 7.505752307972854531, 53.82291666666666430, -28.01184896238303423 ) ) ;
#1059 = CARTESIAN_POINT ( 'NONE',  ( 32.50000000000000000, 13.50000000546236478, -3.980102097228898626E-15 ) ) ;
#1060 = CARTESIAN_POINT ( 'NONE',  ( 15.14183272437242067, 15.44999999453762207, 20.84094480462498211 ) ) ;
#1061 = CARTESIAN_POINT ( 'NONE',  ( -18.94512977948576093, 16.32499999726880091, 13.76444248337722698 ) ) ;
#1062 = CARTESIAN_POINT ( 'NONE',  ( 32.50000000000000000, 57.09999999999999432, -10.55989012756945833 ) ) ;
#1063 = EDGE_CURVE ( 'NONE', #21883, #11212, #23262, .T. ) ;
#1064 = CARTESIAN_POINT ( 'NONE',  ( -2.162160676586881955E-15, 24.87500000273117351, -35.31076352940723240 ) ) ;
#1065 = CARTESIAN_POINT ( 'NONE',  ( 2.375766604868043252, 77.44874571845313938, -14.99999999999999822 ) ) ;
#1066 = CARTESIAN_POINT ( 'NONE',  ( 20.53372385742108008, 67.28086833240935505, 20.47846945139866648 ) ) ;
#1067 = CARTESIAN_POINT ( 'NONE',  ( 13.91746825000000065, 75.77500000273120406, 4.522059556121114987 ) ) ;
#1068 = CARTESIAN_POINT ( 'NONE',  ( -7.570916362186215665, 1.400000000000012346, 23.30088464923126423 ) ) ;
#1069 = DIRECTION ( 'NONE',  ( 0.000000000000000000, 1.000000000000000000, 0.000000000000000000 ) ) ;
#1070 = CARTESIAN_POINT ( 'NONE',  ( -20.08610463437157989, 11.70000000000000995, -27.64615127144129758 ) ) ;
#1071 = ORIENTED_EDGE ( 'NONE', *, *, #11450, .T. ) ;
#1072 = CARTESIAN_POINT ( 'NONE',  ( -14.47279130897151589, 7.824999997268807128, -19.92008829642072598 ) ) ;
#1073 = CARTESIAN_POINT ( 'NONE',  ( 8.601468415847520532, 75.57500000273120122, 11.83890561707634781 ) ) ;
#1074 = CARTESIAN_POINT ( 'NONE',  ( -6.988114217767819270, 38.35416666666666430, 26.07999730980490583 ) ) ;
#1075 = CARTESIAN_POINT ( 'NONE',  ( 33.58253175000000823, 18.02500000273118630, 10.91162601494192863 ) ) ;
#1076 = CARTESIAN_POINT ( 'NONE',  ( -27.16883889988624290, 66.92500000273119554, -19.73931689729374028 ) ) ;
#1077 = CARTESIAN_POINT ( 'NONE',  ( 27.16883889988624290, 32.17500000273120264, 19.73931689729373673 ) ) ;
#1078 = CARTESIAN_POINT ( 'NONE',  ( -10.37757302488624411, 14.97500000273120691, -31.93888565452638417 ) ) ;
#1079 = CARTESIAN_POINT ( 'NONE',  ( -33.58253175000000113, 9.275000002731177418, -10.91162601494193041 ) ) ;
#1080 = CARTESIAN_POINT ( 'NONE',  ( 7.543491769121427382, 10.57329833425730747, -28.00173670424548433 ) ) ;
#1081 = CARTESIAN_POINT ( 'NONE',  ( 7.505752307972854531, 50.38541666666666430, -28.01184896238303423 ) ) ;
#1082 = CARTESIAN_POINT ( 'NONE',  ( -7.579748464070165821E-14, 16.50000000000000355, -24.50000000000000000 ) ) ;
#1083 = CARTESIAN_POINT ( 'NONE',  ( -8.601468415847518756, 77.07500000273118701, -11.83890561707634603 ) ) ;
#1084 = CARTESIAN_POINT ( 'NONE',  ( 10.04305231718578817, 49.39999999999998437, -30.90933677959249337 ) ) ;
#1085 = CARTESIAN_POINT ( 'NONE',  ( -7.570916362186210335, 2.349999994537638415, -23.30088464923126779 ) ) ;
#1086 = CARTESIAN_POINT ( 'NONE',  ( 20.75514604977249178, 51.82500000273120122, 28.56700777964553950 ) ) ;
#1087 = CARTESIAN_POINT ( 'NONE',  ( 23.41746825000000243, 17.22499999726880304, -7.608796670333727974 ) ) ;
#1088 = VERTEX_POINT ( 'NONE', #12842 ) ;
#1089 = CARTESIAN_POINT ( 'NONE',  ( -33.58253175000000113, 69.27500000273116143, -10.91162601494193218 ) ) ;
#1090 = CYLINDRICAL_SURFACE ( 'NONE', #17945, 32.50000000000000000 ) ;
#1091 = CARTESIAN_POINT ( 'NONE',  ( -23.41746825000000243, 7.524999997268816188, -7.608796670333730638 ) ) ;
#1092 = CARTESIAN_POINT ( 'NONE',  ( -24.18731323226248264, 20.16965250092397355, -14.01125832528284931 ) ) ;
#1093 = EDGE_LOOP ( 'NONE', ( #6927, #11913, #5390 ) ) ;
#1094 = CARTESIAN_POINT ( 'NONE',  ( -20.75514604977248112, 39.42500000273118843, 28.56700777964554661 ) ) ;
#1095 = CARTESIAN_POINT ( 'NONE',  ( -24.50000000000000000, 0.9000000000000005773, -7.960532557706207157 ) ) ;
#1096 = EDGE_LOOP ( 'NONE', ( #14624, #31167 ) ) ;
#1097 = CARTESIAN_POINT ( 'NONE',  ( 28.01184896238304134, 51.24479166666666430, 7.505752307972846538 ) ) ;
#1098 = CARTESIAN_POINT ( 'NONE',  ( 33.58253175000000113, 58.37500000273118417, -4.112674001490185761E-15 ) ) ;
#1099 = CARTESIAN_POINT ( 'NONE',  ( 2.375766604868046361, 74.80125428700921475, 14.99999999999999822 ) ) ;
#1100 = CARTESIAN_POINT ( 'NONE',  ( -10.37757302488624411, 72.72500000273119269, -31.93888565452638417 ) ) ;
#1101 = CARTESIAN_POINT ( 'NONE',  ( 30.02300923189239512, 33.91406249999997158, -2.619432448724977703E-13 ) ) ;
#1102 = CARTESIAN_POINT ( 'NONE',  ( -24.50000000000001066, 3.099999999999989875, 7.960532557706201828 ) ) ;
#1103 = CARTESIAN_POINT ( 'NONE',  ( -33.58253175000000113, 5.275000002731187188, -10.91162601494193218 ) ) ;
#1104 = CARTESIAN_POINT ( 'NONE',  ( 10.37757302488624767, 19.72500000273119625, 31.93888565452638417 ) ) ;
#1105 = CARTESIAN_POINT ( 'NONE',  ( -8.891200544363830713E-16, 77.49999999999998579, -15.00000000000000000 ) ) ;
#1106 = CARTESIAN_POINT ( 'NONE',  ( 15.04653450569339945, 39.92409749907602645, 25.98046417659831775 ) ) ;
#1107 = CARTESIAN_POINT ( 'NONE',  ( 13.91746824999999532, 72.47500000273119269, -4.522059556121118540 ) ) ;
#1108 = CARTESIAN_POINT ( 'NONE',  ( 2.740863092043355209E-13, 62.27343749999999289, 30.02300923189239867 ) ) ;
#1109 = CARTESIAN_POINT ( 'NONE',  ( -15.14183272437242067, 16.44999999453761674, -20.84094480462497856 ) ) ;
#1110 = CARTESIAN_POINT ( 'NONE',  ( 7.313012447739250820E-14, 15.50000000000000178, 24.50000000000000000 ) ) ;
#1111 = CARTESIAN_POINT ( 'NONE',  ( 19.09188309203694800, 17.15624999999999645, 19.09188309203660694 ) ) ;
#1112 = CARTESIAN_POINT ( 'NONE',  ( -2.162160676586881955E-15, 34.62500000273119127, -35.31076352940723240 ) ) ;
#1113 = CARTESIAN_POINT ( 'NONE',  ( -13.91746824999999532, 76.97500000273119269, 4.522059556121122093 ) ) ;
#1114 = CARTESIAN_POINT ( 'NONE',  ( -2.162160676586881955E-15, 50.87500000273119838, -35.31076352940723240 ) ) ;
#1115 = CARTESIAN_POINT ( 'NONE',  ( -33.58253175000000113, 31.47500000273117138, 10.91162601494193929 ) ) ;
#1116 = CARTESIAN_POINT ( 'NONE',  ( 20.86390607985937606, 16.99999999999997868, 10.74782858706267952 ) ) ;
#1117 = CARTESIAN_POINT ( 'NONE',  ( 26.07999730980490227, 30.61979166666666075, 6.988114217767821046 ) ) ;
#1118 = CARTESIAN_POINT ( 'NONE',  ( 0.000000000000000000, 52.00000000000000711, 0.000000000000000000 ) ) ;
#1119 = CARTESIAN_POINT ( 'NONE',  ( -5.147494310547430452, 44.05125428700922896, -32.49999999999999289 ) ) ;
#1120 = CARTESIAN_POINT ( 'NONE',  ( 32.50000000000000711, 68.90000000000001990, 10.55989012756945122 ) ) ;
#1121 = CARTESIAN_POINT ( 'NONE',  ( -10.37757302488623701, 7.525000002731194293, 31.93888565452638417 ) ) ;
#1122 = CARTESIAN_POINT ( 'NONE',  ( 18.94512977948576093, 2.824999997268817786, -13.76444248337722875 ) ) ;
#1123 = CARTESIAN_POINT ( 'NONE',  ( 30.02300923189239867, 22.16368083240936215, -0.04044903255044467877 ) ) ;
#1124 = CARTESIAN_POINT ( 'NONE',  ( 3.000384657911015469E-15, 0.000000000000000000, -24.50000000000000000 ) ) ;
#1125 = CARTESIAN_POINT ( 'NONE',  ( 0.04044903255044120238, 29.89805583240935860, 27.95245687107223276 ) ) ;
#1126 = CARTESIAN_POINT ( 'NONE',  ( -9.270509831248423538, 75.95000000546238539, -12.75976212528059861 ) ) ;
#1127 = CARTESIAN_POINT ( 'NONE',  ( -10.37757302488624411, 12.72500000273119092, -31.93888565452638417 ) ) ;
#1128 = CARTESIAN_POINT ( 'NONE',  ( 18.94512977948575738, 6.924999997268810326, 13.76444248337723408 ) ) ;
#1129 = CARTESIAN_POINT ( 'NONE',  ( 24.20753774853731244, 50.81510416666667140, -13.97622843553632599 ) ) ;
#1130 = ORIENTED_EDGE ( 'NONE', *, *, #31881, .F. ) ;
#1131 = CARTESIAN_POINT ( 'NONE',  ( 27.16883889988624290, 53.92500000273118843, 19.73931689729373673 ) ) ;
#1132 = CARTESIAN_POINT ( 'NONE',  ( -27.16883889988624290, 27.17500000273119554, -19.73931689729374028 ) ) ;
#1133 = VERTEX_POINT ( 'NONE', #31022 ) ;
#1134 = CARTESIAN_POINT ( 'NONE',  ( 30.02300923189239512, 23.60156250000000000, -2.619432448724977703E-13 ) ) ;
#1135 = CARTESIAN_POINT ( 'NONE',  ( -14.97647472619946285, 27.33111083425731280, -26.02091320914851025 ) ) ;
#1136 = AXIS2_PLACEMENT_3D ( 'NONE', #18668, #12050, #13680 ) ;
#1137 = CIRCLE ( 'NONE', #17065, 10.11000150615022264 ) ;
#1138 = CARTESIAN_POINT ( 'NONE',  ( 10.04305231718579705, 38.59999999999999432, 30.90933677959248982 ) ) ;
#1139 = CARTESIAN_POINT ( 'NONE',  ( -24.50000000000000355, 18.64999999453763380, -7.960532557706207157 ) ) ;
#1140 = CARTESIAN_POINT ( 'NONE',  ( -23.41746825000000598, 5.724999997268815477, 7.608796670333726198 ) ) ;
#1141 = CARTESIAN_POINT ( 'NONE',  ( -10.37757302488624411, 20.97500000273119625, -31.93888565452638417 ) ) ;
#1142 = CARTESIAN_POINT ( 'NONE',  ( -26.29305231718579350, 30.30000000546237260, -19.10302069950537884 ) ) ;
#1143 = CARTESIAN_POINT ( 'NONE',  ( 26.29305231718578995, 71.19999999999998863, -19.10302069950538240 ) ) ;
#1144 = LINE ( 'NONE', #19370, #25835 ) ;
#1145 = CARTESIAN_POINT ( 'NONE',  ( -15.14183272437242778, 11.29999999999999361, 20.84094480462497856 ) ) ;
#1146 = CARTESIAN_POINT ( 'NONE',  ( -15.04653450569291984, 60.56027750092398065, 25.98046417659859486 ) ) ;
#1147 = CARTESIAN_POINT ( 'NONE',  ( 33.58253175000000113, 38.37500000273119838, -4.112674001490185761E-15 ) ) ;
#1148 = CARTESIAN_POINT ( 'NONE',  ( -33.58253175000000113, 57.02500000273118275, -10.91162601494193041 ) ) ;
#1149 = CARTESIAN_POINT ( 'NONE',  ( -15.01150461594642316, 25.89322916666666430, -26.00068869287341045 ) ) ;
#1150 =( NAMED_UNIT ( * ) PLANE_ANGLE_UNIT ( ) SI_UNIT ( $, .RADIAN. ) );
#1151 = CARTESIAN_POINT ( 'NONE',  ( 18.94512977948576093, 7.324999997268822227, -13.76444248337722875 ) ) ;
#1152 = CARTESIAN_POINT ( 'NONE',  ( 26.29305231718578995, 13.19999999999998863, -19.10302069950538240 ) ) ;
#1153 = CARTESIAN_POINT ( 'NONE',  ( 24.50000000000000000, 12.00000000000001066, 0.000000000000000000 ) ) ;
#1154 = CARTESIAN_POINT ( 'NONE',  ( 27.95245687107223276, 42.78868083240935505, -0.04044903255042905932 ) ) ;
#1155 = CARTESIAN_POINT ( 'NONE',  ( 27.16883889988623935, 60.32500000273119412, -19.73931689729374384 ) ) ;
#1156 = CARTESIAN_POINT ( 'NONE',  ( -20.75514604977248823, 45.07500000273117990, -28.56700777964554305 ) ) ;
#1157 = CARTESIAN_POINT ( 'NONE',  ( -14.47279130897152299, 11.92499999726882187, 19.92008829642072243 ) ) ;
#1158 = ADVANCED_FACE ( 'NONE', ( #10099 ), #7341, .F. ) ;
#1159 = CARTESIAN_POINT ( 'NONE',  ( 19.82091636218621389, 3.949999994537628289, -14.40073868116559197 ) ) ;
#1160 = CARTESIAN_POINT ( 'NONE',  ( 27.16883889988623935, 4.325000002731171911, -19.73931689729374384 ) ) ;
#1161 = CARTESIAN_POINT ( 'NONE',  ( 24.18731323226247554, 42.51340250092398065, 14.01125832528285997 ) ) ;
#1162 = CARTESIAN_POINT ( 'NONE',  ( 30.93003301939247152, 66.99999999999998579, -10.64619209630829211 ) ) ;
#1163 = DIRECTION ( 'NONE',  ( 0.2588190451025240146, -0.9659258262890673130, 0.000000000000000000 ) ) ;
#1164 = CARTESIAN_POINT ( 'NONE',  ( 33.58253175000000113, 26.22500000273119625, -10.91162601494193751 ) ) ;
#1166 = AXIS2_PLACEMENT_3D ( 'NONE', #29236, #16220, #24104 ) ;
#1165 = FACE_OUTER_BOUND ( 'NONE', #17941, .T. ) ;
#1167 = CARTESIAN_POINT ( 'NONE',  ( -14.45873412499999944, 71.68750000136559208, 0.000000000000000000 ) ) ;
#1168 = EDGE_CURVE ( 'NONE', #33174, #33755, #10608, .T. ) ;
#1169 = CYLINDRICAL_SURFACE ( 'NONE', #10005, 15.00000000000000000 ) ;
#1170 = EDGE_CURVE ( 'NONE', #17032, #21850, #8028, .T. ) ;
#1171 = CARTESIAN_POINT ( 'NONE',  ( 25.98046417659831775, 59.68972249907602645, -15.04653450569338879 ) ) ;
#1172 = CARTESIAN_POINT ( 'NONE',  ( 10.04305231718579705, 51.10000000546236976, 30.90933677959248982 ) ) ;
#1173 = CARTESIAN_POINT ( 'NONE',  ( -1.778240108872766143E-15, 58.00000000546237544, -32.49999999999999289 ) ) ;
#1174 = CARTESIAN_POINT ( 'NONE',  ( 13.97622843553633665, 24.17447916666666785, 24.20753774853730889 ) ) ;
#1175 = ORIENTED_EDGE ( 'NONE', *, *, #13369, .F. ) ;
#1176 = CARTESIAN_POINT ( 'NONE',  ( 33.58253175000000113, 72.22500000273119269, -10.91162601494193751 ) ) ;
#1177 = CARTESIAN_POINT ( 'NONE',  ( 7.505752307973351023, 34.63020833333332860, 28.01184896238290278 ) ) ;
#1178 = CARTESIAN_POINT ( 'NONE',  ( 3.000384657911015469E-15, 0.000000000000000000, -24.50000000000000000 ) ) ;
#1179 = VERTEX_POINT ( 'NONE', #5114 ) ;
#1180 = CARTESIAN_POINT ( 'NONE',  ( -0.04044903254990864921, 53.39881916759064495, 30.02300923189239867 ) ) ;
#1181 = CARTESIAN_POINT ( 'NONE',  ( -10.04305231718579172, 10.10000000546239285, -30.90933677959248982 ) ) ;
#1182 = CARTESIAN_POINT ( 'NONE',  ( 20.50609665441005092, 58.40625000000000711, 20.50609665440969209 ) ) ;
#1183 = CARTESIAN_POINT ( 'NONE',  ( -5.147494310547423346, 64.94874572391549350, 32.50000000000000000 ) ) ;
#1184 = CARTESIAN_POINT ( 'NONE',  ( 27.16883889988623935, 44.57500000273117990, -19.73931689729374384 ) ) ;
#1185 = CARTESIAN_POINT ( 'NONE',  ( 6.277390505771533514E-15, 51.00000000546238255, 34.17252228774368916 ) ) ;
#1186 = CARTESIAN_POINT ( 'NONE',  ( 13.91746825000000065, 72.27500000273116143, 4.522059556121114987 ) ) ;
#1187 = CARTESIAN_POINT ( 'NONE',  ( 10.37757302488624056, 30.52500000273117209, -31.93888565452638417 ) ) ;
#1188 = CARTESIAN_POINT ( 'NONE',  ( 32.50000000000000711, 77.40000000546238823, 10.55989012756945122 ) ) ;
#1189 = CARTESIAN_POINT ( 'NONE',  ( -10.37757302488623701, 57.77500000273119696, 31.93888565452638417 ) ) ;
#1190 =( NAMED_UNIT ( * ) PLANE_ANGLE_UNIT ( ) SI_UNIT ( $, .RADIAN. ) );
#1191 = CARTESIAN_POINT ( 'NONE',  ( -20.08610463437156923, 34.29999999999998295, 27.64615127144130113 ) ) ;
#1192 = CARTESIAN_POINT ( 'NONE',  ( 20.08610463437158344, 32.69999999999998863, 27.64615127144129403 ) ) ;
#1193 = CARTESIAN_POINT ( 'NONE',  ( -4.523095164977116484E-15, 10.12499999726881938, 24.62258325217400312 ) ) ;
#1194 = CARTESIAN_POINT ( 'NONE',  ( 20.75514604977248467, 4.675000002731176885, -28.56700777964554305 ) ) ;
#1195 = DIRECTION ( 'NONE',  ( -1.000000000000000000, 0.000000000000000000, 0.000000000000000000 ) ) ;
#1196 = CARTESIAN_POINT ( 'NONE',  ( -11.25946833292375793, 77.17500000273119554, -8.180482586598733619 ) ) ;
#1197 = CARTESIAN_POINT ( 'NONE',  ( 33.58253175000000113, 64.47500000273120691, -10.91162601494193574 ) ) ;
#1198 = CARTESIAN_POINT ( 'NONE',  ( -3.880418787951099180, 18.30125427608446387, -24.50000000000001421 ) ) ;
#1199 = ORIENTED_EDGE ( 'NONE', *, *, #16507, .F. ) ;
#1200 = CARTESIAN_POINT ( 'NONE',  ( 24.50000000000000355, 7.649999994537632908, 7.960532557706212486 ) ) ;
#1201 = CARTESIAN_POINT ( 'NONE',  ( -19.09188309203694445, 67.00000000000000000, -19.09188309203661049 ) ) ;
#1202 = CARTESIAN_POINT ( 'NONE',  ( 5.779280353836490358E-15, 5.000000005462372776, 32.49999999999999289 ) ) ;
#1203 = CARTESIAN_POINT ( 'NONE',  ( 10.37757302488624767, 49.72500000273117848, 31.93888565452638417 ) ) ;
#1204 = CARTESIAN_POINT ( 'NONE',  ( -27.16883889988623935, 13.57500000273119412, 19.73931689729374739 ) ) ;
#1205 = CARTESIAN_POINT ( 'NONE',  ( -27.16883889988624290, 61.17500000273119554, -19.73931689729374028 ) ) ;
#1206 = CARTESIAN_POINT ( 'NONE',  ( 19.09188309203661049, 50.67187500000000000, -19.09188309203694445 ) ) ;
#1207 = CARTESIAN_POINT ( 'NONE',  ( 15.04653450569292872, 38.21652750092398065, -25.98046417659857710 ) ) ;
#1208 = CARTESIAN_POINT ( 'NONE',  ( 25.98046417659831775, 28.75222249907602290, -15.04653450569338879 ) ) ;
#1209 = CARTESIAN_POINT ( 'NONE',  ( -32.50000000000000000, 68.50000000546239676, 0.000000000000000000 ) ) ;
#1210 = CARTESIAN_POINT ( 'NONE',  ( -4.300734207923755825, 79.27500000273118985, 13.23629886949340673 ) ) ;
#1211 = CARTESIAN_POINT ( 'NONE',  ( 0.04044903255044120238, 57.39805583240935505, 27.95245687107223276 ) ) ;
#1212 = CYLINDRICAL_SURFACE ( 'NONE', #29644, 24.50000000000000000 ) ;
#1213 = CARTESIAN_POINT ( 'NONE',  ( -7.570916362186210335, 16.60000000000000497, -23.30088464923126779 ) ) ;
#1214 = ORIENTED_EDGE ( 'NONE', *, *, #29173, .F. ) ;
#1215 = EDGE_CURVE ( 'NONE', #11003, #16033, #29845, .T. ) ;
#1216 = CARTESIAN_POINT ( 'NONE',  ( 33.58253175000000113, 44.47500000273119269, -10.91162601494193751 ) ) ;
#1217 = CARTESIAN_POINT ( 'NONE',  ( -32.50000000000000000, 75.89999999999996305, -10.55989012756945300 ) ) ;
#1218 = CARTESIAN_POINT ( 'NONE',  ( -10.04305231718579172, 32.10000000546238397, -30.90933677959248982 ) ) ;
#1219 = VERTEX_POINT ( 'NONE', #31123 ) ;
#1220 = CARTESIAN_POINT ( 'NONE',  ( -28.01184896238304134, 32.33854166666666430, -7.505752307972844761 ) ) ;
#1221 = VERTEX_POINT ( 'NONE', #6926 ) ;
#1222 = ORIENTED_EDGE ( 'NONE', *, *, #18466, .F. ) ;
#1223 = VECTOR ( 'NONE', #14066, 1000.000000000000000 ) ;
#1224 = CARTESIAN_POINT ( 'NONE',  ( 5.147494310547434893, 26.55125428154685352, 32.49999999999999289 ) ) ;
#1225 = CARTESIAN_POINT ( 'NONE',  ( 10.37757302488624767, 49.72500000273119269, 31.93888565452638417 ) ) ;
#1226 = CARTESIAN_POINT ( 'NONE',  ( 28.01184896238290278, 54.39583333333332860, -7.505752307973347470 ) ) ;
#1227 = CARTESIAN_POINT ( 'NONE',  ( -26.29305231718578995, 8.700000005462394270, 19.10302069950538595 ) ) ;
#1228 = VECTOR ( 'NONE', #21690, 1000.000000000000114 ) ;
#1229 = CARTESIAN_POINT ( 'NONE',  ( -1.756012107511856980E-14, 4.499999999999997335, -24.50000000000000000 ) ) ;
#1230 = CARTESIAN_POINT ( 'NONE',  ( -18.94512977948576093, 18.32499999726880446, 13.76444248337722698 ) ) ;
#1231 = CARTESIAN_POINT ( 'NONE',  ( 32.50000000000000000, 51.09999999999998721, -10.55989012756945833 ) ) ;
#1232 =( BOUNDED_CURVE ( )  B_SPLINE_CURVE ( 2, ( #19854, #17980, #28430, #1483, #30308, #11957, #32875, #6807, #9374, #17286, #27749, #14711, #441 ),
 .UNSPECIFIED., .F., .T. ) 
 B_SPLINE_CURVE_WITH_KNOTS ( ( 3, 2, 2, 2, 2, 2, 3 ),
 ( 0.1388888888888888951, 0.1444444444444444309, 0.1555555555555555580, 0.1666666666666666574, 0.1777777777777777846, 0.1888888888888888840, 0.1944444444444444475 ),
 .UNSPECIFIED. ) 
 CURVE ( )  GEOMETRIC_REPRESENTATION_ITEM ( )  RATIONAL_B_SPLINE_CURVE ( ( 0.9755282581475768211, 0.9755282581475768211, 1.000000000000000000, 0.9510565162951535312, 1.000000000000000000, 0.9510565162951535312, 1.000000000000000000, 0.9510565162951535312, 1.000000000000000000, 0.9510565162951535312, 1.000000000000000000, 0.9755282581475768211, 0.9755282581475768211 ) ) 
 REPRESENTATION_ITEM ( '' )  );
#1233 = CARTESIAN_POINT ( 'NONE',  ( 33.58253175000000113, 24.47500000273118914, -10.91162601494193751 ) ) ;
#1234 = CARTESIAN_POINT ( 'NONE',  ( 0.000000000000000000, 52.00000000000000711, 32.50000000000000000 ) ) ;
#1235 = CARTESIAN_POINT ( 'NONE',  ( -19.11951029504797006, 13.99961833240935327, -19.06425588902558133 ) ) ;
#1236 = CARTESIAN_POINT ( 'NONE',  ( 13.91746824999999532, 75.97500000273119269, -4.522059556121118540 ) ) ;
#1237 = CARTESIAN_POINT ( 'NONE',  ( -26.29305231718578995, 56.20000000000001705, 19.10302069950538595 ) ) ;
#1238 = CARTESIAN_POINT ( 'NONE',  ( -32.50000000000000000, 34.00000000000000000, 0.000000000000000000 ) ) ;
#1239 = CARTESIAN_POINT ( 'NONE',  ( 20.08610463437157279, 3.299999999999997602, -27.64615127144129758 ) ) ;
#1240 = ORIENTED_EDGE ( 'NONE', *, *, #655, .T. ) ;
#1241 = CARTESIAN_POINT ( 'NONE',  ( -23.41746825000000598, 4.224999997268803931, 7.608796670333726198 ) ) ;
#1242 = CARTESIAN_POINT ( 'NONE',  ( 10.04305231718578817, 71.90000000546237402, -30.90933677959249337 ) ) ;
#1243 = CARTESIAN_POINT ( 'NONE',  ( 13.97622843553633665, 41.36197916666666430, 24.20753774853730889 ) ) ;
#1244 = CARTESIAN_POINT ( 'NONE',  ( -33.58253175000000113, 67.22500000273117848, 10.91162601494193929 ) ) ;
#1245 = CARTESIAN_POINT ( 'NONE',  ( 33.58253175000000823, 30.27500000273118630, 10.91162601494192863 ) ) ;
#1246 = CARTESIAN_POINT ( 'NONE',  ( -33.58253175000000113, 15.37500000273118950, 0.000000000000000000 ) ) ;
#1247 = CARTESIAN_POINT ( 'NONE',  ( -10.37757302488624411, 8.975000002731187365, -31.93888565452638417 ) ) ;
#1248 = CARTESIAN_POINT ( 'NONE',  ( -14.01125832528285109, 63.99777750092396644, 24.18731323226248264 ) ) ;
#1249 = CARTESIAN_POINT ( 'NONE',  ( 30.02300923189239512, 51.10156249999998579, -2.619432448724977703E-13 ) ) ;
#1250 = CARTESIAN_POINT ( 'NONE',  ( -13.91746824999999532, 80.77500000273118985, -4.522059556121115875 ) ) ;
#1251 = CARTESIAN_POINT ( 'NONE',  ( -11.25946833292375793, 79.57500000273121543, 8.180482586598737171 ) ) ;
#1252 = CARTESIAN_POINT ( 'NONE',  ( 6.277390505771533514E-15, 46.50000000000001421, 34.17252228774368916 ) ) ;
#1253 = FILL_AREA_STYLE ('',( #27360 ) ) ;
#1254 = CARTESIAN_POINT ( 'NONE',  ( 33.58253175000000823, 52.02500000273118985, 10.91162601494192685 ) ) ;
#1255 = CARTESIAN_POINT ( 'NONE',  ( -4.523095164977116484E-15, 18.62499999726881583, 24.62258325217400312 ) ) ;
#1256 = ADVANCED_FACE ( 'NONE', ( #33351, #25805 ), #9849, .F. ) ;
#1257 = ORIENTED_EDGE ( 'NONE', *, *, #27744, .T. ) ;
#1258 = CARTESIAN_POINT ( 'NONE',  ( 10.37757302488624767, 61.97500000273119269, 31.93888565452638417 ) ) ;
#1259 = DIRECTION ( 'NONE',  ( -0.000000000000000000, -1.000000000000000000, -0.000000000000000000 ) ) ;
#1260 = CARTESIAN_POINT ( 'NONE',  ( 18.94512977948575738, 8.424999997268811214, 13.76444248337723408 ) ) ;
#1261 = CARTESIAN_POINT ( 'NONE',  ( 6.950374756619721595, 32.63059000092395934, 26.09010956794232428 ) ) ;
#1262 = ADVANCED_FACE ( 'NONE', ( #28543, #2297 ), #10028, .T. ) ;
#1263 = ORIENTED_EDGE ( 'NONE', *, *, #19113, .T. ) ;
#1264 = CARTESIAN_POINT ( 'NONE',  ( 6.486482029760649416E-15, 33.62500000273119127, 35.31076352940723240 ) ) ;
#1265 = CARTESIAN_POINT ( 'NONE',  ( -32.50000000000000000, 34.60000000546236976, 10.55989012756946366 ) ) ;
#1266 = EDGE_LOOP ( 'NONE', ( #10520, #19154, #1302, #23049 ) ) ;
#1267 = CARTESIAN_POINT ( 'NONE',  ( 15.01150461594643204, 48.23697916666665719, 26.00068869287340334 ) ) ;
#1268 = CARTESIAN_POINT ( 'NONE',  ( -10.37757302488623701, 61.77500000273117564, 31.93888565452638417 ) ) ;
#1269 = CARTESIAN_POINT ( 'NONE',  ( -4.635254915624211769, 75.59999999999999432, -14.26584774442730286 ) ) ;
#1270 = CARTESIAN_POINT ( 'NONE',  ( -10.37757302488623701, 73.52500000273121827, 31.93888565452638417 ) ) ;
#1271 = CARTESIAN_POINT ( 'NONE',  ( 2.740863092043355209E-13, 31.33593749999999289, 30.02300923189239512 ) ) ;
#1272 = CARTESIAN_POINT ( 'NONE',  ( 24.50000000000000355, 6.100000000000010303, -7.960532557706203605 ) ) ;
#1273 = CARTESIAN_POINT ( 'NONE',  ( 27.16883889988624290, 2.175000002731186655, 19.73931689729373673 ) ) ;
#1274 = CARTESIAN_POINT ( 'NONE',  ( 20.75514604977248467, 14.42500000273119021, -28.56700777964554305 ) ) ;
#1275 = CARTESIAN_POINT ( 'NONE',  ( -13.91746824999999887, 70.87500000273119838, 0.000000000000000000 ) ) ;
#1276 = CARTESIAN_POINT ( 'NONE',  ( -7.468012846824272799, 43.79128499907601935, 28.02196122052058413 ) ) ;
#1277 = CARTESIAN_POINT ( 'NONE',  ( -13.91746824999999532, 71.47500000273119269, 4.522059556121122093 ) ) ;
#1278 = CARTESIAN_POINT ( 'NONE',  ( 30.02300923189239867, 61.41406250000000711, -2.619432448724978208E-13 ) ) ;
#1279 = CIRCLE ( 'NONE', #33640, 32.50000000000000000 ) ;
#1280 = CARTESIAN_POINT ( 'NONE',  ( -19.82091636218621034, 8.549999994537621717, -14.40073868116559552 ) ) ;
#1281 = CARTESIAN_POINT ( 'NONE',  ( 19.82091636218621034, 9.549999994537621717, 14.40073868116559730 ) ) ;
#1282 = CARTESIAN_POINT ( 'NONE',  ( 9.270509831248423538, 79.55000000546237970, -12.75976212528059861 ) ) ;
#1283 = CARTESIAN_POINT ( 'NONE',  ( -27.95245687107223986, 68.56993083240934084, 0.04044903255043252877 ) ) ;
#1284 = CARTESIAN_POINT ( 'NONE',  ( 10.37757302488624767, 37.72500000273118559, 31.93888565452638417 ) ) ;
#1285 = CARTESIAN_POINT ( 'NONE',  ( -8.601468415847518756, 74.57500000273120122, -11.83890561707634781 ) ) ;
#1286 = CARTESIAN_POINT ( 'NONE',  ( -20.75514604977248823, 51.07500000273116569, -28.56700777964554305 ) ) ;
#1287 = CARTESIAN_POINT ( 'NONE',  ( -27.16883889988623935, 27.57500000273119412, 19.73931689729374739 ) ) ;
#1288 = DIRECTION ( 'NONE',  ( -0.000000000000000000, -1.000000000000000000, -0.000000000000000000 ) ) ;
#1289 = CARTESIAN_POINT ( 'NONE',  ( -26.07999730980490583, 35.77604166666666430, -6.988114217767815717 ) ) ;
#1290 = CARTESIAN_POINT ( 'NONE',  ( -24.50000000000000000, 14.64999999453761603, -7.960532557706207157 ) ) ;
#1291 = CARTESIAN_POINT ( 'NONE',  ( -31.04172217648553556, 66.99999999999998579, -12.81397374188210136 ) ) ;
#1292 = CARTESIAN_POINT ( 'NONE',  ( -20.08610463437157989, 65.69999999999998863, -27.64615127144129758 ) ) ;
#1293 = CARTESIAN_POINT ( 'NONE',  ( -18.94512977948576093, 13.82499999726882756, 13.76444248337722698 ) ) ;
#1294 = CARTESIAN_POINT ( 'NONE',  ( 0.04044903255045854962, 26.46055583240935505, 30.02300923189239867 ) ) ;
#1295 = CARTESIAN_POINT ( 'NONE',  ( 23.41746825000000243, 3.024999997268812635, 7.608796670333735079 ) ) ;
#1296 = CARTESIAN_POINT ( 'NONE',  ( -7.025853678916861966, 41.78607666574268364, -26.06988505166722803 ) ) ;
#1297 = CARTESIAN_POINT ( 'NONE',  ( -2.162160676586881955E-15, 78.87500000273118417, -35.31076352940723240 ) ) ;
#1298 = CARTESIAN_POINT ( 'NONE',  ( 27.16883889988623935, 10.32500000273117635, -19.73931689729374384 ) ) ;
#1299 = CARTESIAN_POINT ( 'NONE',  ( -23.41746825000000598, 4.224999997268803931, 7.608796670333726198 ) ) ;
#1300 = CLOSED_SHELL ( 'NONE', ( #7560, #13574, #15897, #13035, #6079, #19634, #15027, #28982, #8831, #17642, #33557, #1262, #15751, #14298, #30209, #23775, #26972, #23633, #2088, #3006, #29689, #33907, #4803, #9146, #33895, #7895, #1256, #14876, #293, #28324, #14823, #26573 ) ) ;
#1301 = CARTESIAN_POINT ( 'NONE',  ( 24.20753774853731244, 54.25260416666666430, -13.97622843553632599 ) ) ;
#1302 = ORIENTED_EDGE ( 'NONE', *, *, #9021, .T. ) ;
#1303 = CARTESIAN_POINT ( 'NONE',  ( -33.58253175000000113, 53.02500000273118985, -10.91162601494193218 ) ) ;
#1304 = CARTESIAN_POINT ( 'NONE',  ( -20.75514604977248112, 25.67500000273118488, 28.56700777964554661 ) ) ;
#1305 = ORIENTED_EDGE ( 'NONE', *, *, #10511, .F. ) ;
#1306 = CARTESIAN_POINT ( 'NONE',  ( -28.01184896238290278, 21.73958333333332860, 7.505752307973363457 ) ) ;
#1307 = CARTESIAN_POINT ( 'NONE',  ( -26.02091320914849959, 26.47173583425730925, 14.97647472619947528 ) ) ;
#1308 = CARTESIAN_POINT ( 'NONE',  ( 20.08610463437157279, 39.30000000000001137, -27.64615127144129758 ) ) ;
#1309 = CARTESIAN_POINT ( 'NONE',  ( 15.14183272437241889, 19.44999999453763806, 20.84094480462498211 ) ) ;
#1310 = CARTESIAN_POINT ( 'NONE',  ( 7.236395654485755280, 4.224999997268802154, 22.27133577429736988 ) ) ;
#1311 = CARTESIAN_POINT ( 'NONE',  ( 27.16883889988624290, 22.17500000273120264, 19.73931689729373673 ) ) ;
#1312 = CARTESIAN_POINT ( 'NONE',  ( 10.04305231718578817, 25.90000000546238823, -30.90933677959249337 ) ) ;
#1313 = CARTESIAN_POINT ( 'NONE',  ( 6.277390505771533514E-15, 72.50000000000001421, 34.17252228774368916 ) ) ;
#1314 = DIRECTION ( 'NONE',  ( 0.000000000000000000, 0.000000000000000000, -1.000000000000000000 ) ) ;
#1315 = CARTESIAN_POINT ( 'NONE',  ( -3.922490400387641962, 74.00000000000000000, 13.75156615976576902 ) ) ;
#1316 = CARTESIAN_POINT ( 'NONE',  ( 25.98046417659858420, 56.26340250092398065, 15.04653450569292872 ) ) ;
#1317 = CARTESIAN_POINT ( 'NONE',  ( -33.58253175000000113, 33.47500000273119269, 10.91162601494193929 ) ) ;
#1318 = CARTESIAN_POINT ( 'NONE',  ( -20.75514604977248823, 54.82500000273118701, -28.56700777964554305 ) ) ;
#1319 = CARTESIAN_POINT ( 'NONE',  ( -15.01150461594595775, 31.62239583333333215, 26.00068869287368756 ) ) ;
#1320 =( NAMED_UNIT ( * ) SI_UNIT ( $, .STERADIAN. ) SOLID_ANGLE_UNIT ( ) );
#1321 = CARTESIAN_POINT ( 'NONE',  ( 7.236395654485760609, 9.524999997268801977, -22.27133577429736633 ) ) ;
#1322 = CARTESIAN_POINT ( 'NONE',  ( -10.04305231718579172, 15.60000000000000320, -30.90933677959248982 ) ) ;
#1323 = MECHANICAL_DESIGN_GEOMETRIC_PRESENTATION_REPRESENTATION (  '', ( #9004 ), #18345 ) ;
#1324 = CARTESIAN_POINT ( 'NONE',  ( 19.82091636218621034, 9.800000000000002487, 14.40073868116559730 ) ) ;
#1325 = EDGE_CURVE ( 'NONE', #33879, #30610, #2908, .T. ) ;
#1326 = CARTESIAN_POINT ( 'NONE',  ( -27.95245687107223986, 41.06993083240934794, 0.04044903255043252877 ) ) ;
#1327 = CARTESIAN_POINT ( 'NONE',  ( 6.486482029760649416E-15, 59.62500000273118417, 35.31076352940723240 ) ) ;
#1328 = CARTESIAN_POINT ( 'NONE',  ( 33.58253175000000113, 44.47500000273119980, -10.91162601494193574 ) ) ;
#1329 = CARTESIAN_POINT ( 'NONE',  ( 23.41746824999999887, 12.52499999726880375, 7.608796670333735079 ) ) ;
#1330 = CARTESIAN_POINT ( 'NONE',  ( 7.570916362186213000, 10.39999999999999325, -23.30088464923126423 ) ) ;
#1331 = DIRECTION ( 'NONE',  ( 0.000000000000000000, 0.000000000000000000, 1.000000000000000000 ) ) ;
#1332 = CARTESIAN_POINT ( 'NONE',  ( 24.18731323226247554, 49.38840250092398776, 14.01125832528285997 ) ) ;
#1333 =( BOUNDED_CURVE ( )  B_SPLINE_CURVE ( 2, ( #15070, #17820, #9916, #23127, #1664, #17476, #22612, #9222, #28276, #28106, #9570, #4763, #19706 ),
 .UNSPECIFIED., .F., .T. ) 
 B_SPLINE_CURVE_WITH_KNOTS ( ( 3, 2, 2, 2, 2, 2, 3 ),
 ( 0.3525641025641025883, 0.3538461538461538658, 0.3564102564102564208, 0.3589743589743589758, 0.3615384615384615308, 0.3641025641025640858, 0.3653846153846153633 ),
 .UNSPECIFIED. ) 
 CURVE ( )  GEOMETRIC_REPRESENTATION_ITEM ( )  RATIONAL_B_SPLINE_CURVE ( ( 0.9755282581475768211, 0.9755282581475772652, 1.000000000000000000, 0.9510565162951535312, 1.000000000000000000, 0.9510565162951535312, 1.000000000000000000, 0.9510565162951535312, 1.000000000000000000, 0.9510565162951535312, 1.000000000000000000, 0.9755282581475768211, 0.9755282581475768211 ) ) 
 REPRESENTATION_ITEM ( '' )  );
#1334 = CARTESIAN_POINT ( 'NONE',  ( -7.570916362186215665, 5.149999994537635573, 23.30088464923126423 ) ) ;
#1335 = DIRECTION ( 'NONE',  ( -0.8660254037844399289, -0.4999999999999977240, 0.000000000000000000 ) ) ;
#1336 = CARTESIAN_POINT ( 'NONE',  ( -33.58253175000000113, 21.02500000273117919, -10.91162601494193218 ) ) ;
#1337 = CYLINDRICAL_SURFACE ( 'NONE', #3434, 32.50000000000000000 ) ;
#1338 = CARTESIAN_POINT ( 'NONE',  ( -12.13525491562420910, 78.45000000546237118, 8.816778784387098611 ) ) ;
#1339 = CARTESIAN_POINT ( 'NONE',  ( 24.50000000000000000, 13.89999999999999680, 7.960532557706212486 ) ) ;
#1340 = CARTESIAN_POINT ( 'NONE',  ( 7.543491769121922985, 64.12982666574268364, 28.00173670424535644 ) ) ;
#1341 = CARTESIAN_POINT ( 'NONE',  ( 32.50000000000000000, 45.60000000546236265, -10.55989012756945833 ) ) ;
#1342 = CYLINDRICAL_SURFACE ( 'NONE', #21108, 15.00000000000000000 ) ;
#1343 = CARTESIAN_POINT ( 'NONE',  ( 33.58253175000000113, 34.22500000273117138, -10.91162601494193574 ) ) ;
#1344 = CARTESIAN_POINT ( 'NONE',  ( -27.95245687107222921, 21.88281249999999645, 2.498001805406602216E-13 ) ) ;
#1345 = VERTEX_POINT ( 'NONE', #20504 ) ;
#1346 = CARTESIAN_POINT ( 'NONE',  ( 33.58253175000000113, 76.22500000273119269, -10.91162601494193751 ) ) ;
#1347 = CARTESIAN_POINT ( 'NONE',  ( 2.740863092043355209E-13, 27.89843750000000000, 30.02300923189239512 ) ) ;
#1348 = VECTOR ( 'NONE', #1004, 1000.000000000000000 ) ;
#1349 = CARTESIAN_POINT ( 'NONE',  ( 4.041334437186266200E-15, -10.99999999999999645, 33.00000000000000000 ) ) ;
#1350 = ORIENTED_EDGE ( 'NONE', *, *, #9950, .T. ) ;
#1351 = CARTESIAN_POINT ( 'NONE',  ( -28.02196122052045268, 47.23996500092398065, 7.468012846824790607 ) ) ;
#1352 = CARTESIAN_POINT ( 'NONE',  ( 6.277390505771533514E-15, 13.00000000546238255, 34.17252228774368916 ) ) ;
#1353 = ADVANCED_FACE ( 'NONE', ( #14831 ), #15022, .F. ) ;
#1354 = CARTESIAN_POINT ( 'NONE',  ( 15.01150461594596308, 60.84114583333332860, -26.00068869287367335 ) ) ;
#1355 = DIRECTION ( 'NONE',  ( -1.000000000000000000, -1.309225264888156377E-16, 0.000000000000000000 ) ) ;
#1356 = CARTESIAN_POINT ( 'NONE',  ( 20.75514604977249178, 44.07500000273117990, 28.56700777964553950 ) ) ;
#1357 = CARTESIAN_POINT ( 'NONE',  ( 26.29305231718579350, 53.30000000546236549, 19.10302069950537529 ) ) ;
#1358 = CARTESIAN_POINT ( 'NONE',  ( -8.960552108402742093E-16, 74.87500000273119838, -14.63369212191046387 ) ) ;
#1359 = CARTESIAN_POINT ( 'NONE',  ( 6.486482029760649416E-15, 29.62500000273120193, 35.31076352940723240 ) ) ;
#1360 = CARTESIAN_POINT ( 'NONE',  ( 10.04305231718579705, 77.10000000546237686, 30.90933677959248982 ) ) ;
#1361 = CARTESIAN_POINT ( 'NONE',  ( -2.162160676586881955E-15, 58.87500000273117706, -35.31076352940723240 ) ) ;
#1362 =( NAMED_UNIT ( * ) SI_UNIT ( $, .STERADIAN. ) SOLID_ANGLE_UNIT ( ) );
#1363 = EDGE_CURVE ( 'NONE', #32007, #6723, #33631, .T. ) ;
#1364 = CARTESIAN_POINT ( 'NONE',  ( -32.50000000000000000, 34.10000000000000142, 10.55989012756946366 ) ) ;
#1365 = CARTESIAN_POINT ( 'NONE',  ( 20.08610463437157279, 31.30000000000000071, -27.64615127144129758 ) ) ;
#1366 = CARTESIAN_POINT ( 'NONE',  ( 23.41746825000000243, 10.72499999726880127, -7.608796670333727974 ) ) ;
#1367 = CARTESIAN_POINT ( 'NONE',  ( -27.16883889988623935, 73.32500000273117280, 19.73931689729374739 ) ) ;
#1368 = AXIS2_PLACEMENT_3D ( 'NONE', #32981, #17395, #27514 ) ;
#1369 = FACE_OUTER_BOUND ( 'NONE', #17714, .T. ) ;
#1370 = CARTESIAN_POINT ( 'NONE',  ( -4.300734207923759378, 80.97500000273122112, -13.23629886949340495 ) ) ;
#1371 = CARTESIAN_POINT ( 'NONE',  ( 10.37757302488624767, 63.97500000273120691, 31.93888565452638417 ) ) ;
#1372 = CARTESIAN_POINT ( 'NONE',  ( -4.635254915624211769, 77.85000000546237686, -14.26584774442730286 ) ) ;
#1373 = EDGE_CURVE ( 'NONE', #11531, #13996, #14522, .T. ) ;
#1374 = DIRECTION ( 'NONE',  ( 0.000000000000000000, -1.000000000000000000, 0.000000000000000000 ) ) ;
#1375 = CARTESIAN_POINT ( 'NONE',  ( -19.82091636218621389, 2.949999994537627401, 14.40073868116558842 ) ) ;
#1376 = AXIS2_PLACEMENT_3D ( 'NONE', #6186, #27460, #21818 ) ;
#1377 = CARTESIAN_POINT ( 'NONE',  ( 19.11951029504763611, 14.29725666759064318, -19.06425588902591173 ) ) ;
#1378 = CARTESIAN_POINT ( 'NONE',  ( 3.000384657911015469E-15, 16.99999999999998579, 24.50000000000000000 ) ) ;
#1379 = CARTESIAN_POINT ( 'NONE',  ( -20.75514604977248112, 49.42500000273118133, 28.56700777964554661 ) ) ;
#1380 = CARTESIAN_POINT ( 'NONE',  ( -33.58253175000000113, 1.375000002731191495, 0.000000000000000000 ) ) ;
#1381 = CARTESIAN_POINT ( 'NONE',  ( 27.16883889988623935, 56.57500000273117990, -19.73931689729374384 ) ) ;
#1382 = CARTESIAN_POINT ( 'NONE',  ( 2.584737979205442066E-13, 51.96093750000000000, 27.95245687107223276 ) ) ;
#1383 = CARTESIAN_POINT ( 'NONE',  ( -30.02300923189239867, 37.07069416759063785, -0.04044903254991731589 ) ) ;
#1384 = ADVANCED_FACE ( 'NONE', ( #23749 ), #5887, .F. ) ;
#1385 = CARTESIAN_POINT ( 'NONE',  ( 7.468012846824281681, 28.32253499907601579, -28.02196122052058058 ) ) ;
#1386 = CARTESIAN_POINT ( 'NONE',  ( 20.08610463437157279, 69.80000000546240813, -27.64615127144129758 ) ) ;
#1387 = CARTESIAN_POINT ( 'NONE',  ( 8.601468415847520532, 71.57500000273118701, 11.83890561707634781 ) ) ;
#1388 = VECTOR ( 'NONE', #20093, 999.9999999999998863 ) ;
#1389 = CARTESIAN_POINT ( 'NONE',  ( -24.22776226481266448, 51.66888916574269075, -13.94119854578892514 ) ) ;
#1390 = AXIS2_PLACEMENT_3D ( 'NONE', #28452, #10100, #31024 ) ;
#1391 = CARTESIAN_POINT ( 'NONE',  ( -32.50000000000000000, 57.89999999999999858, -10.55989012756945300 ) ) ;
#1392 = CARTESIAN_POINT ( 'NONE',  ( -3.880418787951127602, 4.301254276084477191, -24.50000000000000000 ) ) ;
#1393 = VERTEX_POINT ( 'NONE', #7954 ) ;
#1394 = CARTESIAN_POINT ( 'NONE',  ( -10.37757302488623701, 43.77500000273119696, 31.93888565452638417 ) ) ;
#1395 = CARTESIAN_POINT ( 'NONE',  ( -5.147494310547423346, 76.44874571845313938, 32.50000000000000000 ) ) ;
#1396 = CARTESIAN_POINT ( 'NONE',  ( -32.50000000000000000, 32.60000000546237686, 10.55989012756946366 ) ) ;
#1397 = EDGE_LOOP ( 'NONE', ( #10454, #24913, #25682, #18863, #18814, #27071, #26820, #24496 ) ) ;
#1398 = CARTESIAN_POINT ( 'NONE',  ( -20.50609665440969209, 38.64062500000000000, 20.50609665441005092 ) ) ;
#1399 = ORIENTED_EDGE ( 'NONE', *, *, #21754, .T. ) ;
#1400 = CARTESIAN_POINT ( 'NONE',  ( -24.50000000000000711, 12.84999999453761532, 7.960532557706201828 ) ) ;
#1401 = CARTESIAN_POINT ( 'NONE',  ( 33.58253175000000113, 46.12500000273117706, -4.112674001490185761E-15 ) ) ;
#1402 = CARTESIAN_POINT ( 'NONE',  ( 20.50609665440969565, 57.54687500000000000, -20.50609665441004736 ) ) ;
#1403 = CARTESIAN_POINT ( 'NONE',  ( 20.08610463437157279, 13.80000000546235839, -27.64615127144129758 ) ) ;
#1404 = CARTESIAN_POINT ( 'NONE',  ( 20.75514604977248467, 66.42500000273119554, -28.56700777964554305 ) ) ;
#1405 = CARTESIAN_POINT ( 'NONE',  ( -18.94512977948575738, 15.92499999726881832, -13.76444248337723231 ) ) ;
#1406 = CARTESIAN_POINT ( 'NONE',  ( 10.04305231718579705, 54.59999999999998010, 30.90933677959248982 ) ) ;
#1407 = CARTESIAN_POINT ( 'NONE',  ( -8.891200544363830713E-16, 71.75000000546238255, -15.00000000000000000 ) ) ;
#1408 = CARTESIAN_POINT ( 'NONE',  ( 6.486482029760649416E-15, 15.87500000273120015, 35.31076352940723240 ) ) ;
#1409 = SURFACE_SIDE_STYLE ('',( #16544 ) ) ;
#1410 = CARTESIAN_POINT ( 'NONE',  ( 24.18731323226221974, 18.43972249907602290, -14.01125832528328985 ) ) ;
#1411 = CARTESIAN_POINT ( 'NONE',  ( 8.601468415847520532, 77.57500000273118701, 11.83890561707634781 ) ) ;
#1412 = CARTESIAN_POINT ( 'NONE',  ( -20.08610463437156923, 56.29999999999999716, 27.64615127144130113 ) ) ;
#1413 = CARTESIAN_POINT ( 'NONE',  ( 5.779280353836490358E-15, 34.49999999999998579, 32.49999999999999289 ) ) ;
#1414 = CARTESIAN_POINT ( 'NONE',  ( 32.50000000000000000, 5.099999999999998757, -10.55989012756945833 ) ) ;
#1415 = ORIENTED_EDGE ( 'NONE', *, *, #27172, .T. ) ;
#1416 = CARTESIAN_POINT ( 'NONE',  ( 23.41746825000000243, 9.024999997268826846, 7.608796670333735079 ) ) ;
#1417 = CARTESIAN_POINT ( 'NONE',  ( 32.50000000000000711, 71.40000000546240244, 10.55989012756945122 ) ) ;
#1418 = CARTESIAN_POINT ( 'NONE',  ( 19.09188309203661049, 43.79687500000000000, -19.09188309203694445 ) ) ;
#1419 = CARTESIAN_POINT ( 'NONE',  ( -20.75514604977248112, 69.42500000273116711, 28.56700777964554661 ) ) ;
#1420 = CARTESIAN_POINT ( 'NONE',  ( -20.75514604977248823, 23.07500000273117635, -28.56700777964554305 ) ) ;
#1421 = CARTESIAN_POINT ( 'NONE',  ( 33.58253175000000113, 16.47500000273118204, -10.91162601494193751 ) ) ;
#1422 = CARTESIAN_POINT ( 'NONE',  ( -10.37757302488624411, 10.97500000273118914, -31.93888565452638417 ) ) ;
#1423 = CARTESIAN_POINT ( 'NONE',  ( -20.47846945139902175, 13.43788166759064140, -20.53372385742072481 ) ) ;
#1424 = CARTESIAN_POINT ( 'NONE',  ( 26.00068869287340334, 57.69010416666667140, -15.01150461594642316 ) ) ;
#1425 = CARTESIAN_POINT ( 'NONE',  ( 8.601468415847520532, 80.07500000273118701, 11.83890561707634603 ) ) ;
#1426 = CARTESIAN_POINT ( 'NONE',  ( -2.092463501923844636E-15, 45.49999999999998579, -34.17252228774368916 ) ) ;
#1427 = CARTESIAN_POINT ( 'NONE',  ( 7.570916362186207671, 7.349999994537615322, 23.30088464923126779 ) ) ;
#1428 = CARTESIAN_POINT ( 'NONE',  ( -27.16883889988624290, 50.92500000273120264, -19.73931689729374028 ) ) ;
#1429 = CARTESIAN_POINT ( 'NONE',  ( 23.41746825000000243, 4.724999997268818142, -7.608796670333727974 ) ) ;
#1430 = ORIENTED_EDGE ( 'NONE', *, *, #8739, .T. ) ;
#1431 = CARTESIAN_POINT ( 'NONE',  ( -33.58253175000000113, 61.27500000273118985, -10.91162601494193218 ) ) ;
#1432 = CARTESIAN_POINT ( 'NONE',  ( 23.41746824999999887, 14.62499999726882294, 0.000000000000000000 ) ) ;
#1433 = CARTESIAN_POINT ( 'NONE',  ( 26.06988505166735592, 28.62017333425730925, 7.025853678916393896 ) ) ;
#1434 =( BOUNDED_CURVE ( )  B_SPLINE_CURVE ( 2, ( #18708, #3410, #13883, #11465, #16132, #13552, #24015, #31887, #821, #22110, #30143, #14548, #25007 ),
 .UNSPECIFIED., .F., .T. ) 
 B_SPLINE_CURVE_WITH_KNOTS ( ( 3, 2, 2, 2, 2, 2, 3 ),
 ( 0.5705128205128204844, 0.5717948717948717618, 0.5743589743589743168, 0.5769230769230768718, 0.5794871794871795379, 0.5820512820512820928, 0.5833333333333333703 ),
 .UNSPECIFIED. ) 
 CURVE ( )  GEOMETRIC_REPRESENTATION_ITEM ( )  RATIONAL_B_SPLINE_CURVE ( ( 0.9755282581475768211, 0.9755282581475768211, 1.000000000000000000, 0.9510565162951535312, 1.000000000000000000, 0.9510565162951535312, 1.000000000000000000, 0.9510565162951535312, 1.000000000000000000, 0.9510565162951535312, 1.000000000000000000, 0.9755282581475768211, 0.9755282581475768211 ) ) 
 REPRESENTATION_ITEM ( '' )  );
#1435 = ORIENTED_EDGE ( 'NONE', *, *, #13848, .T. ) ;
#1436 = CARTESIAN_POINT ( 'NONE',  ( 27.16883889988624290, 29.92500000273119909, 19.73931689729373673 ) ) ;
#1438 = CARTESIAN_POINT ( 'NONE',  ( 7.570916362186207671, 5.599999999999994316, 23.30088464923126779 ) ) ;
#1437 = AXIS2_PLACEMENT_3D ( 'NONE', #30037, #32278, #3798 ) ;
#1439 = ORIENTED_EDGE ( 'NONE', *, *, #19442, .T. ) ;
#1441 = CARTESIAN_POINT ( 'NONE',  ( 20.50609665441005092, 61.84374999999998579, 20.50609665440969209 ) ) ;
#1440 =( BOUNDED_SURFACE ( )  B_SPLINE_SURFACE ( 1, 2, ( 
 ( #26586, #29145, #13713, #31724, #10968, #2737, #24179, #10632, #31886, #18707, #18867, #16458, #29315, #29477, #26416, #26249, #21443, #21110, #8215, #5818, #31554, #3082, #3409, #5481, #26911, #13200, #16294, #21609, #23677, #5981, #32054, #2910, #8554, #19038, #13882, #24348, #13378, #820, #21282, #11301, #5649, #21779, #16131, #7879, #18369, #21938, #9213, #32717, #11796, #17127, #22274, #3907, #29812, #14213, #19198, #16791, #19532, #19697, #27249, #11625, #6315, #16958, #980, #22433, #27080, #32388, #6486, #6812, #27583, #27417, #24669, #16625, #3574, #11464, #30315, #1313, #30142, #14716, #6646, #14547, #8883, #4072, #6140, #3742, #14376, #1488, #25006, #19369, #1143, #29637, #24835, #22109, #32553, #11962, #32880, #24507, #9379, #25176, #19861, #17293, #8715, #14046, #27754, #9052, #29981, #4242, #1654, #12129, #32226, #17467, #33582, #18156, #4584, #7325, #27927, #7670, #33408, #23297, #17635, #20215, #25861, #20382, #30483, #25528, #2528, #22601, #28267, #28096, #22950, #4411, #33055, #10256, #20038, #7503, #2351, #9905, #14888, #9560, #20737, #6984, #17987, #12825, #25349, #12647, #30833, #23118, #31179, #10082, #28598, #7152, #1828, #15230, #12306, #12481, #20561, #22778, #17809, #5098, #33230, #15583, #9729, #4753, #28435, #30655, #26034, #4925, #15061, #15405, #2174, #25693, #33764, #2005, #31006, #15920, #6401, #7839, #16875, #13160, #5439, #26206, #2700, #23975, #13512, #26544, #31848, #3040, #18666, #10592, #28941, #33929, #31518, #274, #446, #8012, #26376, #21069, #31682, #15752, #3658, #18328, #23636, #21239, #22025, #8341, #8176, #2867, #31346, #28773, #102, #11543, #16093, #10928, #29898, #21403, #29276, #18497, #18831, #20897, #13336, #29104, #16711, #6231, #23809, #10761, #10420, #5609, #27165, #14134, #24590, #1062, #5270, #32469, #27338, #8970, #19453, #23467, #12996, #1742, #11884, #14297, #14804, #30062, #24755, #22519, #32640, #25269, #33326, #19780, #32970, #9135, #22868, #14635, #4500, #32802, #1406, #7072, #1572, #11710, #6731, #17728, #3824, #9474, #9295, #28013, #19617, #3993, #12049, #12397, #33146, #19955, #30229, #22194, #6568, #17042, #1921, #6902, #17383, #20300, #27848, #20131, #14465, #22695, #27502, #22355, #30403, #17556, #4331, #24921, #17214, #1231, #12222, #27673, #4162, #9651, #30576, #25095, #14976, #30750, #25445, #9823, #7239, #33499, #26123, #2270, #4673, #5191, #20475, #15152, #12912, #23041, #15675, #23723, #10175, #23388, #10002, #13250, #5015, #28861, #23216, #25782, #31437, #25953, #2097, #31097, #8098, #28185, #33850, #33676, #28520, #30926, #25616, #15838, #12570, #13083, #7929, #7419, #18246, #15497, #28693, #2784, #2620, #26295, #12743, #17905, #20821, #28358, #18071, #23557, #4844, #10345, #190, #15326, #10677, #20657, #31265, #21, #7594, #21158, #10509, #2446, #20987, #7760, #18416, #5358, #31600, #11182, #21487, #11504, #13425, #21984, #18751, #11017, #31766, #8259, #29519, #19079, #32098, #3452, #8595, #24226, #16176, #530, #5528, #3126, #5862, #6022, #13598, #31934, #26632, #3290, #21325, #16669, #21653, #16500, #1022, #26953, #862, #29193, #13924, #26463, #24064, #696, #21819, #24388, #5699, #8427, #16008, #11343, #18916, #29361, #32267, #8760, #10850, #19243, #32432, #26796, #29682, #29025, #23893, #6187, #16340, #2955, #27126, #13755, #364, #3620, #14094, #24550, #18585, #24882, #27634, #14257, #27975, #19744, #9609, #3952, #6532, #12182, #6692, #16839, #11842, #22825, #8930, #14597, #14427, #9260, #3787, #19411, #30535, #6360, #27805, #22652, #11673, #32929, #30190, #9428, #17514, #30362, #7031, #27462, #27295, #1535, #22156, #32766, #6863, #32598, #4122, #4460, #9098, #14936, #24715, #25054, #14764, #1192, #25401, #25229, #19579, #4289, #22480, #12011, #33104, #30027, #19913, #22321, #1879, #17005, #12356, #1365, #17176, #17342, #1703, #20090, #29860, #12872, #18206, #23349, #4977, #30882, #15281, #20262, #17862, #20614, #20782, #28313, #12700, #7378, #18035, #2055, #23515, #28146, #33457, #7551, #7886, #28649, #28481, #25741, #17686, #4632, #12531, #15455, #15111, #5145, #2223, #15632, #25575, #9956, #4801, #25910, #2404, #30707, #7202, #33285, #18375, #33811, #20947, #10468, #31396, #2580, #7719, #28820, #20432, #13044, #33975, #23000, #5318, #10304, #23171, #26084, #31226, #15798, #33633, #26254, #2742, #13206, #10132, #9782, #31058, #21116, #26917, #10637, #24021, #321, #3414, #29149, #28988, #5487, #18713, #2916, #16301, #26758, #825, #13888, #13383, #32060, #5655, #31728, #29643, #3250, #8560, #13720, #21448, #31891, #16137, #24354, #8057, #491, #3581, #31559, #10808, #21288, #18872, #27087, #8387, #26591, #21615, #10974, #23682, #8219, #18542, #3087, #15966, #19044, #13559, #26422, #23855, #11306, #29321, #5823, #21784, #29482, #24184, #657, #11145, #5986, #16463, #32232, #8722, #19206, #6146, #148, #16631, #19705, #30151, #12138, #24844, #4081, #17302, #6655, #16800, #20047, #16966, #22611, #14222, #27764, #11972, #29819, #33064, #14725, #9569, #30492, #29989, #17138, #17475, #32728, #1322, #32888, #3915, #22283, #6993, #9387, #9221, #6493, #32394, #8889, #27257, #27936, #27591, #14555, #14053, #25016, #30324, #24678, #19871, #21944, #22117, #1496, #4250, #22442, #1152, #27424, #985, #6820, #11634, #14387, #25186, #1663, #6324, #24515, #11470, #19374, #3748, #32561, #9060, #19541, #11805, #14895, #15415, #30664, #25359, #23126, #33240, #25870, #33938, #20391, #33591, #9738, #23476, #15239, #5107, #33417, #2015, #7679, #2183, #12316, #7334, #18336, #4420, #10092, #9915, #4762, #20224, #1837, #26043, #22787, #23307, #18165, #7161, #28442, #25702, #4933, #13005, #2360, #2538, #22959, #17644, #31014, #28105, #28275, #12833, #4592, #20570, #10430, #15068, #20905, #25536, #7512, #10264, #12490, #31356, #20746, #30843, #33773, #17996, #31189, #28607, #17818, #15591, #12657, #7848, #26215, #21412, #109, #18505, #23647, #10600, #21248, #31691, #283, #18675, #10771, #13345, #21078, #8020, #5278, #31526, #26385, #8185, #28951, #5448, #15929, #2877, #13169, #16102, #2708, #23817, #29114, #5618, #13520, #26553, #3048, #23984 ),
 ( #455, #28781, #10936, #15762, #10371, #15357, #7621, #20331, #20849, #7452, #31295, #30781, #25647, #23070, #31129, #18101, #12430, #22899, #25477, #10539, #28549, #13112, #2649, #23586, #28723, #33878, #51, #2125, #5218, #15701, #7274, #21016, #5046, #4876, #7787, #20688, #33709, #12600, #18276, #26155, #31467, #25811, #7959, #18446, #33357, #28889, #9854, #2302, #33531, #5389, #30955, #17757, #28215, #20509, #4702, #15530, #25983, #1956, #15183, #10034, #17937, #28387, #12774, #23248, #2476, #10207, #12943, #23416, #13628, #8288, #16531, #219, #26660, #29713, #13279, #2987, #26492, #11050, #19272, #24092, #18778, #13787, #3156, #15867, #13456, #10706, #29222, #21187, #11211, #5728, #31629, #2812, #26982, #16206, #8127, #13952, #24255, #18615, #560, #31964, #23924, #29053, #21515, #5558, #21684, #8458, #16037, #23754, #3481, #18947, #394, #24415, #725, #10879, #29392, #5892, #16370, #26824, #892, #3320, #32131, #8626, #26324, #21849, #19109, #29547, #11373, #6048, #32294, #8788, #21354, #31796, #23146, #20069, #10111, #6842, #33437, #2036, #11990, #17157, #4101, #1515, #9408, #12159, #1860, #19891, #33264, #9758, #22978, #30513, #20243, #17321, #27784, #22633, #4270, #14744, #30684, #7182, #4199, #27204, #32506, #1442, #9330, #8837, #32673, #9511, #24789, #19816, #27033, #21893, #14501, #24625, #3528, #27539, #19320, #14000, #1268, #11418, #4026, #12085, #9007, #11748, #32343, #1607, #27373, #17249, #11581, #14168, #30268, #14333, #24462, #19487, #30915, #16578, #22227, #22062, #16911, #29762, #938, #14670, #6269, #11919, #6768, #16746, #6602, #3861, #17079, #25130, #24958, #22553, #1098, #3695, #9169, #29936, #6440, #22390, #19653, #30095, #33006, #32839, #20464, #27709, #13073, #13239, #23204, #5518, #23713, #18405, #7920, #20977, #26285, #31427, #23548, #5005, #23378, #28348, #25942, #28683, #28850, #2436, #20812, #15488, #26113, #10163, #31590, #2259, #7585, #15664, #15998, #2775, #2611, #33840, #25773, #12733, #20646, #26454, #10499, #5349, #23884, #15830, #179, #18063, #10669, #15314, #12903, #10, #21148, #8089, #4834, #18576, #29017, #2945, #28508, #10336, #13416, #355, #33666, #10839, #21316, #7409, #17895, #31088, #31256, #7748, #18237, #5181, #8753, #24053, #8249, #16491, #26622, #19237, #27287, #13747, #26946, #3118, #16832, #8588, #32424, #26788, #29353, #1014, #29512, #5689, #689, #11665, #31758, #3446, #3280, #32092, #13589, #18741, #19404, #29184, #16662, #11497, #521, #21812, #19072, #32260, #6353, #29675, #29852, #16332, #16167, #24383, #11008, #21646, #6180, #21478, #13916, #3779, #31925, #14250, #8417, #856, #3612, #18906, #24707, #14085, #5853, #27119, #11336, #24543, #21976, #24218, #8921, #11175, #1184, #6016, #25568, #22313, #14587, #1356, #11835, #14928, #14420, #4282, #15103, #30354, #25394, #32591, #27454, #20083, #30181, #9090, #33098, #24873, #19572, #6856, #16996, #9601, #17676, #4113, #17334, #3945, #7194, #32921, #22818, #17169, #19737, #1871, #19905, #30020, #25047, #2048, #22147, #27798, #27626, #22473, #32758, #6524, #9772, #9252, #7024, #12349, #6685, #12173, #9420, #22645, #30698, #30526, #20255, #1528, #12002, #14756, #25219, #1697, #17506, #27968, #4450, #28138, #33277, #4624, #20424, #18197, #18366, #28306, #10630, #28811, #4794, #7877, #26074, #31217, #26247, #23161, #5136, #15446, #5479, #7368, #15958, #12692, #4968, #25734, #2213, #23508, #13037, #2569, #31387, #33966, #28640, #10123, #28473, #33450, #31050, #33803, #10460, #7542, #25901, #20604, #7710, #15273, #2735, #17853, #33624, #20773, #21107, #5308, #15622, #2394, #30873, #18027, #12863, #31551, #20938, #15790, #28980, #13198, #23675, #23340, #139, #10296, #8049, #18534, #26414, #12523, #9948, #22991, #16456, #24504, #13549, #18865, #21777, #11138, #978, #29474, #11298, #5815, #16789, #8881, #8551, #19036, #11462, #13711, #26908, #6138, #5979, #5647, #19367, #16292, #21936, #3079, #16623, #817, #18705, #32386, #3572, #29810, #6311, #29312, #3407, #2907, #21607, #24177, #32224, #26749, #13879, #31721, #8713, #3243, #19196, #8212, #24011, #648, #29143, #32050, #23847, #312, #13376, #10800, #24346, #21279, #14043, #16129, #27077, #29635, #26583, #483, #10966, #21440, #31884, #8380, #19858, #6644, #22599, #22431, #1486, #3905, #12127, #30481, #33053, #17124, #6982, #9558, #24667, #17465, #14211, #27581, #14374, #27925, #32714, #32551, #9050, #22272, #6484, #30313, #6810, #4408, #14885, #16956, #1652, #9211, #1311, #33228, #17289, #20035, #27752, #25004, #11960, #19694, #25346, #11623, #4070, #7150, #1141, #24833, #11793, #32878, #30653, #9377, #30140, #25173, #14545, #27247, #4240, #22106, #14714, #19529, #1826, #12304, #29979, #27415, #22776, #9727, #20213, #3740, #15582, #22948, #17985, #33762, #31177, #2526, #10419, #9903, #10254, #10590, #25859, #20896, #28093, #33406, #26033, #25691, #4582, #28596, #20380, #15059, #2348, #12478, #5095, #13159, #33579, #12823, #30829, #2699, #28433, #18327, #12645, #15228, #31345, #15403, #25526, #20559, #31517, #17632, #23294, #23116, #4923, #7323, #2003, #5268, #17807, #12995, #7837, #28265, #7667, #20735, #18154, #26205, #23466, #15750, #2172, #4751, #33928, #10078, #7501, #28772, #31004, #23635, #101, #21068, #16583, #15919, #13677, #13840, #23808, #6102, #24307, #273, #3370, #21569, #26713, #21739, #18665, #608, #10927, #943, #2865, #11423, #8174, #444, #21238, #31681, #18997, #8510, #32014, #26875, #29441, #24141, #5608, #23974, #28939, #26543, #29275, #5943, #3038, #21401, #16092, #3209, #10760, #32184, #13334, #29103, #16256, #27038, #781, #11100, #31847, #26375, #13511, #8340, #3533, #16423, #11263, #24468, #8679, #19162, #18830, #29600, #5776, #14005, #21898, #8011, #18496, #5438, #4203, #11925, #19997, #9012, #14338, #17254, #12090, #1103, #22395, #9174, #32844, #6943, #19821, #30445, #16917, #16751, #24965, #11587, #22234, #30273, #22067, #27544, #27887, #32511, #17426, #6274, #4031, #14675, #14173, #4370, #25135, #24630, #27715, #9336, #17084, #22559, #19492, #1447, #1273, #25311, #27209, #1784, #29941, #24794, #6445, #27377, #6773 ) ),
 .UNSPECIFIED., .F., .F., .T. ) 
 B_SPLINE_SURFACE_WITH_KNOTS ( ( 2, 2 ),
 ( 3, 2, 2, 2, 2, 2, 2, 2, 2, 2, 2, 2, 2, 2, 2, 2, 2, 2, 2, 2, 2, 2, 2, 2, 2, 2, 2, 2, 2, 2, 2, 2, 2, 2, 2, 2, 2, 2, 2, 2, 2, 2, 2, 2, 2, 2, 2, 2, 2, 2, 2, 2, 2, 2, 2, 2, 2, 2, 2, 2, 2, 2, 2, 2, 2, 2, 2, 2, 2, 2, 2, 2, 2, 2, 2, 2, 2, 2, 2, 2, 2, 2, 2, 2, 2, 2, 2, 2, 2, 2, 2, 2, 2, 2, 2, 2, 2, 2, 2, 2, 2, 2, 2, 2, 2, 2, 2, 2, 2, 2, 2, 2, 2, 2, 2, 2, 2, 2, 2, 2, 2, 2, 2, 2, 2, 2, 2, 2, 2, 2, 2, 2, 2, 2, 2, 2, 2, 2, 2, 2, 2, 2, 2, 2, 2, 2, 2, 2, 2, 2, 2, 2, 2, 2, 2, 2, 2, 2, 2, 2, 2, 2, 2, 2, 2, 2, 2, 2, 2, 2, 2, 2, 2, 2, 2, 2, 2, 2, 2, 2, 2, 2, 2, 2, 2, 2, 2, 2, 2, 2, 2, 2, 2, 2, 2, 2, 2, 2, 2, 2, 2, 2, 2, 2, 2, 2, 2, 2, 2, 2, 2, 2, 2, 2, 2, 2, 2, 2, 2, 2, 2, 2, 2, 2, 2, 2, 2, 2, 2, 2, 2, 2, 2, 2, 2, 2, 2, 2, 2, 2, 2, 2, 2, 2, 2, 2, 2, 2, 2, 2, 2, 2, 2, 2, 2, 2, 2, 2, 2, 2, 2, 2, 2, 2, 2, 2, 2, 2, 2, 2, 2, 2, 2, 2, 2, 2, 2, 2, 2, 2, 2, 2, 2, 2, 2, 2, 2, 2, 2, 2, 2, 2, 2, 2, 2, 2, 2, 2, 2, 2, 2, 2, 2, 2, 2, 2, 2, 2, 2, 2, 2, 2, 2, 2, 2, 2, 2, 2, 2, 2, 2, 2, 2, 2, 2, 2, 2, 2, 2, 2, 2, 2, 2, 2, 2, 2, 2, 2, 2, 2, 2, 2, 2, 2, 2, 2, 2, 2, 2, 2, 2, 2, 2, 2, 2, 2, 2, 2, 2, 2, 2, 2, 2, 2, 2, 2, 2, 2, 2, 2, 2, 2, 2, 2, 2, 2, 2, 2, 2, 2, 2, 2, 2, 2, 2, 2, 2, 2, 2, 2, 3 ),
 ( 0.000000000000000000, 1.000000000000000000 ),
 ( 0.000000000000000000, 0.002564102564102564100, 0.005128205128205128201, 0.007692307692307692735, 0.01025641025641025640, 0.01282051282051282007, 0.01538461538461538547, 0.01794871794871794740, 0.02051282051282051280, 0.02307692307692307820, 0.02564102564102564014, 0.02820512820512820554, 0.03076923076923077094, 0.03333333333333333287, 0.03589743589743589480, 0.03846153846153846367, 0.04102564102564102561, 0.04358974358974358754, 0.04615384615384615641, 0.04871794871794871834, 0.05128205128205128027, 0.05384615384615384914, 0.05641025641025641107, 0.05897435897435897301, 0.06153846153846154188, 0.06410256410256409687, 0.06666666666666666574, 0.06923076923076923461, 0.07179487179487178961, 0.07435897435897435848, 0.07692307692307692735, 0.07948717948717948234, 0.08205128205128205121, 0.08461538461538462008, 0.08717948717948717507, 0.08974358974358974395, 0.09230769230769231282, 0.09487179487179486781, 0.09743589743589743668, 0.1000000000000000056, 0.1025641025641025605, 0.1051282051282051294, 0.1076923076923076983, 0.1102564102564102533, 0.1128205128205128221, 0.1153846153846153910, 0.1179487179487179460, 0.1205128205128205149, 0.1230769230769230838, 0.1256410256410256387, 0.1282051282051281937, 0.1307692307692307765, 0.1333333333333333315, 0.1358974358974358865, 0.1384615384615384692, 0.1410256410256410242, 0.1435897435897435792, 0.1461538461538461620, 0.1487179487179487170, 0.1512820512820512719, 0.1538461538461538547, 0.1564102564102564097, 0.1589743589743589647, 0.1615384615384615474, 0.1641025641025641024, 0.1666666666666666574, 0.1692307692307692402, 0.1717948717948717952, 0.1743589743589743501, 0.1769230769230769329, 0.1794871794871794879, 0.1820512820512820429, 0.1846153846153846256, 0.1871794871794871806, 0.1897435897435897356, 0.1923076923076923184, 0.1948717948717948734, 0.1974358974358974284, 0.2000000000000000111, 0.2025641025641025661, 0.2051282051282051211, 0.2076923076923077038, 0.2102564102564102588, 0.2128205128205128138, 0.2153846153846153966, 0.2179487179487179516, 0.2205128205128205066, 0.2230769230769230893, 0.2256410256410256443, 0.2282051282051281993, 0.2307692307692307820, 0.2333333333333333370, 0.2358974358974358920, 0.2384615384615384748, 0.2410256410256410298, 0.2435897435897435848, 0.2461538461538461675, 0.2487179487179487225, 0.2512820512820512775, 0.2538461538461538325, 0.2564102564102563875, 0.2589743589743589980, 0.2615384615384615530, 0.2641025641025641080, 0.2666666666666666630, 0.2692307692307692180, 0.2717948717948717730, 0.2743589743589743835, 0.2769230769230769384, 0.2794871794871794934, 0.2820512820512820484, 0.2846153846153846034, 0.2871794871794871584, 0.2897435897435897689, 0.2923076923076923239, 0.2948717948717948789, 0.2974358974358974339, 0.2999999999999999889, 0.3025641025641025439, 0.3051282051282051544, 0.3076923076923077094, 0.3102564102564102644, 0.3128205128205128194, 0.3153846153846153744, 0.3179487179487179294, 0.3205128205128205399, 0.3230769230769230949, 0.3256410256410256499, 0.3282051282051282048, 0.3307692307692307598, 0.3333333333333333148, 0.3358974358974358698, 0.3384615384615384803, 0.3410256410256410353, 0.3435897435897435903, 0.3461538461538461453, 0.3487179487179487003, 0.3512820512820512553, 0.3538461538461538658, 0.3564102564102564208, 0.3589743589743589758, 0.3615384615384615308, 0.3641025641025640858, 0.3666666666666666408, 0.3692307692307692513, 0.3717948717948718063, 0.3743589743589743613, 0.3769230769230769162, 0.3794871794871794712, 0.3820512820512820262, 0.3846153846153846367, 0.3871794871794871917, 0.3897435897435897467, 0.3923076923076923017, 0.3948717948717948567, 0.3974358974358974117, 0.4000000000000000222, 0.4025641025641025772, 0.4051282051282051322, 0.4076923076923076872, 0.4102564102564102422, 0.4128205128205127972, 0.4153846153846154077, 0.4179487179487179627, 0.4205128205128205177, 0.4230769230769230727, 0.4256410256410256276, 0.4282051282051281826, 0.4307692307692307931, 0.4333333333333333481, 0.4358974358974359031, 0.4384615384615384581, 0.4410256410256410131, 0.4435897435897435681, 0.4461538461538461786, 0.4487179487179487336, 0.4512820512820512886, 0.4538461538461538436, 0.4564102564102563986, 0.4589743589743589536, 0.4615384615384615641, 0.4641025641025641191, 0.4666666666666666741, 0.4692307692307692291, 0.4717948717948717841, 0.4743589743589743390, 0.4769230769230769496, 0.4794871794871795045, 0.4820512820512820595, 0.4846153846153846145, 0.4871794871794871695, 0.4897435897435897245, 0.4923076923076923350, 0.4948717948717948900, 0.4974358974358974450, 0.5000000000000000000, 0.5025641025641025550, 0.5051282051282051100, 0.5076923076923076650, 0.5102564102564102200, 0.5128205128205127750, 0.5153846153846153300, 0.5179487179487179960, 0.5205128205128205510, 0.5230769230769231060, 0.5256410256410256610, 0.5282051282051282159, 0.5307692307692307709, 0.5333333333333333259, 0.5358974358974358809, 0.5384615384615384359, 0.5410256410256409909, 0.5435897435897435459, 0.5461538461538461009, 0.5487179487179487669, 0.5512820512820513219, 0.5538461538461538769, 0.5564102564102564319, 0.5589743589743589869, 0.5615384615384615419, 0.5641025641025640969, 0.5666666666666666519, 0.5692307692307692069, 0.5717948717948717618, 0.5743589743589743168, 0.5769230769230768718, 0.5794871794871795379, 0.5820512820512820928, 0.5846153846153846478, 0.5871794871794872028, 0.5897435897435897578, 0.5923076923076923128, 0.5948717948717948678, 0.5974358974358974228, 0.5999999999999999778, 0.6025641025641025328, 0.6051282051282050878, 0.6076923076923076428, 0.6102564102564103088, 0.6128205128205128638, 0.6153846153846154188, 0.6179487179487179738, 0.6205128205128205288, 0.6230769230769230838, 0.6256410256410256387, 0.6282051282051281937, 0.6307692307692307487, 0.6333333333333333037, 0.6358974358974358587, 0.6384615384615384137, 0.6410256410256410797, 0.6435897435897436347, 0.6461538461538461897, 0.6487179487179487447, 0.6512820512820512997, 0.6538461538461538547, 0.6564102564102564097, 0.6589743589743589647, 0.6615384615384615197, 0.6641025641025640747, 0.6666666666666666297, 0.6692307692307691847, 0.6717948717948717396, 0.6743589743589744057, 0.6769230769230769607, 0.6794871794871795156, 0.6820512820512820706, 0.6846153846153846256, 0.6871794871794871806, 0.6897435897435897356, 0.6923076923076922906, 0.6948717948717948456, 0.6974358974358974006, 0.6999999999999999556, 0.7025641025641025106, 0.7051282051282051766, 0.7076923076923077316, 0.7102564102564102866, 0.7128205128205128416, 0.7153846153846153966, 0.7179487179487179516, 0.7205128205128205066, 0.7230769230769230616, 0.7256410256410256165, 0.7282051282051281715, 0.7307692307692307265, 0.7333333333333332815, 0.7358974358974359475, 0.7384615384615385025, 0.7410256410256410575, 0.7435897435897436125, 0.7461538461538461675, 0.7487179487179487225, 0.7512820512820512775, 0.7538461538461538325, 0.7564102564102563875, 0.7589743589743589425, 0.7615384615384614975, 0.7641025641025640525, 0.7666666666666667185, 0.7692307692307692735, 0.7717948717948718285, 0.7743589743589743835, 0.7769230769230769384, 0.7794871794871794934, 0.7820512820512820484, 0.7846153846153846034, 0.7871794871794871584, 0.7897435897435897134, 0.7923076923076922684, 0.7948717948717948234, 0.7974358974358974894, 0.8000000000000000444, 0.8025641025641025994, 0.8051282051282051544, 0.8076923076923077094, 0.8102564102564102644, 0.8128205128205128194, 0.8153846153846153744, 0.8179487179487179294, 0.8205128205128204844, 0.8230769230769230393, 0.8256410256410255943, 0.8282051282051282604, 0.8307692307692308153, 0.8333333333333333703, 0.8358974358974359253, 0.8384615384615384803, 0.8410256410256410353, 0.8435897435897435903, 0.8461538461538461453, 0.8487179487179487003, 0.8512820512820512553, 0.8538461538461538103, 0.8564102564102563653, 0.8589743589743589203, 0.8615384615384615863, 0.8641025641025641413, 0.8666666666666666963, 0.8692307692307692513, 0.8717948717948718063, 0.8743589743589743613, 0.8769230769230769162, 0.8794871794871794712, 0.8820512820512820262, 0.8846153846153845812, 0.8871794871794871362, 0.8897435897435896912, 0.8923076923076923572, 0.8948717948717949122, 0.8974358974358974672, 0.9000000000000000222, 0.9025641025641025772, 0.9051282051282051322, 0.9076923076923076872, 0.9102564102564102422, 0.9128205128205127972, 0.9153846153846153522, 0.9179487179487179072, 0.9205128205128204621, 0.9230769230769231282, 0.9256410256410256832, 0.9282051282051282382, 0.9307692307692307931, 0.9333333333333333481, 0.9358974358974359031, 0.9384615384615384581, 0.9410256410256410131, 0.9435897435897435681, 0.9461538461538461231, 0.9487179487179486781, 0.9512820512820512331, 0.9538461538461538991, 0.9564102564102564541, 0.9589743589743590091, 0.9615384615384615641, 0.9641025641025641191, 0.9666666666666666741, 0.9692307692307692291, 0.9717948717948717841, 0.9743589743589743390, 0.9769230769230768940, 0.9794871794871794490, 0.9820512820512820040, 0.9846153846153846700, 0.9871794871794872250, 0.9897435897435897800, 0.9923076923076923350, 0.9948717948717948900, 0.9974358974358974450, 1.000000000000000000 ),
 .UNSPECIFIED. ) 
 GEOMETRIC_REPRESENTATION_ITEM ( )  RATIONAL_B_SPLINE_SURFACE ( (
 ( 1.000000000000000000, 0.9510565162951535312, 1.000000000000000000, 0.9510565162951535312, 1.000000000000000000, 0.9510565162951535312, 1.000000000000000000, 0.9510565162951535312, 1.000000000000000000, 0.9510565162951535312, 1.000000000000000000, 0.9510565162951535312, 1.000000000000000000, 0.9510565162951535312, 1.000000000000000000, 0.9510565162951535312, 1.000000000000000000, 0.9510565162951535312, 1.000000000000000000, 0.9510565162951535312, 1.000000000000000000, 0.9510565162951535312, 1.000000000000000000, 0.9510565162951535312, 1.000000000000000000, 0.9510565162951535312, 1.000000000000000000, 0.9510565162951535312, 1.000000000000000000, 0.9510565162951535312, 1.000000000000000000, 0.9510565162951535312, 1.000000000000000000, 0.9510565162951535312, 1.000000000000000000, 0.9510565162951535312, 1.000000000000000000, 0.9510565162951535312, 1.000000000000000000, 0.9510565162951535312, 1.000000000000000000, 0.9510565162951535312, 1.000000000000000000, 0.9510565162951535312, 1.000000000000000000, 0.9510565162951535312, 1.000000000000000000, 0.9510565162951535312, 1.000000000000000000, 0.9510565162951535312, 1.000000000000000000, 0.9510565162951535312, 1.000000000000000000, 0.9510565162951535312, 1.000000000000000000, 0.9510565162951535312, 1.000000000000000000, 0.9510565162951535312, 1.000000000000000000, 0.9510565162951535312, 1.000000000000000000, 0.9510565162951535312, 1.000000000000000000, 0.9510565162951535312, 1.000000000000000000, 0.9510565162951535312, 1.000000000000000000, 0.9510565162951535312, 1.000000000000000000, 0.9510565162951535312, 1.000000000000000000, 0.9510565162951535312, 1.000000000000000000, 0.9510565162951535312, 1.000000000000000000, 0.9510565162951535312, 1.000000000000000000, 0.9510565162951535312, 1.000000000000000000, 0.9510565162951535312, 1.000000000000000000, 0.9510565162951535312, 1.000000000000000000, 0.9510565162951535312, 1.000000000000000000, 0.9510565162951535312, 1.000000000000000000, 0.9510565162951535312, 1.000000000000000000, 0.9510565162951535312, 1.000000000000000000, 0.9510565162951535312, 1.000000000000000000, 0.9510565162951535312, 1.000000000000000000, 0.9510565162951535312, 1.000000000000000000, 0.9510565162951535312, 1.000000000000000000, 0.9510565162951535312, 1.000000000000000000, 0.9510565162951535312, 1.000000000000000000, 0.9510565162951535312, 1.000000000000000000, 0.9510565162951535312, 1.000000000000000000, 0.9510565162951535312, 1.000000000000000000, 0.9510565162951535312, 1.000000000000000000, 0.9510565162951535312, 1.000000000000000000, 0.9510565162951535312, 1.000000000000000000, 0.9510565162951535312, 1.000000000000000000, 0.9510565162951535312, 1.000000000000000000, 0.9510565162951535312, 1.000000000000000000, 0.9510565162951535312, 1.000000000000000000, 0.9510565162951535312, 1.000000000000000000, 0.9510565162951535312, 1.000000000000000000, 0.9510565162951535312, 1.000000000000000000, 0.9510565162951535312, 1.000000000000000000, 0.9510565162951535312, 1.000000000000000000, 0.9510565162951535312, 1.000000000000000000, 0.9510565162951535312, 1.000000000000000000, 0.9510565162951535312, 1.000000000000000000, 0.9510565162951535312, 1.000000000000000000, 0.9510565162951535312, 1.000000000000000000, 0.9510565162951535312, 1.000000000000000000, 0.9510565162951535312, 1.000000000000000000, 0.9510565162951535312, 1.000000000000000000, 0.9510565162951535312, 1.000000000000000000, 0.9510565162951535312, 1.000000000000000000, 0.9510565162951535312, 1.000000000000000000, 0.9510565162951535312, 1.000000000000000000, 0.9510565162951535312, 1.000000000000000000, 0.9510565162951535312, 1.000000000000000000, 0.9510565162951535312, 1.000000000000000000, 0.9510565162951535312, 1.000000000000000000, 0.9510565162951535312, 1.000000000000000000, 0.9510565162951535312, 1.000000000000000000, 0.9510565162951535312, 1.000000000000000000, 0.9510565162951535312, 1.000000000000000000, 0.9510565162951535312, 1.000000000000000000, 0.9510565162951535312, 1.000000000000000000, 0.9510565162951535312, 1.000000000000000000, 0.9510565162951535312, 1.000000000000000000, 0.9510565162951535312, 1.000000000000000000, 0.9510565162951535312, 1.000000000000000000, 0.9510565162951535312, 1.000000000000000000, 0.9510565162951535312, 1.000000000000000000, 0.9510565162951535312, 1.000000000000000000, 0.9510565162951535312, 1.000000000000000000, 0.9510565162951535312, 1.000000000000000000, 0.9510565162951535312, 1.000000000000000000, 0.9510565162951535312, 1.000000000000000000, 0.9510565162951535312, 1.000000000000000000, 0.9510565162951535312, 1.000000000000000000, 0.9510565162951535312, 1.000000000000000000, 0.9510565162951535312, 1.000000000000000000, 0.9510565162951535312, 1.000000000000000000, 0.9510565162951535312, 1.000000000000000000, 0.9510565162951535312, 1.000000000000000000, 0.9510565162951535312, 1.000000000000000000, 0.9510565162951535312, 1.000000000000000000, 0.9510565162951535312, 1.000000000000000000, 0.9510565162951535312, 1.000000000000000000, 0.9510565162951535312, 1.000000000000000000, 0.9510565162951535312, 1.000000000000000000, 0.9510565162951535312, 1.000000000000000000, 0.9510565162951535312, 1.000000000000000000, 0.9510565162951535312, 1.000000000000000000, 0.9510565162951535312, 1.000000000000000000, 0.9510565162951535312, 1.000000000000000000, 0.9510565162951535312, 1.000000000000000000, 0.9510565162951535312, 1.000000000000000000, 0.9510565162951535312, 1.000000000000000000, 0.9510565162951535312, 1.000000000000000000, 0.9510565162951535312, 1.000000000000000000, 0.9510565162951535312, 1.000000000000000000, 0.9510565162951535312, 1.000000000000000000, 0.9510565162951535312, 1.000000000000000000, 0.9510565162951535312, 1.000000000000000000, 0.9510565162951535312, 1.000000000000000000, 0.9510565162951535312, 1.000000000000000000, 0.9510565162951535312, 1.000000000000000000, 0.9510565162951535312, 1.000000000000000000, 0.9510565162951535312, 1.000000000000000000, 0.9510565162951535312, 1.000000000000000000, 0.9510565162951535312, 1.000000000000000000, 0.9510565162951535312, 1.000000000000000000, 0.9510565162951535312, 1.000000000000000000, 0.9510565162951535312, 1.000000000000000000, 0.9510565162951535312, 1.000000000000000000, 0.9510565162951535312, 1.000000000000000000, 0.9510565162951535312, 1.000000000000000000, 0.9510565162951535312, 1.000000000000000000, 0.9510565162951535312, 1.000000000000000000, 0.9510565162951535312, 1.000000000000000000, 0.9510565162951535312, 1.000000000000000000, 0.9510565162951535312, 1.000000000000000000, 0.9510565162951535312, 1.000000000000000000, 0.9510565162951535312, 1.000000000000000000, 0.9510565162951535312, 1.000000000000000000, 0.9510565162951535312, 1.000000000000000000, 0.9510565162951535312, 1.000000000000000000, 0.9510565162951535312, 1.000000000000000000, 0.9510565162951535312, 1.000000000000000000, 0.9510565162951535312, 1.000000000000000000, 0.9510565162951535312, 1.000000000000000000, 0.9510565162951535312, 1.000000000000000000, 0.9510565162951535312, 1.000000000000000000, 0.9510565162951535312, 1.000000000000000000, 0.9510565162951535312, 1.000000000000000000, 0.9510565162951535312, 1.000000000000000000, 0.9510565162951535312, 1.000000000000000000, 0.9510565162951535312, 1.000000000000000000, 0.9510565162951535312, 1.000000000000000000, 0.9510565162951535312, 1.000000000000000000, 0.9510565162951535312, 1.000000000000000000, 0.9510565162951535312, 1.000000000000000000, 0.9510565162951535312, 1.000000000000000000, 0.9510565162951535312, 1.000000000000000000, 0.9510565162951535312, 1.000000000000000000, 0.9510565162951535312, 1.000000000000000000, 0.9510565162951535312, 1.000000000000000000, 0.9510565162951535312, 1.000000000000000000, 0.9510565162951535312, 1.000000000000000000, 0.9510565162951535312, 1.000000000000000000, 0.9510565162951535312, 1.000000000000000000, 0.9510565162951535312, 1.000000000000000000, 0.9510565162951535312, 1.000000000000000000, 0.9510565162951535312, 1.000000000000000000, 0.9510565162951535312, 1.000000000000000000, 0.9510565162951535312, 1.000000000000000000, 0.9510565162951535312, 1.000000000000000000, 0.9510565162951535312, 1.000000000000000000, 0.9510565162951535312, 1.000000000000000000, 0.9510565162951535312, 1.000000000000000000, 0.9510565162951535312, 1.000000000000000000, 0.9510565162951535312, 1.000000000000000000, 0.9510565162951535312, 1.000000000000000000, 0.9510565162951535312, 1.000000000000000000, 0.9510565162951535312, 1.000000000000000000, 0.9510565162951535312, 1.000000000000000000, 0.9510565162951535312, 1.000000000000000000, 0.9510565162951535312, 1.000000000000000000, 0.9510565162951535312, 1.000000000000000000, 0.9510565162951535312, 1.000000000000000000, 0.9510565162951535312, 1.000000000000000000, 0.9510565162951535312, 1.000000000000000000, 0.9510565162951535312, 1.000000000000000000, 0.9510565162951535312, 1.000000000000000000, 0.9510565162951535312, 1.000000000000000000, 0.9510565162951535312, 1.000000000000000000, 0.9510565162951535312, 1.000000000000000000, 0.9510565162951535312, 1.000000000000000000, 0.9510565162951535312, 1.000000000000000000, 0.9510565162951535312, 1.000000000000000000, 0.9510565162951535312, 1.000000000000000000, 0.9510565162951535312, 1.000000000000000000, 0.9510565162951535312, 1.000000000000000000, 0.9510565162951535312, 1.000000000000000000, 0.9510565162951535312, 1.000000000000000000, 0.9510565162951535312, 1.000000000000000000, 0.9510565162951535312, 1.000000000000000000, 0.9510565162951535312, 1.000000000000000000, 0.9510565162951535312, 1.000000000000000000, 0.9510565162951535312, 1.000000000000000000, 0.9510565162951535312, 1.000000000000000000, 0.9510565162951535312, 1.000000000000000000, 0.9510565162951535312, 1.000000000000000000, 0.9510565162951535312, 1.000000000000000000, 0.9510565162951535312, 1.000000000000000000, 0.9510565162951535312, 1.000000000000000000, 0.9510565162951535312, 1.000000000000000000, 0.9510565162951535312, 1.000000000000000000, 0.9510565162951535312, 1.000000000000000000, 0.9510565162951535312, 1.000000000000000000, 0.9510565162951535312, 1.000000000000000000, 0.9510565162951535312, 1.000000000000000000, 0.9510565162951535312, 1.000000000000000000, 0.9510565162951535312, 1.000000000000000000, 0.9510565162951535312, 1.000000000000000000, 0.9510565162951535312, 1.000000000000000000, 0.9510565162951535312, 1.000000000000000000, 0.9510565162951535312, 1.000000000000000000, 0.9510565162951535312, 1.000000000000000000, 0.9510565162951535312, 1.000000000000000000, 0.9510565162951535312, 1.000000000000000000, 0.9510565162951535312, 1.000000000000000000, 0.9510565162951535312, 1.000000000000000000, 0.9510565162951535312, 1.000000000000000000, 0.9510565162951535312, 1.000000000000000000, 0.9510565162951535312, 1.000000000000000000, 0.9510565162951535312, 1.000000000000000000, 0.9510565162951535312, 1.000000000000000000, 0.9510565162951535312, 1.000000000000000000, 0.9510565162951535312, 1.000000000000000000, 0.9510565162951535312, 1.000000000000000000, 0.9510565162951535312, 1.000000000000000000, 0.9510565162951535312, 1.000000000000000000, 0.9510565162951535312, 1.000000000000000000, 0.9510565162951535312, 1.000000000000000000, 0.9510565162951535312, 1.000000000000000000, 0.9510565162951535312, 1.000000000000000000, 0.9510565162951535312, 1.000000000000000000, 0.9510565162951535312, 1.000000000000000000, 0.9510565162951535312, 1.000000000000000000, 0.9510565162951535312, 1.000000000000000000, 0.9510565162951535312, 1.000000000000000000, 0.9510565162951535312, 1.000000000000000000, 0.9510565162951535312, 1.000000000000000000, 0.9510565162951535312, 1.000000000000000000, 0.9510565162951535312, 1.000000000000000000, 0.9510565162951535312, 1.000000000000000000, 0.9510565162951535312, 1.000000000000000000, 0.9510565162951535312, 1.000000000000000000, 0.9510565162951535312, 1.000000000000000000, 0.9510565162951535312, 1.000000000000000000, 0.9510565162951535312, 1.000000000000000000, 0.9510565162951535312, 1.000000000000000000, 0.9510565162951535312, 1.000000000000000000, 0.9510565162951535312, 1.000000000000000000, 0.9510565162951535312, 1.000000000000000000, 0.9510565162951535312, 1.000000000000000000, 0.9510565162951535312, 1.000000000000000000, 0.9510565162951535312, 1.000000000000000000, 0.9510565162951535312, 1.000000000000000000, 0.9510565162951535312, 1.000000000000000000, 0.9510565162951535312, 1.000000000000000000, 0.9510565162951535312, 1.000000000000000000, 0.9510565162951535312, 1.000000000000000000, 0.9510565162951535312, 1.000000000000000000, 0.9510565162951535312, 1.000000000000000000, 0.9510565162951535312, 1.000000000000000000, 0.9510565162951535312, 1.000000000000000000, 0.9510565162951535312, 1.000000000000000000, 0.9510565162951535312, 1.000000000000000000, 0.9510565162951535312, 1.000000000000000000, 0.9510565162951535312, 1.000000000000000000, 0.9510565162951535312, 1.000000000000000000, 0.9510565162951535312, 1.000000000000000000, 0.9510565162951535312, 1.000000000000000000, 0.9510565162951535312, 1.000000000000000000, 0.9510565162951535312, 1.000000000000000000, 0.9510565162951535312, 1.000000000000000000, 0.9510565162951535312, 1.000000000000000000, 0.9510565162951535312, 1.000000000000000000, 0.9510565162951535312, 1.000000000000000000, 0.9510565162951535312, 1.000000000000000000, 0.9510565162951535312, 1.000000000000000000, 0.9510565162951535312, 1.000000000000000000, 0.9510565162951535312, 1.000000000000000000, 0.9510565162951535312, 1.000000000000000000, 0.9510565162951535312, 1.000000000000000000, 0.9510565162951535312, 1.000000000000000000, 0.9510565162951535312, 1.000000000000000000, 0.9510565162951535312, 1.000000000000000000, 0.9510565162951535312, 1.000000000000000000, 0.9510565162951535312, 1.000000000000000000, 0.9510565162951535312, 1.000000000000000000, 0.9510565162951535312, 1.000000000000000000, 0.9510565162951535312, 1.000000000000000000, 0.9510565162951535312, 1.000000000000000000, 0.9510565162951535312, 1.000000000000000000, 0.9510565162951535312, 1.000000000000000000, 0.9510565162951535312, 1.000000000000000000, 0.9510565162951535312, 1.000000000000000000, 0.9510565162951535312, 1.000000000000000000, 0.9510565162951535312, 1.000000000000000000, 0.9510565162951535312, 1.000000000000000000, 0.9510565162951535312, 1.000000000000000000, 0.9510565162951535312, 1.000000000000000000, 0.9510565162951535312, 1.000000000000000000, 0.9510565162951535312, 1.000000000000000000, 0.9510565162951535312, 1.000000000000000000, 0.9510565162951535312, 1.000000000000000000, 0.9510565162951535312, 1.000000000000000000, 0.9510565162951535312, 1.000000000000000000, 0.9510565162951535312, 1.000000000000000000, 0.9510565162951535312, 1.000000000000000000, 0.9510565162951535312, 1.000000000000000000, 0.9510565162951535312, 1.000000000000000000, 0.9510565162951535312, 1.000000000000000000, 0.9510565162951535312, 1.000000000000000000, 0.9510565162951535312, 1.000000000000000000, 0.9510565162951535312, 1.000000000000000000, 0.9510565162951535312, 1.000000000000000000, 0.9510565162951535312, 1.000000000000000000, 0.9510565162951535312, 1.000000000000000000, 0.9510565162951535312, 1.000000000000000000, 0.9510565162951535312, 1.000000000000000000, 0.9510565162951535312, 1.000000000000000000, 0.9510565162951535312, 1.000000000000000000, 0.9510565162951535312, 1.000000000000000000, 0.9510565162951535312, 1.000000000000000000, 0.9510565162951535312, 1.000000000000000000, 0.9510565162951535312, 1.000000000000000000, 0.9510565162951535312, 1.000000000000000000, 0.9510565162951535312, 1.000000000000000000, 0.9510565162951535312, 1.000000000000000000, 0.9510565162951535312, 1.000000000000000000, 0.9510565162951535312, 1.000000000000000000, 0.9510565162951535312, 1.000000000000000000, 0.9510565162951535312, 1.000000000000000000, 0.9510565162951535312, 1.000000000000000000, 0.9510565162951535312, 1.000000000000000000, 0.9510565162951535312, 1.000000000000000000, 0.9510565162951535312, 1.000000000000000000, 0.9510565162951535312, 1.000000000000000000, 0.9510565162951535312, 1.000000000000000000, 0.9510565162951535312, 1.000000000000000000, 0.9510565162951535312, 1.000000000000000000, 0.9510565162951535312, 1.000000000000000000, 0.9510565162951535312, 1.000000000000000000, 0.9510565162951535312, 1.000000000000000000, 0.9510565162951535312, 1.000000000000000000, 0.9510565162951535312, 1.000000000000000000, 0.9510565162951535312, 1.000000000000000000, 0.9510565162951535312, 1.000000000000000000, 0.9510565162951535312, 1.000000000000000000, 0.9510565162951535312, 1.000000000000000000, 0.9510565162951535312, 1.000000000000000000, 0.9510565162951535312, 1.000000000000000000, 0.9510565162951535312, 1.000000000000000000, 0.9510565162951535312, 1.000000000000000000, 0.9510565162951535312, 1.000000000000000000, 0.9510565162951535312, 1.000000000000000000, 0.9510565162951535312, 1.000000000000000000, 0.9510565162951535312, 1.000000000000000000, 0.9510565162951535312, 1.000000000000000000, 0.9510565162951535312, 1.000000000000000000, 0.9510565162951535312, 1.000000000000000000, 0.9510565162951535312, 1.000000000000000000, 0.9510565162951535312, 1.000000000000000000, 0.9510565162951535312, 1.000000000000000000, 0.9510565162951535312, 1.000000000000000000, 0.9510565162951535312, 1.000000000000000000, 0.9510565162951535312, 1.000000000000000000, 0.9510565162951535312, 1.000000000000000000, 0.9510565162951535312, 1.000000000000000000, 0.9510565162951535312, 1.000000000000000000, 0.9510565162951535312, 1.000000000000000000, 0.9510565162951535312, 1.000000000000000000, 0.9510565162951535312, 1.000000000000000000, 0.9510565162951535312, 1.000000000000000000),
 ( 1.000000000000000000, 0.9510565162951535312, 1.000000000000000000, 0.9510565162951535312, 1.000000000000000000, 0.9510565162951535312, 1.000000000000000000, 0.9510565162951535312, 1.000000000000000000, 0.9510565162951535312, 1.000000000000000000, 0.9510565162951535312, 1.000000000000000000, 0.9510565162951535312, 1.000000000000000000, 0.9510565162951535312, 1.000000000000000000, 0.9510565162951535312, 1.000000000000000000, 0.9510565162951535312, 1.000000000000000000, 0.9510565162951535312, 1.000000000000000000, 0.9510565162951535312, 1.000000000000000000, 0.9510565162951535312, 1.000000000000000000, 0.9510565162951535312, 1.000000000000000000, 0.9510565162951535312, 1.000000000000000000, 0.9510565162951535312, 1.000000000000000000, 0.9510565162951535312, 1.000000000000000000, 0.9510565162951535312, 1.000000000000000000, 0.9510565162951535312, 1.000000000000000000, 0.9510565162951535312, 1.000000000000000000, 0.9510565162951535312, 1.000000000000000000, 0.9510565162951535312, 1.000000000000000000, 0.9510565162951535312, 1.000000000000000000, 0.9510565162951535312, 1.000000000000000000, 0.9510565162951535312, 1.000000000000000000, 0.9510565162951535312, 1.000000000000000000, 0.9510565162951535312, 1.000000000000000000, 0.9510565162951535312, 1.000000000000000000, 0.9510565162951535312, 1.000000000000000000, 0.9510565162951535312, 1.000000000000000000, 0.9510565162951535312, 1.000000000000000000, 0.9510565162951535312, 1.000000000000000000, 0.9510565162951535312, 1.000000000000000000, 0.9510565162951535312, 1.000000000000000000, 0.9510565162951535312, 1.000000000000000000, 0.9510565162951535312, 1.000000000000000000, 0.9510565162951535312, 1.000000000000000000, 0.9510565162951535312, 1.000000000000000000, 0.9510565162951535312, 1.000000000000000000, 0.9510565162951535312, 1.000000000000000000, 0.9510565162951535312, 1.000000000000000000, 0.9510565162951535312, 1.000000000000000000, 0.9510565162951535312, 1.000000000000000000, 0.9510565162951535312, 1.000000000000000000, 0.9510565162951535312, 1.000000000000000000, 0.9510565162951535312, 1.000000000000000000, 0.9510565162951535312, 1.000000000000000000, 0.9510565162951535312, 1.000000000000000000, 0.9510565162951535312, 1.000000000000000000, 0.9510565162951535312, 1.000000000000000000, 0.9510565162951535312, 1.000000000000000000, 0.9510565162951535312, 1.000000000000000000, 0.9510565162951535312, 1.000000000000000000, 0.9510565162951535312, 1.000000000000000000, 0.9510565162951535312, 1.000000000000000000, 0.9510565162951535312, 1.000000000000000000, 0.9510565162951535312, 1.000000000000000000, 0.9510565162951535312, 1.000000000000000000, 0.9510565162951535312, 1.000000000000000000, 0.9510565162951535312, 1.000000000000000000, 0.9510565162951535312, 1.000000000000000000, 0.9510565162951535312, 1.000000000000000000, 0.9510565162951535312, 1.000000000000000000, 0.9510565162951535312, 1.000000000000000000, 0.9510565162951535312, 1.000000000000000000, 0.9510565162951535312, 1.000000000000000000, 0.9510565162951535312, 1.000000000000000000, 0.9510565162951535312, 1.000000000000000000, 0.9510565162951535312, 1.000000000000000000, 0.9510565162951535312, 1.000000000000000000, 0.9510565162951535312, 1.000000000000000000, 0.9510565162951535312, 1.000000000000000000, 0.9510565162951535312, 1.000000000000000000, 0.9510565162951535312, 1.000000000000000000, 0.9510565162951535312, 1.000000000000000000, 0.9510565162951535312, 1.000000000000000000, 0.9510565162951535312, 1.000000000000000000, 0.9510565162951535312, 1.000000000000000000, 0.9510565162951535312, 1.000000000000000000, 0.9510565162951535312, 1.000000000000000000, 0.9510565162951535312, 1.000000000000000000, 0.9510565162951535312, 1.000000000000000000, 0.9510565162951535312, 1.000000000000000000, 0.9510565162951535312, 1.000000000000000000, 0.9510565162951535312, 1.000000000000000000, 0.9510565162951535312, 1.000000000000000000, 0.9510565162951535312, 1.000000000000000000, 0.9510565162951535312, 1.000000000000000000, 0.9510565162951535312, 1.000000000000000000, 0.9510565162951535312, 1.000000000000000000, 0.9510565162951535312, 1.000000000000000000, 0.9510565162951535312, 1.000000000000000000, 0.9510565162951535312, 1.000000000000000000, 0.9510565162951535312, 1.000000000000000000, 0.9510565162951535312, 1.000000000000000000, 0.9510565162951535312, 1.000000000000000000, 0.9510565162951535312, 1.000000000000000000, 0.9510565162951535312, 1.000000000000000000, 0.9510565162951535312, 1.000000000000000000, 0.9510565162951535312, 1.000000000000000000, 0.9510565162951535312, 1.000000000000000000, 0.9510565162951535312, 1.000000000000000000, 0.9510565162951535312, 1.000000000000000000, 0.9510565162951535312, 1.000000000000000000, 0.9510565162951535312, 1.000000000000000000, 0.9510565162951535312, 1.000000000000000000, 0.9510565162951535312, 1.000000000000000000, 0.9510565162951535312, 1.000000000000000000, 0.9510565162951535312, 1.000000000000000000, 0.9510565162951535312, 1.000000000000000000, 0.9510565162951535312, 1.000000000000000000, 0.9510565162951535312, 1.000000000000000000, 0.9510565162951535312, 1.000000000000000000, 0.9510565162951535312, 1.000000000000000000, 0.9510565162951535312, 1.000000000000000000, 0.9510565162951535312, 1.000000000000000000, 0.9510565162951535312, 1.000000000000000000, 0.9510565162951535312, 1.000000000000000000, 0.9510565162951535312, 1.000000000000000000, 0.9510565162951535312, 1.000000000000000000, 0.9510565162951535312, 1.000000000000000000, 0.9510565162951535312, 1.000000000000000000, 0.9510565162951535312, 1.000000000000000000, 0.9510565162951535312, 1.000000000000000000, 0.9510565162951535312, 1.000000000000000000, 0.9510565162951535312, 1.000000000000000000, 0.9510565162951535312, 1.000000000000000000, 0.9510565162951535312, 1.000000000000000000, 0.9510565162951535312, 1.000000000000000000, 0.9510565162951535312, 1.000000000000000000, 0.9510565162951535312, 1.000000000000000000, 0.9510565162951535312, 1.000000000000000000, 0.9510565162951535312, 1.000000000000000000, 0.9510565162951535312, 1.000000000000000000, 0.9510565162951535312, 1.000000000000000000, 0.9510565162951535312, 1.000000000000000000, 0.9510565162951535312, 1.000000000000000000, 0.9510565162951535312, 1.000000000000000000, 0.9510565162951535312, 1.000000000000000000, 0.9510565162951535312, 1.000000000000000000, 0.9510565162951535312, 1.000000000000000000, 0.9510565162951535312, 1.000000000000000000, 0.9510565162951535312, 1.000000000000000000, 0.9510565162951535312, 1.000000000000000000, 0.9510565162951535312, 1.000000000000000000, 0.9510565162951535312, 1.000000000000000000, 0.9510565162951535312, 1.000000000000000000, 0.9510565162951535312, 1.000000000000000000, 0.9510565162951535312, 1.000000000000000000, 0.9510565162951535312, 1.000000000000000000, 0.9510565162951535312, 1.000000000000000000, 0.9510565162951535312, 1.000000000000000000, 0.9510565162951535312, 1.000000000000000000, 0.9510565162951535312, 1.000000000000000000, 0.9510565162951535312, 1.000000000000000000, 0.9510565162951535312, 1.000000000000000000, 0.9510565162951535312, 1.000000000000000000, 0.9510565162951535312, 1.000000000000000000, 0.9510565162951535312, 1.000000000000000000, 0.9510565162951535312, 1.000000000000000000, 0.9510565162951535312, 1.000000000000000000, 0.9510565162951535312, 1.000000000000000000, 0.9510565162951535312, 1.000000000000000000, 0.9510565162951535312, 1.000000000000000000, 0.9510565162951535312, 1.000000000000000000, 0.9510565162951535312, 1.000000000000000000, 0.9510565162951535312, 1.000000000000000000, 0.9510565162951535312, 1.000000000000000000, 0.9510565162951535312, 1.000000000000000000, 0.9510565162951535312, 1.000000000000000000, 0.9510565162951535312, 1.000000000000000000, 0.9510565162951535312, 1.000000000000000000, 0.9510565162951535312, 1.000000000000000000, 0.9510565162951535312, 1.000000000000000000, 0.9510565162951535312, 1.000000000000000000, 0.9510565162951535312, 1.000000000000000000, 0.9510565162951535312, 1.000000000000000000, 0.9510565162951535312, 1.000000000000000000, 0.9510565162951535312, 1.000000000000000000, 0.9510565162951535312, 1.000000000000000000, 0.9510565162951535312, 1.000000000000000000, 0.9510565162951535312, 1.000000000000000000, 0.9510565162951535312, 1.000000000000000000, 0.9510565162951535312, 1.000000000000000000, 0.9510565162951535312, 1.000000000000000000, 0.9510565162951535312, 1.000000000000000000, 0.9510565162951535312, 1.000000000000000000, 0.9510565162951535312, 1.000000000000000000, 0.9510565162951535312, 1.000000000000000000, 0.9510565162951535312, 1.000000000000000000, 0.9510565162951535312, 1.000000000000000000, 0.9510565162951535312, 1.000000000000000000, 0.9510565162951535312, 1.000000000000000000, 0.9510565162951535312, 1.000000000000000000, 0.9510565162951535312, 1.000000000000000000, 0.9510565162951535312, 1.000000000000000000, 0.9510565162951535312, 1.000000000000000000, 0.9510565162951535312, 1.000000000000000000, 0.9510565162951535312, 1.000000000000000000, 0.9510565162951535312, 1.000000000000000000, 0.9510565162951535312, 1.000000000000000000, 0.9510565162951535312, 1.000000000000000000, 0.9510565162951535312, 1.000000000000000000, 0.9510565162951535312, 1.000000000000000000, 0.9510565162951535312, 1.000000000000000000, 0.9510565162951535312, 1.000000000000000000, 0.9510565162951535312, 1.000000000000000000, 0.9510565162951535312, 1.000000000000000000, 0.9510565162951535312, 1.000000000000000000, 0.9510565162951535312, 1.000000000000000000, 0.9510565162951535312, 1.000000000000000000, 0.9510565162951535312, 1.000000000000000000, 0.9510565162951535312, 1.000000000000000000, 0.9510565162951535312, 1.000000000000000000, 0.9510565162951535312, 1.000000000000000000, 0.9510565162951535312, 1.000000000000000000, 0.9510565162951535312, 1.000000000000000000, 0.9510565162951535312, 1.000000000000000000, 0.9510565162951535312, 1.000000000000000000, 0.9510565162951535312, 1.000000000000000000, 0.9510565162951535312, 1.000000000000000000, 0.9510565162951535312, 1.000000000000000000, 0.9510565162951535312, 1.000000000000000000, 0.9510565162951535312, 1.000000000000000000, 0.9510565162951535312, 1.000000000000000000, 0.9510565162951535312, 1.000000000000000000, 0.9510565162951535312, 1.000000000000000000, 0.9510565162951535312, 1.000000000000000000, 0.9510565162951535312, 1.000000000000000000, 0.9510565162951535312, 1.000000000000000000, 0.9510565162951535312, 1.000000000000000000, 0.9510565162951535312, 1.000000000000000000, 0.9510565162951535312, 1.000000000000000000, 0.9510565162951535312, 1.000000000000000000, 0.9510565162951535312, 1.000000000000000000, 0.9510565162951535312, 1.000000000000000000, 0.9510565162951535312, 1.000000000000000000, 0.9510565162951535312, 1.000000000000000000, 0.9510565162951535312, 1.000000000000000000, 0.9510565162951535312, 1.000000000000000000, 0.9510565162951535312, 1.000000000000000000, 0.9510565162951535312, 1.000000000000000000, 0.9510565162951535312, 1.000000000000000000, 0.9510565162951535312, 1.000000000000000000, 0.9510565162951535312, 1.000000000000000000, 0.9510565162951535312, 1.000000000000000000, 0.9510565162951535312, 1.000000000000000000, 0.9510565162951535312, 1.000000000000000000, 0.9510565162951535312, 1.000000000000000000, 0.9510565162951535312, 1.000000000000000000, 0.9510565162951535312, 1.000000000000000000, 0.9510565162951535312, 1.000000000000000000, 0.9510565162951535312, 1.000000000000000000, 0.9510565162951535312, 1.000000000000000000, 0.9510565162951535312, 1.000000000000000000, 0.9510565162951535312, 1.000000000000000000, 0.9510565162951535312, 1.000000000000000000, 0.9510565162951535312, 1.000000000000000000, 0.9510565162951535312, 1.000000000000000000, 0.9510565162951535312, 1.000000000000000000, 0.9510565162951535312, 1.000000000000000000, 0.9510565162951535312, 1.000000000000000000, 0.9510565162951535312, 1.000000000000000000, 0.9510565162951535312, 1.000000000000000000, 0.9510565162951535312, 1.000000000000000000, 0.9510565162951535312, 1.000000000000000000, 0.9510565162951535312, 1.000000000000000000, 0.9510565162951535312, 1.000000000000000000, 0.9510565162951535312, 1.000000000000000000, 0.9510565162951535312, 1.000000000000000000, 0.9510565162951535312, 1.000000000000000000, 0.9510565162951535312, 1.000000000000000000, 0.9510565162951535312, 1.000000000000000000, 0.9510565162951535312, 1.000000000000000000, 0.9510565162951535312, 1.000000000000000000, 0.9510565162951535312, 1.000000000000000000, 0.9510565162951535312, 1.000000000000000000, 0.9510565162951535312, 1.000000000000000000, 0.9510565162951535312, 1.000000000000000000, 0.9510565162951535312, 1.000000000000000000, 0.9510565162951535312, 1.000000000000000000, 0.9510565162951535312, 1.000000000000000000, 0.9510565162951535312, 1.000000000000000000, 0.9510565162951535312, 1.000000000000000000, 0.9510565162951535312, 1.000000000000000000, 0.9510565162951535312, 1.000000000000000000, 0.9510565162951535312, 1.000000000000000000, 0.9510565162951535312, 1.000000000000000000, 0.9510565162951535312, 1.000000000000000000, 0.9510565162951535312, 1.000000000000000000, 0.9510565162951535312, 1.000000000000000000, 0.9510565162951535312, 1.000000000000000000, 0.9510565162951535312, 1.000000000000000000, 0.9510565162951535312, 1.000000000000000000, 0.9510565162951535312, 1.000000000000000000, 0.9510565162951535312, 1.000000000000000000, 0.9510565162951535312, 1.000000000000000000, 0.9510565162951535312, 1.000000000000000000, 0.9510565162951535312, 1.000000000000000000, 0.9510565162951535312, 1.000000000000000000, 0.9510565162951535312, 1.000000000000000000, 0.9510565162951535312, 1.000000000000000000, 0.9510565162951535312, 1.000000000000000000, 0.9510565162951535312, 1.000000000000000000, 0.9510565162951535312, 1.000000000000000000, 0.9510565162951535312, 1.000000000000000000, 0.9510565162951535312, 1.000000000000000000, 0.9510565162951535312, 1.000000000000000000, 0.9510565162951535312, 1.000000000000000000, 0.9510565162951535312, 1.000000000000000000, 0.9510565162951535312, 1.000000000000000000, 0.9510565162951535312, 1.000000000000000000, 0.9510565162951535312, 1.000000000000000000, 0.9510565162951535312, 1.000000000000000000, 0.9510565162951535312, 1.000000000000000000, 0.9510565162951535312, 1.000000000000000000, 0.9510565162951535312, 1.000000000000000000, 0.9510565162951535312, 1.000000000000000000, 0.9510565162951535312, 1.000000000000000000, 0.9510565162951535312, 1.000000000000000000, 0.9510565162951535312, 1.000000000000000000, 0.9510565162951535312, 1.000000000000000000, 0.9510565162951535312, 1.000000000000000000, 0.9510565162951535312, 1.000000000000000000, 0.9510565162951535312, 1.000000000000000000, 0.9510565162951535312, 1.000000000000000000, 0.9510565162951535312, 1.000000000000000000, 0.9510565162951535312, 1.000000000000000000, 0.9510565162951535312, 1.000000000000000000, 0.9510565162951535312, 1.000000000000000000, 0.9510565162951535312, 1.000000000000000000, 0.9510565162951535312, 1.000000000000000000, 0.9510565162951535312, 1.000000000000000000, 0.9510565162951535312, 1.000000000000000000, 0.9510565162951535312, 1.000000000000000000, 0.9510565162951535312, 1.000000000000000000, 0.9510565162951535312, 1.000000000000000000, 0.9510565162951535312, 1.000000000000000000, 0.9510565162951535312, 1.000000000000000000, 0.9510565162951535312, 1.000000000000000000, 0.9510565162951535312, 1.000000000000000000, 0.9510565162951535312, 1.000000000000000000, 0.9510565162951535312, 1.000000000000000000, 0.9510565162951535312, 1.000000000000000000, 0.9510565162951535312, 1.000000000000000000, 0.9510565162951535312, 1.000000000000000000, 0.9510565162951535312, 1.000000000000000000, 0.9510565162951535312, 1.000000000000000000, 0.9510565162951535312, 1.000000000000000000, 0.9510565162951535312, 1.000000000000000000, 0.9510565162951535312, 1.000000000000000000, 0.9510565162951535312, 1.000000000000000000, 0.9510565162951535312, 1.000000000000000000, 0.9510565162951535312, 1.000000000000000000, 0.9510565162951535312, 1.000000000000000000, 0.9510565162951535312, 1.000000000000000000, 0.9510565162951535312, 1.000000000000000000, 0.9510565162951535312, 1.000000000000000000, 0.9510565162951535312, 1.000000000000000000, 0.9510565162951535312, 1.000000000000000000, 0.9510565162951535312, 1.000000000000000000, 0.9510565162951535312, 1.000000000000000000, 0.9510565162951535312, 1.000000000000000000, 0.9510565162951535312, 1.000000000000000000, 0.9510565162951535312, 1.000000000000000000, 0.9510565162951535312, 1.000000000000000000, 0.9510565162951535312, 1.000000000000000000, 0.9510565162951535312, 1.000000000000000000, 0.9510565162951535312, 1.000000000000000000, 0.9510565162951535312, 1.000000000000000000, 0.9510565162951535312, 1.000000000000000000, 0.9510565162951535312, 1.000000000000000000, 0.9510565162951535312, 1.000000000000000000, 0.9510565162951535312, 1.000000000000000000, 0.9510565162951535312, 1.000000000000000000, 0.9510565162951535312, 1.000000000000000000, 0.9510565162951535312, 1.000000000000000000, 0.9510565162951535312, 1.000000000000000000, 0.9510565162951535312, 1.000000000000000000, 0.9510565162951535312, 1.000000000000000000, 0.9510565162951535312, 1.000000000000000000, 0.9510565162951535312, 1.000000000000000000, 0.9510565162951535312, 1.000000000000000000, 0.9510565162951535312, 1.000000000000000000, 0.9510565162951535312, 1.000000000000000000, 0.9510565162951535312, 1.000000000000000000, 0.9510565162951535312, 1.000000000000000000, 0.9510565162951535312, 1.000000000000000000, 0.9510565162951535312, 1.000000000000000000, 0.9510565162951535312, 1.000000000000000000) ) ) 
 REPRESENTATION_ITEM ( '' )  SURFACE ( )  );
#1442 = CARTESIAN_POINT ( 'NONE',  ( -33.58253175000000113, 63.27500000273118985, -10.91162601494193218 ) ) ;
#1443 = DIRECTION ( 'NONE',  ( -1.224646799147353454E-16, 1.000000000000000000, -0.000000000000000000 ) ) ;
#1444 = CARTESIAN_POINT ( 'NONE',  ( -27.16883889988624290, 70.92500000273119554, -19.73931689729374028 ) ) ;
#1445 = CARTESIAN_POINT ( 'NONE',  ( 28.01184896238304134, 27.18229166666666430, 7.505752307972846538 ) ) ;
#1446 = CARTESIAN_POINT ( 'NONE',  ( -15.14183272437241889, 12.70000000000000639, -20.84094480462497856 ) ) ;
#1447 = CARTESIAN_POINT ( 'NONE',  ( 33.58253175000000823, 2.275000002731194293, 10.91162601494192863 ) ) ;
#1448 = CARTESIAN_POINT ( 'NONE',  ( -33.58253175000000113, 19.22500000273118204, 10.91162601494193929 ) ) ;
#1449 = CARTESIAN_POINT ( 'NONE',  ( -5.147494310547423346, 0.9487457239155284716, 32.50000000000000000 ) ) ;
#1450 = CARTESIAN_POINT ( 'NONE',  ( -7.468012846824272799, 47.22878499907602645, 28.02196122052058413 ) ) ;
#1451 = CARTESIAN_POINT ( 'NONE',  ( 2.688165632520823219E-15, 71.87500000273121259, 14.63369212191046387 ) ) ;
#1452 = CARTESIAN_POINT ( 'NONE',  ( -15.01150461594595775, 62.55989583333332149, 26.00068869287368756 ) ) ;
#1453 = CARTESIAN_POINT ( 'NONE',  ( 32.50000000000000711, 22.90000000000000213, 10.55989012756945122 ) ) ;
#1454 = CARTESIAN_POINT ( 'NONE',  ( -19.82091636218621034, 4.549999994537618164, -14.40073868116559552 ) ) ;
#1455 = CARTESIAN_POINT ( 'NONE',  ( -15.00000000000000000, 78.15000000546235981, -4.873795443493594171 ) ) ;
#1456 = CARTESIAN_POINT ( 'NONE',  ( 26.06988505166722803, 66.70795166574268364, -7.025853678916862854 ) ) ;
#1457 = EDGE_CURVE ( 'NONE', #7536, #10957, #5384, .T. ) ;
#1458 = CARTESIAN_POINT ( 'NONE',  ( 33.58253175000000823, 38.02500000273117564, 10.91162601494192863 ) ) ;
#1459 = CARTESIAN_POINT ( 'NONE',  ( 13.91746824999999532, 73.97500000273115006, -4.522059556121118540 ) ) ;
#1460 = CARTESIAN_POINT ( 'NONE',  ( 10.37757302488624767, 49.97500000273117848, 31.93888565452638417 ) ) ;
#1461 = CARTESIAN_POINT ( 'NONE',  ( -2.162160676586882350E-15, 26.87500000273117706, -35.31076352940722529 ) ) ;
#1462 = CARTESIAN_POINT ( 'NONE',  ( 26.29305231718579350, 40.80000000000000426, 19.10302069950537529 ) ) ;
#1463 = ADVANCED_FACE ( 'NONE', ( #2982 ), #389, .T. ) ;
#1464 = CARTESIAN_POINT ( 'NONE',  ( -20.08610463437157989, 8.200000005462390718, -27.64615127144129758 ) ) ;
#1465 = AXIS2_PLACEMENT_3D ( 'NONE', #20580, #4942, #2371 ) ;
#1466 = CARTESIAN_POINT ( 'NONE',  ( -13.91746824999999887, 71.37500000273119838, 0.000000000000000000 ) ) ;
#1467 = CARTESIAN_POINT ( 'NONE',  ( -20.08610463437157989, 69.69999999999997442, -27.64615127144129758 ) ) ;
#1468 = CARTESIAN_POINT ( 'NONE',  ( 23.41746824999999887, 8.524999997268812635, 7.608796670333735079 ) ) ;
#1469 = CARTESIAN_POINT ( 'NONE',  ( -7.543491769121917656, 21.16107666574269075, -28.00173670424536354 ) ) ;
#1470 = VECTOR ( 'NONE', #27620, 1000.000000000000000 ) ;
#1471 = CARTESIAN_POINT ( 'NONE',  ( 14.47279130897151589, 2.824999997268819119, 19.92008829642072953 ) ) ;
#1472 = CARTESIAN_POINT ( 'NONE',  ( -19.11951029504797006, 38.06211833240934084, -19.06425588902558133 ) ) ;
#1473 = CARTESIAN_POINT ( 'NONE',  ( -27.16883889988624290, 77.17500000273118133, -19.73931689729374028 ) ) ;
#1474 = CARTESIAN_POINT ( 'NONE',  ( -33.58253175000000113, 11.22500000273120335, 10.91162601494193929 ) ) ;
#1475 = CARTESIAN_POINT ( 'NONE',  ( 18.94512977948576093, 9.324999997268824004, -13.76444248337722875 ) ) ;
#1476 = CARTESIAN_POINT ( 'NONE',  ( -13.97622843553588901, 62.55989583333332860, 24.20753774853756823 ) ) ;
#1477 = ORIENTED_EDGE ( 'NONE', *, *, #11880, .F. ) ;
#1478 = CARTESIAN_POINT ( 'NONE',  ( 27.16883889988624290, 47.92500000273118843, 19.73931689729373673 ) ) ;
#1479 = CARTESIAN_POINT ( 'NONE',  ( 6.486482029760649416E-15, 21.87500000273118062, 35.31076352940723240 ) ) ;
#1480 = ORIENTED_EDGE ( 'NONE', *, *, #24258, .T. ) ;
#1481 = CARTESIAN_POINT ( 'NONE',  ( -7.505752307973343918, 36.34895833333333570, -28.01184896238290989 ) ) ;
#1482 = CARTESIAN_POINT ( 'NONE',  ( -28.02196122052045268, 30.05246500092397000, 7.468012846824790607 ) ) ;
#1483 = CARTESIAN_POINT ( 'NONE',  ( -15.14183272437242067, 2.700000000000001954, -20.84094480462497856 ) ) ;
#1484 = CARTESIAN_POINT ( 'NONE',  ( -24.50000000000000000, 14.74999999453763166, -3.000384657911015469E-15 ) ) ;
#1485 = CARTESIAN_POINT ( 'NONE',  ( 23.41746824999999887, 6.624999997268815832, 0.000000000000000000 ) ) ;
#1486 = CARTESIAN_POINT ( 'NONE',  ( 10.37757302488624056, 24.77500000273119696, -31.93888565452638417 ) ) ;
#1487 = CARTESIAN_POINT ( 'NONE',  ( 32.50000000000000000, 23.60000000546236976, -10.55989012756945833 ) ) ;
#1488 = CARTESIAN_POINT ( 'NONE',  ( -2.092463501923844636E-15, 71.50000000000001421, -34.17252228774368916 ) ) ;
#1489 = CARTESIAN_POINT ( 'NONE',  ( 0.000000000000000000, 11.99999999999999645, 30.00000000000000000 ) ) ;
#1490 = CARTESIAN_POINT ( 'NONE',  ( -1.778240108872766143E-15, 44.00000000546238255, -32.49999999999999289 ) ) ;
#1491 = CARTESIAN_POINT ( 'NONE',  ( -26.02091320914849959, 53.97173583425732346, 14.97647472619947528 ) ) ;
#1492 = CARTESIAN_POINT ( 'NONE',  ( 27.16883889988624290, 36.17500000273118843, 19.73931689729373673 ) ) ;
#1493 = CARTESIAN_POINT ( 'NONE',  ( 33.58253175000000823, 54.02500000273118985, 10.91162601494192685 ) ) ;
#1494 = CARTESIAN_POINT ( 'NONE',  ( -20.50609665440969209, 31.76562499999999289, 20.50609665441005092 ) ) ;
#1495 = CARTESIAN_POINT ( 'NONE',  ( -18.94512977948575738, 7.924999997268811214, -13.76444248337723231 ) ) ;
#1496 = CARTESIAN_POINT ( 'NONE',  ( -2.092463501923844636E-15, 13.50000000000001066, -34.17252228774368916 ) ) ;
#1497 = CARTESIAN_POINT ( 'NONE',  ( -15.14183272437241889, 16.69999999999999574, -20.84094480462497856 ) ) ;
#1498 = CARTESIAN_POINT ( 'NONE',  ( -13.94119854578892514, 43.93451416574269075, 24.22776226481266448 ) ) ;
#1499 = CARTESIAN_POINT ( 'NONE',  ( -33.58253175000000113, 57.22500000273117848, 10.91162601494193929 ) ) ;
#1500 = CARTESIAN_POINT ( 'NONE',  ( 33.58253175000000113, 48.47500000273118559, -10.91162601494193574 ) ) ;
#1501 = CARTESIAN_POINT ( 'NONE',  ( 23.41746824999999887, 16.62499999726882294, 0.000000000000000000 ) ) ;
#1502 = CARTESIAN_POINT ( 'NONE',  ( 5.147494310547426899, 67.94874572391553613, -32.50000000000000000 ) ) ;
#1503 = DIRECTION ( 'NONE',  ( -1.224646799147353454E-16, 1.000000000000000000, -0.000000000000000000 ) ) ;
#1504 = CARTESIAN_POINT ( 'NONE',  ( 24.22776226481241224, 45.37798583425732346, -13.94119854578936923 ) ) ;
#1505 = CARTESIAN_POINT ( 'NONE',  ( -1.778240108872766143E-15, 38.00000000546237544, -32.49999999999999289 ) ) ;
#1506 = CARTESIAN_POINT ( 'NONE',  ( -10.04305231718579172, 41.60000000000000142, -30.90933677959248982 ) ) ;
#1507 = CARTESIAN_POINT ( 'NONE',  ( 27.16883889988624290, 21.92500000273119198, 19.73931689729373673 ) ) ;
#1508 = CARTESIAN_POINT ( 'NONE',  ( -40.00000000000000711, 52.00000000000000711, 23.09401076758504345 ) ) ;
#1509 = CARTESIAN_POINT ( 'NONE',  ( -15.00000000000000000, 78.25000000546239676, 0.000000000000000000 ) ) ;
#1510 = DIRECTION ( 'NONE',  ( -0.000000000000000000, -1.000000000000000000, -0.000000000000000000 ) ) ;
#1511 = CARTESIAN_POINT ( 'NONE',  ( -0.04044903255044120238, 62.55430583240935505, -30.02300923189239867 ) ) ;
#1512 = CARTESIAN_POINT ( 'NONE',  ( 32.50000000000000000, 39.60000000546234844, -10.55989012756945833 ) ) ;
#1513 = CARTESIAN_POINT ( 'NONE',  ( 9.270509831248425314, 70.95000000546235697, 12.75976212528059683 ) ) ;
#1514 = CARTESIAN_POINT ( 'NONE',  ( -20.75514604977248112, 29.42500000273118133, 28.56700777964554661 ) ) ;
#1515 = CARTESIAN_POINT ( 'NONE',  ( -33.58253175000000113, 65.27500000273117564, -10.91162601494193218 ) ) ;
#1516 = CARTESIAN_POINT ( 'NONE',  ( 6.988114217768294445, 31.19270833333333215, 26.07999730980477437 ) ) ;
#1517 = ORIENTED_EDGE ( 'NONE', *, *, #21552, .F. ) ;
#1518 = CARTESIAN_POINT ( 'NONE',  ( 27.16883889988624290, 65.92500000273119554, 19.73931689729373673 ) ) ;
#1519 = CARTESIAN_POINT ( 'NONE',  ( 7.505752307972854531, 36.63541666666666430, -28.01184896238303423 ) ) ;
#1520 = VECTOR ( 'NONE', #23993, 1000.000000000000000 ) ;
#1521 = FACE_BOUND ( 'NONE', #23198, .T. ) ;
#1522 = VERTEX_POINT ( 'NONE', #29217 ) ;
#1523 = CARTESIAN_POINT ( 'NONE',  ( 26.02091320914851025, 52.25298583425730925, -14.97647472619946463 ) ) ;
#1524 = CARTESIAN_POINT ( 'NONE',  ( 26.09010956794232428, 55.83371500092398065, -6.950374756619718042 ) ) ;
#1525 = CARTESIAN_POINT ( 'NONE',  ( 32.50000000000000000, 9.500000005462375441, -3.980102097228898626E-15 ) ) ;
#1526 = CARTESIAN_POINT ( 'NONE',  ( 15.01150461594643204, 61.98697916666665009, 26.00068869287340334 ) ) ;
#1527 = CARTESIAN_POINT ( 'NONE',  ( 20.08610463437158344, 56.69999999999998153, 27.64615127144129403 ) ) ;
#1528 = CARTESIAN_POINT ( 'NONE',  ( -20.75514604977248823, 39.07500000273119412, -28.56700777964554305 ) ) ;
#1529 = CARTESIAN_POINT ( 'NONE',  ( -26.29305231718578995, 40.70000000546236407, 19.10302069950538595 ) ) ;
#1530 = CARTESIAN_POINT ( 'NONE',  ( 13.91746824999999532, 72.47500000273116427, -4.522059556121118540 ) ) ;
#1531 = CARTESIAN_POINT ( 'NONE',  ( -20.75514604977248823, 26.82500000273117280, -28.56700777964554305 ) ) ;
#1532 = CARTESIAN_POINT ( 'NONE',  ( 7.313012447739250820E-14, 13.24999999453762456, 24.50000000000000000 ) ) ;
#1533 = CARTESIAN_POINT ( 'NONE',  ( -27.16883889988624290, 55.17500000273118133, -19.73931689729374028 ) ) ;
#1534 = CARTESIAN_POINT ( 'NONE',  ( -32.50000000000000000, 34.00000000000001421, 0.000000000000000000 ) ) ;
#1535 = CARTESIAN_POINT ( 'NONE',  ( -32.50000000000000000, 33.90000000000001279, -10.55989012756945478 ) ) ;
#1536 = CARTESIAN_POINT ( 'NONE',  ( 14.47279130897151767, 14.92499999726881299, -19.92008829642072598 ) ) ;
#1537 =( BOUNDED_CURVE ( )  B_SPLINE_CURVE ( 2, ( #4163, #14636, #25096, #1573, #8178, #7420, #7240, #1922, #4332, #30927, #25270, #1743, #4674 ),
 .UNSPECIFIED., .F., .T. ) 
 B_SPLINE_CURVE_WITH_KNOTS ( ( 3, 2, 2, 2, 2, 2, 3 ),
 ( 0.08333333333333334259, 0.08888888888888889228, 0.1000000000000000056, 0.1111111111111111049, 0.1222222222222222182, 0.1333333333333333315, 0.1388888888888888673 ),
 .UNSPECIFIED. ) 
 CURVE ( )  GEOMETRIC_REPRESENTATION_ITEM ( )  RATIONAL_B_SPLINE_CURVE ( ( 0.9755282581475768211, 0.9755282581475768211, 1.000000000000000000, 0.9510565162951535312, 1.000000000000000000, 0.9510565162951535312, 1.000000000000000000, 0.9510565162951535312, 1.000000000000000000, 0.9510565162951535312, 1.000000000000000000, 0.9755282581475768211, 0.9755282581475768211 ) ) 
 REPRESENTATION_ITEM ( '' )  );
#1538 = CARTESIAN_POINT ( 'NONE',  ( -33.58253175000000113, 79.02500000273118985, -10.91162601494193218 ) ) ;
#1539 = CARTESIAN_POINT ( 'NONE',  ( -1.778240108872766143E-15, 63.50000000000000000, -32.49999999999999289 ) ) ;
#1540 = CARTESIAN_POINT ( 'NONE',  ( 6.486482029760648627E-15, 67.87500000273118417, 35.31076352940722529 ) ) ;
#1541 = CARTESIAN_POINT ( 'NONE',  ( 4.635254915624209993, 77.65000000546234560, -14.26584774442730463 ) ) ;
#1542 = ORIENTED_EDGE ( 'NONE', *, *, #10080, .F. ) ;
#1543 = CARTESIAN_POINT ( 'NONE',  ( -24.50000000000000355, 2.649999994537616477, -7.960532557706207157 ) ) ;
#1544 = CARTESIAN_POINT ( 'NONE',  ( 26.06988505166735592, 21.74517333425730925, 7.025853678916393896 ) ) ;
#1545 = CARTESIAN_POINT ( 'NONE',  ( 10.04305231718578817, 47.39999999999999858, -30.90933677959249337 ) ) ;
#1546 = CARTESIAN_POINT ( 'NONE',  ( -20.75514604977248112, 43.42500000273117422, 28.56700777964554661 ) ) ;
#1547 = CARTESIAN_POINT ( 'NONE',  ( -33.58253175000000113, 5.275000002731187188, -10.91162601494193218 ) ) ;
#1548 = CARTESIAN_POINT ( 'NONE',  ( -20.75514604977248112, 57.67500000273118843, 28.56700777964554661 ) ) ;
#1549 = CARTESIAN_POINT ( 'NONE',  ( 27.95245687107223276, 54.53906249999999289, -2.463307335887066074E-13 ) ) ;
#1550 = CARTESIAN_POINT ( 'NONE',  ( -30.02300923189239867, 43.94569416759065206, -0.04044903254991731589 ) ) ;
#1551 = CARTESIAN_POINT ( 'NONE',  ( -26.02091320914878025, 34.48138916574268364, -14.97647472619899389 ) ) ;
#1552 = CARTESIAN_POINT ( 'NONE',  ( -26.29305231718579350, 58.30000000546238681, -19.10302069950537884 ) ) ;
#1553 = CARTESIAN_POINT ( 'NONE',  ( -8.960552108402742093E-16, 80.87500000273116996, -14.63369212191046387 ) ) ;
#1554 = CARTESIAN_POINT ( 'NONE',  ( 26.06988505166722803, 66.70795166574268364, -7.025853678916862854 ) ) ;
#1555 = CARTESIAN_POINT ( 'NONE',  ( 0.000000000000000000, 80.00000000000001421, -32.50000000000000000 ) ) ;
#1556 = CARTESIAN_POINT ( 'NONE',  ( 28.01184896238290278, 13.14583333333332860, -7.505752307973347470 ) ) ;
#1557 = CARTESIAN_POINT ( 'NONE',  ( -33.58253175000000113, 41.47500000273117138, 10.91162601494193929 ) ) ;
#1558 = CARTESIAN_POINT ( 'NONE',  ( 23.41746824999999887, 3.124999997268812280, 0.000000000000000000 ) ) ;
#1559 = VERTEX_POINT ( 'NONE', #5551 ) ;
#1560 = CARTESIAN_POINT ( 'NONE',  ( -26.29305231718579350, 28.30000000546238681, -19.10302069950537884 ) ) ;
#1561 = EDGE_LOOP ( 'NONE', ( #16202, #13374, #12638, #10013 ) ) ;
#1562 = CARTESIAN_POINT ( 'NONE',  ( 26.00068869287340334, 33.62760416666665719, -15.01150461594642316 ) ) ;
#1563 = CARTESIAN_POINT ( 'NONE',  ( -26.29305231718579350, 60.30000000546237260, -19.10302069950537884 ) ) ;
#1564 = ORIENTED_EDGE ( 'NONE', *, *, #32911, .F. ) ;
#1565 = CARTESIAN_POINT ( 'NONE',  ( -10.04305231718579172, 74.10000000546237686, -30.90933677959248982 ) ) ;
#1566 = CARTESIAN_POINT ( 'NONE',  ( 33.58253175000000113, 50.22500000273118559, -10.91162601494193751 ) ) ;
#1567 = CARTESIAN_POINT ( 'NONE',  ( -14.47279130897151589, 15.32499999726880269, -19.92008829642072598 ) ) ;
#1568 = CARTESIAN_POINT ( 'NONE',  ( 20.50609665440969565, 64.42187499999998579, -20.50609665441004736 ) ) ;
#1569 = CARTESIAN_POINT ( 'NONE',  ( -32.50000000000000000, 10.40000000546237935, -10.55989012756945478 ) ) ;
#1570 = CARTESIAN_POINT ( 'NONE',  ( 27.16883889988624290, 65.92500000273119554, 19.73931689729373673 ) ) ;
#1571 = CARTESIAN_POINT ( 'NONE',  ( 18.94512977948576093, 13.32499999726882756, -13.76444248337722875 ) ) ;
#1572 = CARTESIAN_POINT ( 'NONE',  ( -10.04305231718578462, 54.40000000000000568, 30.90933677959249337 ) ) ;
#1573 = CARTESIAN_POINT ( 'NONE',  ( 15.14183272437242067, 1.700000000000004396, 20.84094480462498211 ) ) ;
#1574 = CARTESIAN_POINT ( 'NONE',  ( -20.75514604977248112, 19.67500000273119909, 28.56700777964554661 ) ) ;
#1575 = DIRECTION ( 'NONE',  ( 0.000000000000000000, -1.000000000000000000, 0.000000000000000000 ) ) ;
#1576 = CARTESIAN_POINT ( 'NONE',  ( -24.22776226481266448, 20.73138916574268720, -13.94119854578892514 ) ) ;
#1577 = CARTESIAN_POINT ( 'NONE',  ( 11.25946833292375793, 71.67500000273119554, 8.180482586598731842 ) ) ;
#1578 = CARTESIAN_POINT ( 'NONE',  ( -7.570916362186215665, 13.39999999999999503, 23.30088464923126423 ) ) ;
#1579 = CARTESIAN_POINT ( 'NONE',  ( -20.08610463437156923, 22.29999999999999361, 27.64615127144130113 ) ) ;
#1580 = CARTESIAN_POINT ( 'NONE',  ( 10.04305231718579705, 6.599999999999994316, 30.90933677959248982 ) ) ;
#1581 = VERTEX_POINT ( 'NONE', #10534 ) ;
#1582 = CARTESIAN_POINT ( 'NONE',  ( -18.94512977948576093, 4.324999997268818674, 13.76444248337722698 ) ) ;
#1583 = CARTESIAN_POINT ( 'NONE',  ( -13.91746824999999532, 70.97500000273116427, 4.522059556121122093 ) ) ;
#1584 = CARTESIAN_POINT ( 'NONE',  ( 19.09188309203661049, 50.67187500000000000, -19.09188309203694445 ) ) ;
#1585 = ADVANCED_FACE ( 'NONE', ( #13622 ), #23917, .F. ) ;
#1586 = CARTESIAN_POINT ( 'NONE',  ( -27.16883889988623935, 63.32500000273120833, 19.73931689729374739 ) ) ;
#1587 = CARTESIAN_POINT ( 'NONE',  ( -33.58253175000000113, 25.37500000273119838, 0.000000000000000000 ) ) ;
#1588 = CARTESIAN_POINT ( 'NONE',  ( -27.16883889988623935, 11.57500000273119234, 19.73931689729374739 ) ) ;
#1589 = CARTESIAN_POINT ( 'NONE',  ( 28.00173670424549499, 14.87017333425730747, 7.543491769121417612 ) ) ;
#1590 = CARTESIAN_POINT ( 'NONE',  ( 20.50609665440969565, 60.98437499999999289, -20.50609665441004736 ) ) ;
#1591 = CARTESIAN_POINT ( 'NONE',  ( 8.601468415847520532, 74.07500000273120122, 11.83890561707634603 ) ) ;
#1592 = CARTESIAN_POINT ( 'NONE',  ( 32.50000000000000711, 46.90000000000000568, 10.55989012756945122 ) ) ;
#1593 = CARTESIAN_POINT ( 'NONE',  ( -2.162160676586882350E-15, 52.62500000273117706, -35.31076352940722529 ) ) ;
#1594 = CARTESIAN_POINT ( 'NONE',  ( -14.47279130897152122, 5.924999997268808549, 19.92008829642072243 ) ) ;
#1595 = ADVANCED_FACE ( 'NONE', ( #555 ), #27605, .F. ) ;
#1596 = PRODUCT_DEFINITION_SHAPE ( 'NONE', 'NONE',  #33994 ) ;
#1597 = CARTESIAN_POINT ( 'NONE',  ( 4.635254915624212657, 78.60000000000000853, 14.26584774442730286 ) ) ;
#1598 = ORIENTED_EDGE ( 'NONE', *, *, #25617, .F. ) ;
#1599 = CARTESIAN_POINT ( 'NONE',  ( 27.16883889988624290, 58.17500000273119554, 19.73931689729373673 ) ) ;
#1600 = DIRECTION ( 'NONE',  ( 1.000000000000000000, 0.000000000000000000, -0.000000000000000000 ) ) ;
#1601 = CARTESIAN_POINT ( 'NONE',  ( 18.94512977948576093, 10.82499999726882578, -13.76444248337722875 ) ) ;
#1602 = CARTESIAN_POINT ( 'NONE',  ( -26.09010956794232428, 36.92746500092395934, 6.950374756619732253 ) ) ;
#1603 = VERTEX_POINT ( 'NONE', #10701 ) ;
#1604 = CARTESIAN_POINT ( 'NONE',  ( -10.37757302488623701, 27.52500000273118275, 31.93888565452638417 ) ) ;
#1605 = VERTEX_POINT ( 'NONE', #13450 ) ;
#1606 = CARTESIAN_POINT ( 'NONE',  ( 15.01150461594596308, 57.40364583333333570, -26.00068869287367335 ) ) ;
#1607 = CARTESIAN_POINT ( 'NONE',  ( -20.75514604977248823, 61.07500000273119412, -28.56700777964554305 ) ) ;
#1608 = DIRECTION ( 'NONE',  ( -1.224646799147353454E-16, 1.000000000000000000, -0.000000000000000000 ) ) ;
#1609 = CARTESIAN_POINT ( 'NONE',  ( 33.58253175000000823, 70.02500000273121827, 10.91162601494192863 ) ) ;
#1610 = CARTESIAN_POINT ( 'NONE',  ( 30.02300923189239512, 27.03906250000000000, -2.619432448724977703E-13 ) ) ;
#1611 = CARTESIAN_POINT ( 'NONE',  ( 24.50000000000000355, 14.09999999999999254, -7.960532557706203605 ) ) ;
#1612 = CARTESIAN_POINT ( 'NONE',  ( -10.11000150615021909, -45.00000000000000000, 0.000000000000000000 ) ) ;
#1613 = CARTESIAN_POINT ( 'NONE',  ( -33.58253175000000113, 9.225000002731178483, 10.91162601494193929 ) ) ;
#1614 = CARTESIAN_POINT ( 'NONE',  ( -4.300734207923755825, 71.27500000273117564, 13.23629886949340673 ) ) ;
#1615 = CARTESIAN_POINT ( 'NONE',  ( 20.53372385742108008, 53.53086833240935505, 20.47846945139866648 ) ) ;
#1616 = CARTESIAN_POINT ( 'NONE',  ( 26.29305231718578995, 37.20000000000000995, -19.10302069950538240 ) ) ;
#1617 = CARTESIAN_POINT ( 'NONE',  ( 2.740863092043355209E-13, 55.39843749999999289, 30.02300923189239867 ) ) ;
#1618 = CARTESIAN_POINT ( 'NONE',  ( 1.555960095263670572E-15, 14.24999999453762278, -24.50000000000000000 ) ) ;
#1619 = CARTESIAN_POINT ( 'NONE',  ( 32.50000000000000000, 61.50000000546238255, -3.980102097228898626E-15 ) ) ;
#1620 = CARTESIAN_POINT ( 'NONE',  ( 7.570916362186213000, 4.149999994537633796, -23.30088464923126423 ) ) ;
#1621 = CARTESIAN_POINT ( 'NONE',  ( 4.635254915624212657, 76.85000000546237686, 14.26584774442730286 ) ) ;
#1622 = CARTESIAN_POINT ( 'NONE',  ( -24.22776226481266448, 68.85638916574269786, -13.94119854578892514 ) ) ;
#1623 = CARTESIAN_POINT ( 'NONE',  ( -27.16883889988624290, 38.92500000273118843, -19.73931689729374028 ) ) ;
#1624 = CARTESIAN_POINT ( 'NONE',  ( 8.601468415847516980, 76.17500000273115290, -11.83890561707634781 ) ) ;
#1625 = CARTESIAN_POINT ( 'NONE',  ( 20.75514604977249178, 40.07500000273118701, 28.56700777964553950 ) ) ;
#1626 = CARTESIAN_POINT ( 'NONE',  ( 27.16883889988623935, 30.57500000273119412, -19.73931689729374384 ) ) ;
#1627 = CARTESIAN_POINT ( 'NONE',  ( 7.313012447739250820E-14, 17.24999999453762456, 24.50000000000000000 ) ) ;
#1628 = CARTESIAN_POINT ( 'NONE',  ( -10.04305231718578462, 8.900000005462372243, 30.90933677959249337 ) ) ;
#1629 = CARTESIAN_POINT ( 'NONE',  ( 20.08610463437157279, 33.29999999999999716, -27.64615127144129758 ) ) ;
#1630 = CARTESIAN_POINT ( 'NONE',  ( 20.08610463437157279, 69.29999999999996874, -27.64615127144129758 ) ) ;
#1631 = CARTESIAN_POINT ( 'NONE',  ( -18.94512977948576093, 9.824999997268824004, 13.76444248337722698 ) ) ;
#1632 = CARTESIAN_POINT ( 'NONE',  ( 28.00173670424535644, 25.45795166574268364, -7.543491769121920321 ) ) ;
#1633 =( BOUNDED_CURVE ( )  B_SPLINE_CURVE ( 2, ( #18273, #5216, #2647, #23584, #49, #18945, #24413 ),
 .UNSPECIFIED., .F., .T. ) 
 B_SPLINE_CURVE_WITH_KNOTS ( ( 3, 2, 2, 3 ),
 ( 0.9499999999999999556, 0.9599999999999999645, 0.9799999999999999822, 1.000000000000000000 ),
 .UNSPECIFIED. ) 
 CURVE ( )  GEOMETRIC_REPRESENTATION_ITEM ( )  RATIONAL_B_SPLINE_CURVE ( ( 0.9755282581475768211, 0.9755282581475768211, 1.000000000000000000, 0.9510565162951535312, 1.000000000000000000, 0.9510565162951535312, 1.000000000000000000 ) ) 
 REPRESENTATION_ITEM ( '' )  );
#1634 = CARTESIAN_POINT ( 'NONE',  ( -14.47279130897152122, 2.424999997268802332, 19.92008829642072243 ) ) ;
#1635 = CARTESIAN_POINT ( 'NONE',  ( -0.04044903255042732459, 38.49180583240935505, -27.95245687107223986 ) ) ;
#1636 = LINE ( 'NONE', #9362, #17269 ) ;
#1637 =( BOUNDED_CURVE ( )  B_SPLINE_CURVE ( 2, ( #30999, #31340, #15055, #10413, #9723, #7497, #7662 ),
 .UNSPECIFIED., .F., .T. ) 
 B_SPLINE_CURVE_WITH_KNOTS ( ( 3, 2, 2, 3 ),
 ( 0.000000000000000000, 0.002564102564102564100, 0.005128205128205128201, 0.006410256410256410901 ),
 .UNSPECIFIED. ) 
 CURVE ( )  GEOMETRIC_REPRESENTATION_ITEM ( )  RATIONAL_B_SPLINE_CURVE ( ( 1.000000000000000000, 0.9510565162951535312, 1.000000000000000000, 0.9510565162951535312, 1.000000000000000000, 0.9755282581475768211, 0.9755282581475768211 ) ) 
 REPRESENTATION_ITEM ( '' )  );
#1638 = CARTESIAN_POINT ( 'NONE',  ( -20.75514604977248112, 13.42500000273119198, 28.56700777964554661 ) ) ;
#1639 = CARTESIAN_POINT ( 'NONE',  ( 14.47279130897151589, 12.82499999726882400, 19.92008829642072953 ) ) ;
#1640 = CARTESIAN_POINT ( 'NONE',  ( 24.20753774853731244, 61.12760416666665719, -13.97622843553632599 ) ) ;
#1641 = EDGE_LOOP ( 'NONE', ( #19114, #3299, #32177, #24096 ) ) ;
#1642 = CARTESIAN_POINT ( 'NONE',  ( 20.75514604977248467, 50.42500000273118843, -28.56700777964554305 ) ) ;
#1643 = CARTESIAN_POINT ( 'NONE',  ( 33.58253175000000113, 20.47500000273120335, -10.91162601494193751 ) ) ;
#1644 = EDGE_CURVE ( 'NONE', #17496, #30053, #15696, .T. ) ;
#1645 = ORIENTED_EDGE ( 'NONE', *, *, #18742, .F. ) ;
#1646 = CARTESIAN_POINT ( 'NONE',  ( 26.00068869287340334, 37.06510416666666430, -15.01150461594642316 ) ) ;
#1647 = CARTESIAN_POINT ( 'NONE',  ( 15.04653450569292872, 34.77902750092397355, -25.98046417659857710 ) ) ;
#1648 = CARTESIAN_POINT ( 'NONE',  ( 1.555960095263670572E-15, 8.249999994537619230, -24.50000000000000000 ) ) ;
#1649 = CARTESIAN_POINT ( 'NONE',  ( 24.50000000000000355, 13.84999999453764197, -7.960532557706203605 ) ) ;
#1650 = ADVANCED_FACE ( 'NONE', ( #31958 ), #29048, .T. ) ;
#1651 = CARTESIAN_POINT ( 'NONE',  ( -7.236395654485763274, 10.02499999726880198, 22.27133577429736633 ) ) ;
#1652 = CARTESIAN_POINT ( 'NONE',  ( 33.58253175000000113, 22.37500000273118417, -4.112674001490185761E-15 ) ) ;
#1653 = CARTESIAN_POINT ( 'NONE',  ( -32.50000000000000000, 26.60000000546239107, 10.55989012756946366 ) ) ;
#1654 = CARTESIAN_POINT ( 'NONE',  ( 10.04305231718578817, 69.40000000000001990, -30.90933677959249337 ) ) ;
#1655 = CARTESIAN_POINT ( 'NONE',  ( 26.29305231718579350, 47.30000000546235839, 19.10302069950537529 ) ) ;
#1656 = CARTESIAN_POINT ( 'NONE',  ( -31.04172217648553556, 66.99999999999998579, -12.81397374188210136 ) ) ;
#1657 = CARTESIAN_POINT ( 'NONE',  ( 25.98046417659858420, 59.70090250092397355, 15.04653450569292872 ) ) ;
#1658 = CARTESIAN_POINT ( 'NONE',  ( 20.75514604977248467, 34.67500000273118843, -28.56700777964554305 ) ) ;
#1659 = CARTESIAN_POINT ( 'NONE',  ( 26.29305231718579350, 43.30000000546238681, 19.10302069950537529 ) ) ;
#1660 = CARTESIAN_POINT ( 'NONE',  ( 30.02300923189239867, 27.03906250000000000, -2.619432448724978208E-13 ) ) ;
#1661 =( LENGTH_UNIT ( ) NAMED_UNIT ( * ) SI_UNIT ( .MILLI., .METRE. ) );
#1662 = CARTESIAN_POINT ( 'NONE',  ( 18.94512977948575738, 12.92499999726881654, 13.76444248337723408 ) ) ;
#1663 = CARTESIAN_POINT ( 'NONE',  ( 6.277390505771533514E-15, 12.49999999999998401, 34.17252228774368916 ) ) ;
#1664 = CARTESIAN_POINT ( 'NONE',  ( -26.29305231718578995, 52.19999999999999574, 19.10302069950538595 ) ) ;
#1665 = CARTESIAN_POINT ( 'NONE',  ( 24.18731323226221974, 45.93972249907602645, -14.01125832528328985 ) ) ;
#1666 = CARTESIAN_POINT ( 'NONE',  ( -10.37757302488623701, 55.52500000273119696, 31.93888565452638417 ) ) ;
#1667 = CARTESIAN_POINT ( 'NONE',  ( -20.75514604977248823, 61.07500000273119412, -28.56700777964554305 ) ) ;
#1668 = CARTESIAN_POINT ( 'NONE',  ( 20.75514604977249178, 48.07500000273120122, 28.56700777964553950 ) ) ;
#1669 = CARTESIAN_POINT ( 'NONE',  ( 18.94512977948576093, 14.82499999726880091, -13.76444248337722875 ) ) ;
#1670 = CARTESIAN_POINT ( 'NONE',  ( 32.50000000000000711, 67.40000000546240244, 10.55989012756945122 ) ) ;
#1671 = CARTESIAN_POINT ( 'NONE',  ( 5.779280353836490358E-15, 50.50000000000000000, 32.49999999999999289 ) ) ;
#1672 = CARTESIAN_POINT ( 'NONE',  ( -6.950374756619716266, 51.53684000092397355, -26.09010956794232428 ) ) ;
#1673 = CARTESIAN_POINT ( 'NONE',  ( -4.223320258572819786E-15, 5.249999994537629888, 24.50000000000000000 ) ) ;
#1674 = DIRECTION ( 'NONE',  ( -1.000000000000000000, -1.416100796715761110E-16, 0.000000000000000000 ) ) ;
#1675 = CARTESIAN_POINT ( 'NONE',  ( -33.58253175000000113, 21.12500000273119483, 0.000000000000000000 ) ) ;
#1676 = CARTESIAN_POINT ( 'NONE',  ( -1.053607264507113999E-13, 63.00000000546238255, 32.50000000000000711 ) ) ;
#1677 = CARTESIAN_POINT ( 'NONE',  ( -2.165007332552593587E-13, 52.50000000000000711, 32.50000000000000000 ) ) ;
#1678 = CARTESIAN_POINT ( 'NONE',  ( 10.04305231718579705, 41.10000000546237686, 30.90933677959248982 ) ) ;
#1679 = CARTESIAN_POINT ( 'NONE',  ( -7.468012846824272799, 67.85378499907602645, 28.02196122052058413 ) ) ;
#1680 = CARTESIAN_POINT ( 'NONE',  ( 26.29305231718578995, 43.70000000546238539, -19.10302069950538240 ) ) ;
#1681 = CARTESIAN_POINT ( 'NONE',  ( -10.04305231718579172, 60.10000000546239818, -30.90933677959248982 ) ) ;
#1682 = CARTESIAN_POINT ( 'NONE',  ( 27.16883889988624290, 29.92500000273118488, 19.73931689729373673 ) ) ;
#1683 = CARTESIAN_POINT ( 'NONE',  ( -10.37757302488623701, 65.77500000273118985, 31.93888565452638417 ) ) ;
#1684 = AXIS2_PLACEMENT_3D ( 'NONE', #15585, #25863, #20563 ) ;
#1685 = CARTESIAN_POINT ( 'NONE',  ( -19.09188309203660694, 31.76562499999999289, 19.09188309203694800 ) ) ;
#1686 = VERTEX_POINT ( 'NONE', #26487 ) ;
#1687 = CARTESIAN_POINT ( 'NONE',  ( -10.37757302488624411, 68.72500000273116427, -31.93888565452638417 ) ) ;
#1688 = CARTESIAN_POINT ( 'NONE',  ( 15.01150461594596308, 40.21614583333332860, -26.00068869287367335 ) ) ;
#1689 = EDGE_CURVE ( 'NONE', #7405, #23066, #10874, .T. ) ;
#1690 = VERTEX_POINT ( 'NONE', #10366 ) ;
#1691 = CARTESIAN_POINT ( 'NONE',  ( 15.04653450569292872, 58.84152750092397355, -25.98046417659857710 ) ) ;
#1692 = CARTESIAN_POINT ( 'NONE',  ( -19.06425588902591173, 65.00038166759063074, -19.11951029504763611 ) ) ;
#1693 = CARTESIAN_POINT ( 'NONE',  ( -2.162160676586881955E-15, 12.62500000273118772, -35.31076352940723240 ) ) ;
#1694 = EDGE_CURVE ( 'NONE', #7536, #19359, #32051, .T. ) ;
#1695 = CARTESIAN_POINT ( 'NONE',  ( 26.00068869287367335, 58.26302083333332149, 15.01150461594596308 ) ) ;
#1696 = CARTESIAN_POINT ( 'NONE',  ( -26.29305231718578995, 46.19999999999998863, 19.10302069950538595 ) ) ;
#1697 = CARTESIAN_POINT ( 'NONE',  ( 20.75514604977248467, 38.67500000273117422, -28.56700777964554305 ) ) ;
#1698 = CARTESIAN_POINT ( 'NONE',  ( -20.08610463437157989, 42.20000000546239249, -27.64615127144129758 ) ) ;
#1699 = CARTESIAN_POINT ( 'NONE',  ( 4.300734207923757602, 72.77500000273118985, -13.23629886949340673 ) ) ;
#1700 = CARTESIAN_POINT ( 'NONE',  ( 33.58253175000000823, 30.02500000273118985, 10.91162601494192863 ) ) ;
#1701 = CARTESIAN_POINT ( 'NONE',  ( -33.58253175000000113, 53.37500000273118417, 0.000000000000000000 ) ) ;
#1702 = CARTESIAN_POINT ( 'NONE',  ( -10.04305231718578462, 36.39999999999999858, 30.90933677959249337 ) ) ;
#1703 = CARTESIAN_POINT ( 'NONE',  ( 32.50000000000000000, 31.00000000000000000, -3.980102097228898626E-15 ) ) ;
#1704 = CARTESIAN_POINT ( 'NONE',  ( 24.50000000000000355, 0.09999999999999684142, -7.960532557706203605 ) ) ;
#1705 = CARTESIAN_POINT ( 'NONE',  ( -10.37757302488623701, 77.52500000273118985, 31.93888565452638417 ) ) ;
#1706 = CARTESIAN_POINT ( 'NONE',  ( 5.779280353836490358E-15, 62.50000000000000000, 32.49999999999999289 ) ) ;
#1707 = CIRCLE ( 'NONE', #20926, 10.18398033115917656 ) ;
#1708 = CARTESIAN_POINT ( 'NONE',  ( -32.50000000000000000, 37.89999999999999858, -10.55989012756945300 ) ) ;
#1709 = CARTESIAN_POINT ( 'NONE',  ( -20.75514604977248823, 67.07500000273118701, -28.56700777964554305 ) ) ;
#1710 = CARTESIAN_POINT ( 'NONE',  ( 12.13525491562421088, 77.05000000546242234, 8.816778784387095058 ) ) ;
#1711 = ORIENTED_EDGE ( 'NONE', *, *, #805, .F. ) ;
#1712 = CARTESIAN_POINT ( 'NONE',  ( -33.58253175000000113, 19.12500000273118062, 0.000000000000000000 ) ) ;
#1713 = CARTESIAN_POINT ( 'NONE',  ( 19.82091636218621034, 11.54999999453762349, 14.40073868116559730 ) ) ;
#1714 = CARTESIAN_POINT ( 'NONE',  ( -14.01125832528285109, 22.74777750092397355, 24.18731323226248264 ) ) ;
#1715 = CARTESIAN_POINT ( 'NONE',  ( 0.000000000000000000, 80.00000000000001421, -32.50000000000000000 ) ) ;
#1716 = CARTESIAN_POINT ( 'NONE',  ( 20.75514604977248467, 42.42500000273117422, -28.56700777964554305 ) ) ;
#1717 = CARTESIAN_POINT ( 'NONE',  ( -10.37757302488624411, 6.975000002731198911, -31.93888565452638417 ) ) ;
#1718 = CARTESIAN_POINT ( 'NONE',  ( -2.162160676586882350E-15, 52.87500000273119838, -35.31076352940722529 ) ) ;
#1719 = CARTESIAN_POINT ( 'NONE',  ( -30.02300923189239867, 47.38319416759065206, -0.04044903254991731589 ) ) ;
#1720 = CARTESIAN_POINT ( 'NONE',  ( 7.543491769121922985, 40.06732666574268364, 28.00173670424535644 ) ) ;
#1721 = CARTESIAN_POINT ( 'NONE',  ( -32.50000000000000000, 58.50000000546238965, 0.000000000000000000 ) ) ;
#1722 = CARTESIAN_POINT ( 'NONE',  ( 4.300734207923757602, 80.77500000273118985, -13.23629886949340673 ) ) ;
#1723 = CARTESIAN_POINT ( 'NONE',  ( 26.09010956794244507, 66.99440999907601224, 6.950374756619249084 ) ) ;
#1724 = LINE ( 'NONE', #12204, #13775 ) ;
#1725 = CARTESIAN_POINT ( 'NONE',  ( 6.277390505771533514E-15, 77.00000000546235412, 34.17252228774368916 ) ) ;
#1726 = CARTESIAN_POINT ( 'NONE',  ( 28.01184896238290278, 16.58333333333333215, -7.505752307973347470 ) ) ;
#1727 = CARTESIAN_POINT ( 'NONE',  ( 6.486482029760649416E-15, 41.87500000273119127, 35.31076352940723240 ) ) ;
#1728 = CARTESIAN_POINT ( 'NONE',  ( -7.236395654485757944, 5.724999997268803931, -22.27133577429736988 ) ) ;
#1729 = VERTEX_POINT ( 'NONE', #22178 ) ;
#1730 = CARTESIAN_POINT ( 'NONE',  ( 20.75514604977249178, 72.07500000273120122, 28.56700777964553950 ) ) ;
#1731 = CARTESIAN_POINT ( 'NONE',  ( -20.08610463437156923, 32.80000000546237260, 27.64615127144130113 ) ) ;
#1732 = VERTEX_POINT ( 'NONE', #14281 ) ;
#1733 = CARTESIAN_POINT ( 'NONE',  ( -15.01150461594595775, 31.62239583333332860, 26.00068869287368756 ) ) ;
#1734 = CARTESIAN_POINT ( 'NONE',  ( 20.08610463437157279, 65.80000000546237970, -27.64615127144129758 ) ) ;
#1735 = ORIENTED_EDGE ( 'NONE', *, *, #7267, .T. ) ;
#1736 =( BOUNDED_CURVE ( )  B_SPLINE_CURVE ( 2, ( #33821, #10315, #4815, #31068, #18047, #4988, #13398, #669, #6161, #27100, #3427, #21959, #16645 ),
 .UNSPECIFIED., .F., .T. ) 
 B_SPLINE_CURVE_WITH_KNOTS ( ( 3, 2, 2, 2, 2, 2, 3 ),
 ( 0.2884615384615384914, 0.2897435897435897689, 0.2923076923076923239, 0.2948717948717948789, 0.2974358974358974339, 0.2999999999999999889, 0.3012820512820512664 ),
 .UNSPECIFIED. ) 
 CURVE ( )  GEOMETRIC_REPRESENTATION_ITEM ( )  RATIONAL_B_SPLINE_CURVE ( ( 0.9755282581475768211, 0.9755282581475772652, 1.000000000000000000, 0.9510565162951535312, 1.000000000000000000, 0.9510565162951535312, 1.000000000000000000, 0.9510565162951535312, 1.000000000000000000, 0.9510565162951535312, 1.000000000000000000, 0.9755282581475768211, 0.9755282581475768211 ) ) 
 REPRESENTATION_ITEM ( '' )  );
#1737 = CARTESIAN_POINT ( 'NONE',  ( -27.16883889988623935, 47.32500000273117990, 19.73931689729374739 ) ) ;
#1738 = CARTESIAN_POINT ( 'NONE',  ( 5.779280353836490358E-15, 55.00000000546238965, 32.49999999999999289 ) ) ;
#1739 = CARTESIAN_POINT ( 'NONE',  ( -10.04305231718579172, 6.100000005462375086, -30.90933677959248982 ) ) ;
#1740 = CARTESIAN_POINT ( 'NONE',  ( -10.37757302488624411, 64.72500000273119269, -31.93888565452638417 ) ) ;
#1741 = CARTESIAN_POINT ( 'NONE',  ( -20.50609665441004736, 15.43749999999999645, -20.50609665440969565 ) ) ;
#1742 = CARTESIAN_POINT ( 'NONE',  ( -20.08610463437156923, 56.29999999999999716, 27.64615127144130113 ) ) ;
#1743 = CARTESIAN_POINT ( 'NONE',  ( 3.880418787951150694, 2.448745718453165132, -24.49999999999999645 ) ) ;
#1744 = CARTESIAN_POINT ( 'NONE',  ( -27.16883889988624290, 19.17500000273120264, -19.73931689729374028 ) ) ;
#1745 = CARTESIAN_POINT ( 'NONE',  ( 3.880418787951141812, 0.4487457184531665200, -24.50000000000000000 ) ) ;
#1746 = CARTESIAN_POINT ( 'NONE',  ( 27.95245687107223276, 29.03868083240935505, -0.04044903255042905932 ) ) ;
#1747 = CARTESIAN_POINT ( 'NONE',  ( 13.91746824999999887, 71.87500000273119838, -1.704398294459741270E-15 ) ) ;
#1748 = CARTESIAN_POINT ( 'NONE',  ( 19.82091636218621389, 8.200000000000013500, -14.40073868116559197 ) ) ;
#1749 = DIRECTION ( 'NONE',  ( 0.8660254037844385966, 0.000000000000000000, 0.5000000000000000000 ) ) ;
#1750 = CARTESIAN_POINT ( 'NONE',  ( -20.08610463437157989, 5.699999999999993960, -27.64615127144129758 ) ) ;
#1751 = ORIENTED_EDGE ( 'NONE', *, *, #28129, .T. ) ;
#1752 = CARTESIAN_POINT ( 'NONE',  ( 23.41746824999999887, 13.12499999726882116, 0.000000000000000000 ) ) ;
#1753 = CARTESIAN_POINT ( 'NONE',  ( 23.41746824999999887, 0.6249999972688102812, 0.000000000000000000 ) ) ;
#1754 = CARTESIAN_POINT ( 'NONE',  ( -2.428612866367529427E-13, 46.80468750000000000, -27.95245687107222921 ) ) ;
#1755 = CARTESIAN_POINT ( 'NONE',  ( 33.58253175000000113, 60.12500000273117706, -4.112674001490185761E-15 ) ) ;
#1756 = CARTESIAN_POINT ( 'NONE',  ( -33.58253175000000113, 21.37500000273119483, 0.000000000000000000 ) ) ;
#1757 = CARTESIAN_POINT ( 'NONE',  ( -27.16883889988624290, 11.17500000273118133, -19.73931689729374028 ) ) ;
#1758 = CARTESIAN_POINT ( 'NONE',  ( 33.58253175000000113, 4.375000002731193938, -4.112674001490185761E-15 ) ) ;
#1759 = CARTESIAN_POINT ( 'NONE',  ( 7.543491769121427382, 20.88579833425730925, -28.00173670424548433 ) ) ;
#1760 = CARTESIAN_POINT ( 'NONE',  ( -28.01184896238290278, 59.55208333333332149, 7.505752307973363457 ) ) ;
#1761 = CARTESIAN_POINT ( 'NONE',  ( -27.16883889988624290, 2.925000002731187543, -19.73931689729374028 ) ) ;
#1762 = CARTESIAN_POINT ( 'NONE',  ( 10.04305231718579705, 68.59999999999999432, 30.90933677959248982 ) ) ;
#1763 = CARTESIAN_POINT ( 'NONE',  ( -10.04305231718579172, 41.60000000000000853, -30.90933677959248982 ) ) ;
#1764 = CARTESIAN_POINT ( 'NONE',  ( 20.75514604977249178, 45.82500000273118701, 28.56700777964553950 ) ) ;
#1765 = CARTESIAN_POINT ( 'NONE',  ( 18.94512977948576093, 0.8249999972688160099, -13.76444248337722875 ) ) ;
#1766 = CARTESIAN_POINT ( 'NONE',  ( 2.757615341152813402E-15, -45.51763809020504681, 0.000000000000000000 ) ) ;
#1767 = EDGE_LOOP ( 'NONE', ( #11128, #21845, #19685, #258 ) ) ;
#1768 = CARTESIAN_POINT ( 'NONE',  ( 27.16883889988624290, 60.17500000273119554, 19.73931689729373673 ) ) ;
#1769 = PLANE ( 'NONE',  #26702 ) ;
#1770 = AXIS2_PLACEMENT_3D ( 'NONE', #2717, #20916, #25712 ) ;
#1771 = CARTESIAN_POINT ( 'NONE',  ( -4.523095164977116484E-15, 10.12499999726881938, 24.62258325217400312 ) ) ;
#1772 = CARTESIAN_POINT ( 'NONE',  ( 13.94119854578937812, 32.48736083425731636, 24.22776226481240514 ) ) ;
#1773 = ORIENTED_EDGE ( 'NONE', *, *, #8175, .T. ) ;
#1774 = CARTESIAN_POINT ( 'NONE',  ( 10.37757302488624056, 28.52500000273118630, -31.93888565452638417 ) ) ;
#1775 = CIRCLE ( 'NONE', #13857, 26.50000000000000355 ) ;
#1776 = CYLINDRICAL_SURFACE ( 'NONE', #28573, 16.50000000000002842 ) ;
#1777 =( BOUNDED_CURVE ( )  B_SPLINE_CURVE ( 2, ( #17992, #22606, #25698, #33235, #17472, #20741, #4929, #9734, #12829, #31011, #15410, #23301, #7157 ),
 .UNSPECIFIED., .F., .T. ) 
 B_SPLINE_CURVE_WITH_KNOTS ( ( 3, 2, 2, 2, 2, 2, 3 ),
 ( 0.5833333333333333703, 0.5846153846153846478, 0.5871794871794872028, 0.5897435897435897578, 0.5923076923076923128, 0.5948717948717948678, 0.5961538461538461453 ),
 .UNSPECIFIED. ) 
 CURVE ( )  GEOMETRIC_REPRESENTATION_ITEM ( )  RATIONAL_B_SPLINE_CURVE ( ( 0.9755282581475768211, 0.9755282581475768211, 1.000000000000000000, 0.9510565162951535312, 1.000000000000000000, 0.9510565162951535312, 1.000000000000000000, 0.9510565162951535312, 1.000000000000000000, 0.9510565162951535312, 1.000000000000000000, 0.9755282581475768211, 0.9755282581475768211 ) ) 
 REPRESENTATION_ITEM ( '' )  );
#1778 = ORIENTED_EDGE ( 'NONE', *, *, #3857, .T. ) ;
#1779 = CARTESIAN_POINT ( 'NONE',  ( 5.147494310547408247, 69.05125428700922896, 32.50000000000000711 ) ) ;
#1780 = CARTESIAN_POINT ( 'NONE',  ( 33.58253175000000823, 66.02500000273118985, 10.91162601494192863 ) ) ;
#1781 = CARTESIAN_POINT ( 'NONE',  ( -7.505752307972844761, 38.35416666666666430, 28.01184896238304134 ) ) ;
#1782 = EDGE_CURVE ( 'NONE', #20971, #6049, #18351, .T. ) ;
#1783 = CARTESIAN_POINT ( 'NONE',  ( 19.82091636218621389, 10.19999999999998685, -14.40073868116559197 ) ) ;
#1784 = CARTESIAN_POINT ( 'NONE',  ( 6.486482029760649416E-15, 1.875000002731177728, 35.31076352940723240 ) ) ;
#1785 = CARTESIAN_POINT ( 'NONE',  ( 6.486482029760649416E-15, 7.625000002731170845, 35.31076352940723240 ) ) ;
#1786 = CARTESIAN_POINT ( 'NONE',  ( 4.041334437186266200E-15, -12.99999999999999822, 33.00000000000000000 ) ) ;
#1787 = CARTESIAN_POINT ( 'NONE',  ( 25.98046417659831775, 56.25222249907602645, -15.04653450569338879 ) ) ;
#1788 = CARTESIAN_POINT ( 'NONE',  ( 32.50000000000000000, 37.09999999999999432, -10.55989012756945833 ) ) ;
#1789 = CARTESIAN_POINT ( 'NONE',  ( 28.01184896238290278, 61.27083333333332860, -7.505752307973347470 ) ) ;
#1790 = CARTESIAN_POINT ( 'NONE',  ( 5.779280353836490358E-15, 19.00000000546237544, 32.49999999999999289 ) ) ;
#1791 = EDGE_CURVE ( 'NONE', #438, #17032, #10195, .T. ) ;
#1792 = FACE_OUTER_BOUND ( 'NONE', #13191, .T. ) ;
#1793 = CARTESIAN_POINT ( 'NONE',  ( -4.732186688966233175E-15, 7.249999994537616566, 25.76082449383753925 ) ) ;
#1794 = CARTESIAN_POINT ( 'NONE',  ( -9.270509831248425314, 75.95000000546237118, -12.75976212528059861 ) ) ;
#1795 = CARTESIAN_POINT ( 'NONE',  ( 24.20753774853756113, 27.32552083333332860, 13.97622843553589789 ) ) ;
#1796 = CARTESIAN_POINT ( 'NONE',  ( -20.75514604977248112, 37.42500000273118843, 28.56700777964554661 ) ) ;
#1797 = AXIS2_PLACEMENT_3D ( 'NONE', #2551, #23660, #26230 ) ;
#1798 = CARTESIAN_POINT ( 'NONE',  ( -8.601468415847515203, 71.17500000273118133, 11.83890561707634959 ) ) ;
#1799 = CARTESIAN_POINT ( 'NONE',  ( 20.75514604977248467, 40.67500000273116711, -28.56700777964554305 ) ) ;
#1800 = CARTESIAN_POINT ( 'NONE',  ( 33.58253175000000113, 22.37500000273118417, -4.112674001490185761E-15 ) ) ;
#1801 = CARTESIAN_POINT ( 'NONE',  ( -5.147494310547430452, 12.05125428700922718, -32.49999999999999289 ) ) ;
#1802 = AXIS2_PLACEMENT_3D ( 'NONE', #18407, #5351, #3448 ) ;
#1803 = EDGE_CURVE ( 'NONE', #29733, #5805, #14784, .T. ) ;
#1804 = CARTESIAN_POINT ( 'NONE',  ( -26.29305231718579350, 17.79999999999998295, -19.10302069950537884 ) ) ;
#1805 = CARTESIAN_POINT ( 'NONE',  ( 20.08610463437157279, 79.29999999999999716, -27.64615127144129758 ) ) ;
#1806 = CARTESIAN_POINT ( 'NONE',  ( -10.04305231718578462, 60.39999999999999858, 30.90933677959249337 ) ) ;
#1807 = CARTESIAN_POINT ( 'NONE',  ( -7.236395654485763274, 12.02499999726880375, 22.27133577429736633 ) ) ;
#1808 = CARTESIAN_POINT ( 'NONE',  ( -28.00173670424535644, 27.17670166574268009, 7.543491769121936308 ) ) ;
#1809 = CARTESIAN_POINT ( 'NONE',  ( -7.236395654485757944, 3.724999997268802154, -22.27133577429736988 ) ) ;
#1810 = CARTESIAN_POINT ( 'NONE',  ( 0.04044903255044120238, 33.33555583240935505, 27.95245687107223276 ) ) ;
#1811 = CARTESIAN_POINT ( 'NONE',  ( 27.16883889988624290, 78.17500000273118133, 19.73931689729373673 ) ) ;
#1812 = CARTESIAN_POINT ( 'NONE',  ( 6.486482029760648627E-15, 13.62500000273118417, 35.31076352940722529 ) ) ;
#1813 = CARTESIAN_POINT ( 'NONE',  ( -14.47279130897151589, 11.82499999726882578, -19.92008829642072598 ) ) ;
#1814 = CARTESIAN_POINT ( 'NONE',  ( 24.20753774853756113, 61.70052083333331439, 13.97622843553589789 ) ) ;
#1815 = ORIENTED_EDGE ( 'NONE', *, *, #23644, .F. ) ;
#1816 = CARTESIAN_POINT ( 'NONE',  ( 33.58253175000000113, 50.12500000273119127, -4.112674001490185761E-15 ) ) ;
#1817 = CARTESIAN_POINT ( 'NONE',  ( -27.16883889988624290, 21.17500000273118843, -19.73931689729374028 ) ) ;
#1818 = ORIENTED_EDGE ( 'NONE', *, *, #11970, .T. ) ;
#1819 = CARTESIAN_POINT ( 'NONE',  ( 15.01150461594596308, 29.90364583333332504, -26.00068869287367335 ) ) ;
#1820 = CARTESIAN_POINT ( 'NONE',  ( -0.04044903254990864921, 29.33631916759064850, 30.02300923189239867 ) ) ;
#1821 = CARTESIAN_POINT ( 'NONE',  ( -1.778240108872766143E-15, 7.500000000000001776, -32.49999999999999289 ) ) ;
#1822 = CARTESIAN_POINT ( 'NONE',  ( 0.000000000000000000, 102.0000000000000284, 0.000000000000000000 ) ) ;
#1823 = CARTESIAN_POINT ( 'NONE',  ( 18.94512977948576093, 1.324999997268816454, -13.76444248337722875 ) ) ;
#1824 = VECTOR ( 'NONE', #15914, 1000.000000000000000 ) ;
#1825 = CARTESIAN_POINT ( 'NONE',  ( 14.47279130897151589, 12.32499999726880802, 19.92008829642072953 ) ) ;
#1826 = CARTESIAN_POINT ( 'NONE',  ( -27.16883889988623935, 19.57500000273118701, 19.73931689729374739 ) ) ;
#1827 = CARTESIAN_POINT ( 'NONE',  ( 32.50000000000000711, 25.40000000546236691, 10.55989012756945122 ) ) ;
#1828 = CARTESIAN_POINT ( 'NONE',  ( 32.50000000000000000, 65.00000000000000000, -3.980102097228898626E-15 ) ) ;
#1829 = DIRECTION ( 'NONE',  ( -0.000000000000000000, -1.000000000000000000, -0.000000000000000000 ) ) ;
#1830 = CARTESIAN_POINT ( 'NONE',  ( -6.159586018150516651, 74.00000000000001421, 12.99395819748794700 ) ) ;
#1831 = CARTESIAN_POINT ( 'NONE',  ( 28.01184896238290278, 16.58333333333333215, -7.505752307973347470 ) ) ;
#1832 = CARTESIAN_POINT ( 'NONE',  ( -33.58253175000000113, 37.47500000273118559, 10.91162601494193929 ) ) ;
#1833 = CARTESIAN_POINT ( 'NONE',  ( 10.04305231718579705, 43.10000000546237686, 30.90933677959248982 ) ) ;
#1834 = CARTESIAN_POINT ( 'NONE',  ( -15.01150461594642316, 32.76822916666666430, -26.00068869287341045 ) ) ;
#1835 = APPLICATION_PROTOCOL_DEFINITION ( 'draft international standard', 'automotive_design', 1998, #14461 ) ;
#1836 = CARTESIAN_POINT ( 'NONE',  ( 23.41746825000000243, 15.22499999726880482, -7.608796670333727974 ) ) ;
#1837 = CARTESIAN_POINT ( 'NONE',  ( 32.50000000000000711, 8.900000000000011013, 10.55989012756945122 ) ) ;
#1838 = CARTESIAN_POINT ( 'NONE',  ( 26.29305231718579350, 9.300000005462383257, 19.10302069950537529 ) ) ;
#1839 = CARTESIAN_POINT ( 'NONE',  ( 27.95245687107223276, 49.66368083240936215, -0.04044903255042905932 ) ) ;
#1840 = CARTESIAN_POINT ( 'NONE',  ( 10.37757302488624056, 54.52500000273119696, -31.93888565452638417 ) ) ;
#1841 = CARTESIAN_POINT ( 'NONE',  ( 20.75514604977248467, 60.67500000273118133, -28.56700777964554305 ) ) ;
#1842 = CARTESIAN_POINT ( 'NONE',  ( -2.162160676586882350E-15, 40.87500000273119838, -35.31076352940722529 ) ) ;
#1843 =( BOUNDED_CURVE ( )  B_SPLINE_CURVE ( 2, ( #32968, #22353, #6566, #30573, #9293, #22693, #7070, #2095, #17554, #19778, #25443, #1918, #12395 ),
 .UNSPECIFIED., .F., .F. ) 
 B_SPLINE_CURVE_WITH_KNOTS ( ( 3, 2, 2, 2, 2, 2, 3 ),
 ( 0.3500000000000000333, 0.3599999999999999867, 0.3800000000000000044, 0.4000000000000000222, 0.4199999999999999845, 0.4400000000000000022, 0.4500000000000000111 ),
 .UNSPECIFIED. ) 
 CURVE ( )  GEOMETRIC_REPRESENTATION_ITEM ( )  RATIONAL_B_SPLINE_CURVE ( ( 0.9755282581475768211, 0.9755282581475768211, 1.000000000000000000, 0.9510565162951535312, 1.000000000000000000, 0.9510565162951535312, 1.000000000000000000, 0.9510565162951535312, 1.000000000000000000, 0.9510565162951535312, 1.000000000000000000, 0.9755282581475768211, 0.9755282581475768211 ) ) 
 REPRESENTATION_ITEM ( '' )  );
#1844 = FACE_OUTER_BOUND ( 'NONE', #14245, .T. ) ;
#1845 = CARTESIAN_POINT ( 'NONE',  ( -5.147494310547430452, 49.55125428154685352, -32.49999999999999289 ) ) ;
#1846 = CARTESIAN_POINT ( 'NONE',  ( 19.06425588902592239, 52.96913166759063785, 19.11951029504763611 ) ) ;
#1847 = EDGE_CURVE ( 'NONE', #3734, #17459, #13698, .T. ) ;
#1848 = CARTESIAN_POINT ( 'NONE',  ( 32.50000000000000000, 63.50000000546239676, -3.980102097228898626E-15 ) ) ;
#1849 = CARTESIAN_POINT ( 'NONE',  ( -5.147494310547430452, 41.55125428154684641, -32.49999999999999289 ) ) ;
#1850 = CARTESIAN_POINT ( 'NONE',  ( 33.58253175000000113, 24.22500000273119625, -10.91162601494193751 ) ) ;
#1851 = FACE_OUTER_BOUND ( 'NONE', #29137, .T. ) ;
#1852 = CARTESIAN_POINT ( 'NONE',  ( -4.635254915624208216, 78.65000000546234560, 14.26584774442730463 ) ) ;
#1853 = TOROIDAL_SURFACE ( 'NONE', #7348, 12.11607355459420177, 2.000000000000000000 ) ;
#1854 = AXIS2_PLACEMENT_3D ( 'NONE', #13967, #24431, #32646 ) ;
#1855 = CARTESIAN_POINT ( 'NONE',  ( -5.147494310547427787, 78.05125428700921475, -32.49999999999999289 ) ) ;
#1856 = CARTESIAN_POINT ( 'NONE',  ( -14.97647472619899389, 67.99701416574269786, 26.02091320914878025 ) ) ;
#1857 = CARTESIAN_POINT ( 'NONE',  ( 10.04305231718579705, 39.10000000546236265, 30.90933677959248982 ) ) ;
#1858 = CARTESIAN_POINT ( 'NONE',  ( 5.779280353836490358E-15, 34.49999999999998579, 32.49999999999999289 ) ) ;
#1859 = CARTESIAN_POINT ( 'NONE',  ( -33.58253175000000113, 31.22500000273118204, 10.91162601494193929 ) ) ;
#1860 = CARTESIAN_POINT ( 'NONE',  ( -10.37757302488624411, 64.97500000273120691, -31.93888565452638417 ) ) ;
#1861 = CARTESIAN_POINT ( 'NONE',  ( -26.07999730980490583, 32.33854166666666430, -6.988114217767815717 ) ) ;
#1862 = CARTESIAN_POINT ( 'NONE',  ( -33.58253175000000113, 69.22500000273117848, 10.91162601494193929 ) ) ;
#1863 = CARTESIAN_POINT ( 'NONE',  ( -28.01184896238304134, 39.21354166666666430, -7.505752307972844761 ) ) ;
#1864 = CARTESIAN_POINT ( 'NONE',  ( 13.38432950954957512, -58.51673569255127205, 1.639107629260334588E-15 ) ) ;
#1865 = VERTEX_POINT ( 'NONE', #24906 ) ;
#1866 = CARTESIAN_POINT ( 'NONE',  ( -0.04044903254990864921, 56.83631916759064495, 30.02300923189239867 ) ) ;
#1867 = CARTESIAN_POINT ( 'NONE',  ( -26.09010956794232428, 57.55246500092398065, 6.950374756619732253 ) ) ;
#1868 = CARTESIAN_POINT ( 'NONE',  ( -33.58253175000000113, 11.12500000273118594, 0.000000000000000000 ) ) ;
#1869 = CARTESIAN_POINT ( 'NONE',  ( -0.04044903255044120238, 17.86680583240935860, -30.02300923189239867 ) ) ;
#1870 = CARTESIAN_POINT ( 'NONE',  ( 5.779280353836490358E-15, 66.50000000000000000, 32.49999999999999289 ) ) ;
#1871 = CARTESIAN_POINT ( 'NONE',  ( -33.58253175000000113, 41.27500000273117564, -10.91162601494193218 ) ) ;
#1872 = CARTESIAN_POINT ( 'NONE',  ( 26.29305231718579350, 43.30000000546238681, 19.10302069950537529 ) ) ;
#1873 = CARTESIAN_POINT ( 'NONE',  ( 2.897257156509938333E-15, 74.49999999999995737, 15.77193336357400710 ) ) ;
#1874 = CARTESIAN_POINT ( 'NONE',  ( -20.75514604977248112, 29.42500000273118133, 28.56700777964554661 ) ) ;
#1875 = CARTESIAN_POINT ( 'NONE',  ( 24.50000000000000000, 13.64999999453761781, 7.960532557706212486 ) ) ;
#1876 = CARTESIAN_POINT ( 'NONE',  ( -20.75514604977248112, 55.67500000273118843, 28.56700777964554661 ) ) ;
#1877 =( LENGTH_UNIT ( ) NAMED_UNIT ( * ) SI_UNIT ( .MILLI., .METRE. ) );
#1878 = CARTESIAN_POINT ( 'NONE',  ( -26.29305231718578995, 28.19999999999998863, 19.10302069950538595 ) ) ;
#1879 = CARTESIAN_POINT ( 'NONE',  ( -10.04305231718579172, 31.59999999999999076, -30.90933677959248982 ) ) ;
#1880 = CARTESIAN_POINT ( 'NONE',  ( -15.14183272437241889, 0.7000000000000070610, -20.84094480462497856 ) ) ;
#1881 = CARTESIAN_POINT ( 'NONE',  ( 10.37757302488624056, 76.52500000273118985, -31.93888565452638417 ) ) ;
#1882 = DIRECTION ( 'NONE',  ( 0.000000000000000000, -0.000000000000000000, -1.000000000000000000 ) ) ;
#1883 = CARTESIAN_POINT ( 'NONE',  ( 5.779280353836490358E-15, 38.50000000000000000, 32.49999999999999289 ) ) ;
#1884 = CARTESIAN_POINT ( 'NONE',  ( 33.58253175000000113, 68.37500000273119838, -4.112674001490185761E-15 ) ) ;
#1885 = CARTESIAN_POINT ( 'NONE',  ( 15.00000000000000000, 75.35000000546236265, -4.873795443493596835 ) ) ;
#1886 = ORIENTED_EDGE ( 'NONE', *, *, #20671, .F. ) ;
#1887 = CARTESIAN_POINT ( 'NONE',  ( 27.16883889988624290, 19.92500000273117422, 19.73931689729373673 ) ) ;
#1888 = PRODUCT_DEFINITION_SHAPE ( 'NONE', 'NONE',  #33991 ) ;
#1889 = CARTESIAN_POINT ( 'NONE',  ( 15.14183272437241889, 11.44999999453763095, 20.84094480462498211 ) ) ;
#1890 = CARTESIAN_POINT ( 'NONE',  ( 7.025853678916403666, 17.44829833425730925, -26.06988505166735237 ) ) ;
#1891 = EDGE_CURVE ( 'NONE', #6637, #30070, #484, .T. ) ;
#1892 = CARTESIAN_POINT ( 'NONE',  ( 2.445080149700053643E-15, 74.75000000546239676, 15.00000000000000000 ) ) ;
#1893 = CARTESIAN_POINT ( 'NONE',  ( 20.75514604977248467, 38.42500000273118133, -28.56700777964554305 ) ) ;
#1894 = CARTESIAN_POINT ( 'NONE',  ( 6.486482029760649416E-15, 5.875000002731183280, 35.31076352940723240 ) ) ;
#1895 = CARTESIAN_POINT ( 'NONE',  ( -27.16883889988624290, 57.17500000273119554, -19.73931689729374028 ) ) ;
#1896 = CARTESIAN_POINT ( 'NONE',  ( -30.02300923189239867, 50.82069416759063785, -0.04044903254991731589 ) ) ;
#1897 = EDGE_CURVE ( 'NONE', #21971, #4339, #29772, .T. ) ;
#1898 = CARTESIAN_POINT ( 'NONE',  ( 4.300734207923757602, 80.27500000273118985, -13.23629886949340673 ) ) ;
#1899 = CARTESIAN_POINT ( 'NONE',  ( -15.04653450569338524, 38.20534749907601935, -25.98046417659831775 ) ) ;
#1900 = CARTESIAN_POINT ( 'NONE',  ( 6.277390505771533514E-15, 63.00000000546238255, 34.17252228774368916 ) ) ;
#1901 = CARTESIAN_POINT ( 'NONE',  ( -13.91746824999999532, 74.77500000273118985, -4.522059556121115875 ) ) ;
#1902 = CARTESIAN_POINT ( 'NONE',  ( -14.01125832528328985, 65.70534749907602645, -24.18731323226223040 ) ) ;
#1903 = CARTESIAN_POINT ( 'NONE',  ( 7.236395654485760609, 1.524999997268822183, -22.27133577429736633 ) ) ;
#1904 = CARTESIAN_POINT ( 'NONE',  ( -20.08610463437156923, 76.80000000546239391, 27.64615127144130113 ) ) ;
#1905 = CARTESIAN_POINT ( 'NONE',  ( 0.000000000000000000, 70.00000000000000000, 0.000000000000000000 ) ) ;
#1906 = CARTESIAN_POINT ( 'NONE',  ( -27.16883889988623935, 37.57500000273118701, 19.73931689729374739 ) ) ;
#1907 = CARTESIAN_POINT ( 'NONE',  ( 14.47279130897151767, 8.824999997268804464, 19.92008829642072953 ) ) ;
#1908 = ORIENTED_EDGE ( 'NONE', *, *, #1030, .T. ) ;
#1909 = CARTESIAN_POINT ( 'NONE',  ( -33.58253175000000113, 75.37500000273116996, 0.000000000000000000 ) ) ;
#1910 = CARTESIAN_POINT ( 'NONE',  ( -32.50000000000000000, 24.40000000546237047, -10.55989012756945478 ) ) ;
#1911 = CARTESIAN_POINT ( 'NONE',  ( 7.505752307972854531, 46.94791666666666430, -28.01184896238303423 ) ) ;
#1912 = CARTESIAN_POINT ( 'NONE',  ( -20.08610463437157989, 66.20000000546238539, -27.64615127144129758 ) ) ;
#1913 = EDGE_LOOP ( 'NONE', ( #4571, #8333, #33317, #766, #26937, #32376, #8454, #22179 ) ) ;
#1914 = DIRECTION ( 'NONE',  ( 0.000000000000000000, 0.000000000000000000, 1.000000000000000000 ) ) ;
#1915 = CARTESIAN_POINT ( 'NONE',  ( -10.37757302488624411, 48.72500000273119269, -31.93888565452638417 ) ) ;
#1916 = CARTESIAN_POINT ( 'NONE',  ( -23.41746825000000598, 17.72499999726881725, 7.608796670333726198 ) ) ;
#1917 = CARTESIAN_POINT ( 'NONE',  ( -10.04305231718578462, 6.900000005462370467, 30.90933677959249337 ) ) ;
#1918 = CARTESIAN_POINT ( 'NONE',  ( -2.375766604868045029, 77.55125428154684641, -14.99999999999999822 ) ) ;
#1919 = CARTESIAN_POINT ( 'NONE',  ( 20.50609665440969565, 12.85937500000000000, -20.50609665441004736 ) ) ;
#1920 = COLOUR_RGB ( '', 0.66274510, 0.83137255, 0.94901961) ;
#1921 = CARTESIAN_POINT ( 'NONE',  ( 10.04305231718579705, 52.60000000000000853, 30.90933677959248982 ) ) ;
#1922 = CARTESIAN_POINT ( 'NONE',  ( 24.50000000000000000, 2.099999999999991651, -7.960532557706203605 ) ) ;
#1923 = CARTESIAN_POINT ( 'NONE',  ( -2.162160676586881955E-15, 16.87500000273120193, -35.31076352940723240 ) ) ;
#1924 = DIRECTION ( 'NONE',  ( -0.000000000000000000, -1.000000000000000000, -0.000000000000000000 ) ) ;
#1925 = CARTESIAN_POINT ( 'NONE',  ( 24.18731323226221974, 21.87722249907602290, -14.01125832528328985 ) ) ;
#1926 = CARTESIAN_POINT ( 'NONE',  ( -8.601468415847515203, 71.17500000273115290, 11.83890561707634959 ) ) ;
#1927 = CARTESIAN_POINT ( 'NONE',  ( 7.570916362186213000, 8.399999999999991473, -23.30088464923126423 ) ) ;
#1928 = CARTESIAN_POINT ( 'NONE',  ( 0.000000000000000000, 52.00000000000000711, 0.000000000000000000 ) ) ;
#1929 = CARTESIAN_POINT ( 'NONE',  ( 26.29305231718579350, 4.799999999999998934, 19.10302069950537529 ) ) ;
#1930 = ORIENTED_EDGE ( 'NONE', *, *, #18271, .T. ) ;
#1931 = CARTESIAN_POINT ( 'NONE',  ( 18.94512977948576093, 15.32499999726880091, -13.76444248337722875 ) ) ;
#1932 = CARTESIAN_POINT ( 'NONE',  ( 14.47279130897151944, 0.9249999972688209837, -19.92008829642072598 ) ) ;
#1933 = CARTESIAN_POINT ( 'NONE',  ( -19.09188309203694445, 49.81249999999999289, -19.09188309203661049 ) ) ;
#1934 = CARTESIAN_POINT ( 'NONE',  ( -10.37757302488624411, 62.72500000273119269, -31.93888565452638417 ) ) ;
#1935 = CARTESIAN_POINT ( 'NONE',  ( -27.16883889988623935, 21.57500000273120122, 19.73931689729374739 ) ) ;
#1936 = CARTESIAN_POINT ( 'NONE',  ( -33.58253175000000113, 13.47500000273118914, 10.91162601494193929 ) ) ;
#1937 = CARTESIAN_POINT ( 'NONE',  ( -26.07999730980490583, 28.90104166666666785, -6.988114217767815717 ) ) ;
#1938 = CARTESIAN_POINT ( 'NONE',  ( 27.16883889988623935, 4.575000002731199444, -19.73931689729374384 ) ) ;
#1939 = CARTESIAN_POINT ( 'NONE',  ( 20.47846945139902530, 22.03163166759064495, 20.53372385742071771 ) ) ;
#1940 = EDGE_CURVE ( 'NONE', #28718, #20887, #4791, .T. ) ;
#1941 = CARTESIAN_POINT ( 'NONE',  ( -28.01184896238304134, 59.83854166666666430, -7.505752307972844761 ) ) ;
#1942 = EDGE_CURVE ( 'NONE', #22733, #28806, #27713, .T. ) ;
#1943 = CARTESIAN_POINT ( 'NONE',  ( -33.58253175000000113, 5.225000002731188253, 10.91162601494193929 ) ) ;
#1944 = CARTESIAN_POINT ( 'NONE',  ( 32.50000000000000000, 69.00000000000000000, -3.980102097228898626E-15 ) ) ;
#1945 = CARTESIAN_POINT ( 'NONE',  ( 10.04305231718579705, 40.60000000000000853, 30.90933677959248982 ) ) ;
#1946 = CARTESIAN_POINT ( 'NONE',  ( -2.162160676586882350E-15, 44.62500000273119838, -35.31076352940722529 ) ) ;
#1947 = CARTESIAN_POINT ( 'NONE',  ( -23.41746825000000243, 3.524999997268826402, -7.608796670333730638 ) ) ;
#1948 = CARTESIAN_POINT ( 'NONE',  ( 10.04305231718579705, 21.10000000546238752, 30.90933677959248982 ) ) ;
#1949 = STYLED_ITEM ( 'NONE', ( #25225 ), #13626 ) ;
#1950 = EDGE_LOOP ( 'NONE', ( #6804, #16249, #16847, #32834 ) ) ;
#1951 = CARTESIAN_POINT ( 'NONE',  ( 27.16883889988623935, 58.57500000273117990, -19.73931689729374384 ) ) ;
#1952 =( BOUNDED_CURVE ( )  B_SPLINE_CURVE ( 2, ( #2358, #18503, #16757, #1109, #19331, #11594, #27216, #6281, #3378, #3709, #14179 ),
 .UNSPECIFIED., .F., .T. ) 
 B_SPLINE_CURVE_WITH_KNOTS ( ( 3, 2, 2, 2, 2, 3 ),
 ( 0.8055555555555555802, 0.8111111111111111160, 0.8222222222222221877, 0.8333333333333333703, 0.8444444444444444420, 0.8472738309268738055 ),
 .UNSPECIFIED. ) 
 CURVE ( )  GEOMETRIC_REPRESENTATION_ITEM ( )  RATIONAL_B_SPLINE_CURVE ( ( 0.9755282581475768211, 0.9755282581475768211, 1.000000000000000000, 0.9510565162951535312, 1.000000000000000000, 0.9510565162951535312, 1.000000000000000000, 0.9510565162951535312, 1.000000000000000000, 0.9875367971922254240, 0.9814209735438276239 ) ) 
 REPRESENTATION_ITEM ( '' )  );
#1953 = CARTESIAN_POINT ( 'NONE',  ( 5.147494310547434893, 42.55125428154684641, 32.49999999999999289 ) ) ;
#1954 = CARTESIAN_POINT ( 'NONE',  ( 1.507698388325705758E-15, 13.12499999726881228, -24.62258325217400312 ) ) ;
#1955 = CARTESIAN_POINT ( 'NONE',  ( -14.01125832528285109, 33.06027750092398776, 24.18731323226248264 ) ) ;
#1956 = CARTESIAN_POINT ( 'NONE',  ( -20.75514604977248112, 73.67500000273120975, 28.56700777964554661 ) ) ;
#1957 = ORIENTED_EDGE ( 'NONE', *, *, #17449, .T. ) ;
#1958 = CARTESIAN_POINT ( 'NONE',  ( 6.486482029760649416E-15, 31.62500000273119483, 35.31076352940723240 ) ) ;
#1959 = CARTESIAN_POINT ( 'NONE',  ( -26.00068869287340334, 18.15885416666666075, 15.01150461594643382 ) ) ;
#1960 = EDGE_LOOP ( 'NONE', ( #18655, #11215, #15221, #19732 ) ) ;
#1961 = VECTOR ( 'NONE', #29560, 1000.000000000000000 ) ;
#1962 = CARTESIAN_POINT ( 'NONE',  ( -12.13525491562420910, 76.19999999999998863, 8.816778784387098611 ) ) ;
#1963 = CARTESIAN_POINT ( 'NONE',  ( 20.75514604977249178, 65.82500000273115859, 28.56700777964553950 ) ) ;
#1964 = CARTESIAN_POINT ( 'NONE',  ( 15.01150461594596308, 36.77864583333332860, -26.00068869287367335 ) ) ;
#1965 = CARTESIAN_POINT ( 'NONE',  ( -7.570916362186215665, 9.399999999999991473, 23.30088464923126423 ) ) ;
#1966 = CARTESIAN_POINT ( 'NONE',  ( 14.47279130897151767, 4.824999997268814234, 19.92008829642072953 ) ) ;
#1967 = CARTESIAN_POINT ( 'NONE',  ( 33.58253175000000113, 10.22500000273117671, -10.91162601494193751 ) ) ;
#1968 = CARTESIAN_POINT ( 'NONE',  ( -7.570916362186215665, 7.149999994537637349, 23.30088464923126423 ) ) ;
#1969 = CARTESIAN_POINT ( 'NONE',  ( 0.04044903255045854962, 53.96055583240936926, 30.02300923189239867 ) ) ;
#1970 = CARTESIAN_POINT ( 'NONE',  ( -9.270509831248425314, 75.69999999999998863, -12.75976212528059861 ) ) ;
#1971 = CARTESIAN_POINT ( 'NONE',  ( 2.740863092043355209E-13, 65.71093749999998579, 30.02300923189239867 ) ) ;
#1972 = CARTESIAN_POINT ( 'NONE',  ( -10.04305231718578462, 70.40000000000001990, 30.90933677959249337 ) ) ;
#1973 = DIRECTION ( 'NONE',  ( 0.000000000000000000, 0.000000000000000000, 1.000000000000000000 ) ) ;
#1974 = CARTESIAN_POINT ( 'NONE',  ( 15.14183272437241889, 15.44999999453761852, 20.84094480462498211 ) ) ;
#1975 = CARTESIAN_POINT ( 'NONE',  ( 9.270509831248425314, 74.95000000546237118, 12.75976212528059683 ) ) ;
#1976 = CARTESIAN_POINT ( 'NONE',  ( -19.09188309203660694, 24.89062500000000000, 19.09188309203694800 ) ) ;
#1977 = CARTESIAN_POINT ( 'NONE',  ( -27.16883889988623935, 29.32500000273119412, 19.73931689729374739 ) ) ;
#1978 = CARTESIAN_POINT ( 'NONE',  ( 20.75514604977248467, 78.42500000273116711, -28.56700777964554305 ) ) ;
#1979 = CARTESIAN_POINT ( 'NONE',  ( -33.58253175000000113, 43.47500000273117138, 10.91162601494193929 ) ) ;
#1980 = CARTESIAN_POINT ( 'NONE',  ( -10.37757302488624411, 18.97500000273119625, -31.93888565452638417 ) ) ;
#1981 = FACE_OUTER_BOUND ( 'NONE', #8042, .T. ) ;
#1982 = CARTESIAN_POINT ( 'NONE',  ( -24.50000000000000000, 14.74999999453763166, -3.000384657911015469E-15 ) ) ;
#1983 = CARTESIAN_POINT ( 'NONE',  ( 32.50000000000000000, 33.00000000000000000, -3.980102097228898626E-15 ) ) ;
#1984 = CARTESIAN_POINT ( 'NONE',  ( -26.29305231718578995, 58.20000000000001705, 19.10302069950538595 ) ) ;
#1985 = CARTESIAN_POINT ( 'NONE',  ( 23.41746824999999887, 16.62499999726882294, 0.000000000000000000 ) ) ;
#1986 = CARTESIAN_POINT ( 'NONE',  ( 27.16883889988624290, 63.92500000273118843, 19.73931689729373673 ) ) ;
#1987 = CARTESIAN_POINT ( 'NONE',  ( -14.47279130897151589, 1.824999997268821339, -19.92008829642072598 ) ) ;
#1988 = CARTESIAN_POINT ( 'NONE',  ( -13.94119854578892514, 37.05951416574268364, 24.22776226481266448 ) ) ;
#1989 = CARTESIAN_POINT ( 'NONE',  ( -2.162160676586881955E-15, 76.87500000273115575, -35.31076352940723240 ) ) ;
#1990 = CARTESIAN_POINT ( 'NONE',  ( -2.162160676586882350E-15, 8.625000002731168181, -35.31076352940722529 ) ) ;
#1991 = CARTESIAN_POINT ( 'NONE',  ( -4.523095164977116484E-15, 12.62499999726879985, 24.62258325217400312 ) ) ;
#1992 = CARTESIAN_POINT ( 'NONE',  ( 2.584737979205441561E-13, 62.27343749999999289, 27.95245687107222921 ) ) ;
#1993 = ORIENTED_EDGE ( 'NONE', *, *, #6515, .F. ) ;
#1994 = CARTESIAN_POINT ( 'NONE',  ( -10.37757302488623701, 49.52500000273117564, 31.93888565452638417 ) ) ;
#1995 = CARTESIAN_POINT ( 'NONE',  ( 33.58253175000000823, 24.27500000273120051, 10.91162601494192863 ) ) ;
#1996 = ORIENTED_EDGE ( 'NONE', *, *, #9547, .T. ) ;
#1997 = CARTESIAN_POINT ( 'NONE',  ( -26.00068869287340334, 35.34635416666666430, 15.01150461594643382 ) ) ;
#1998 = CARTESIAN_POINT ( 'NONE',  ( 7.543491769121427382, 31.19829833425730570, -28.00173670424548433 ) ) ;
#1999 = DIRECTION ( 'NONE',  ( -0.000000000000000000, -1.000000000000000000, -0.000000000000000000 ) ) ;
#2000 = DIRECTION ( 'NONE',  ( -0.000000000000000000, -1.000000000000000000, -0.000000000000000000 ) ) ;
#2001 = CARTESIAN_POINT ( 'NONE',  ( 23.41746825000000243, 7.024999997268802865, 7.608796670333735079 ) ) ;
#2002 = CARTESIAN_POINT ( 'NONE',  ( 7.236395654485755280, 14.22499999726881192, 22.27133577429736988 ) ) ;
#2003 = CARTESIAN_POINT ( 'NONE',  ( 27.16883889988623935, 14.57500000273120833, -19.73931689729374384 ) ) ;
#2004 = CARTESIAN_POINT ( 'NONE',  ( -32.50000000000000000, 24.60000000546236620, 10.55989012756946366 ) ) ;
#2005 = CARTESIAN_POINT ( 'NONE',  ( 32.50000000000000711, 62.89999999999999147, 10.55989012756945122 ) ) ;
#2006 = CARTESIAN_POINT ( 'NONE',  ( -8.891200544363830713E-16, 77.75000000546236834, -15.00000000000000000 ) ) ;
#2007 = CARTESIAN_POINT ( 'NONE',  ( -22.23068731925732422, 67.00000000000001421, -25.26668985625435226 ) ) ;
#2008 = CARTESIAN_POINT ( 'NONE',  ( 7.468012846824777284, 63.56809000092398065, 28.02196122052045268 ) ) ;
#2009 = CARTESIAN_POINT ( 'NONE',  ( 33.58253175000000823, 32.27500000273117564, 10.91162601494192863 ) ) ;
#2010 = CARTESIAN_POINT ( 'NONE',  ( -4.300734207923759378, 80.97500000273119269, -13.23629886949340495 ) ) ;
#2011 = CARTESIAN_POINT ( 'NONE',  ( 2.740863092043355209E-13, 34.77343750000000000, 30.02300923189239867 ) ) ;
#2012 = DIRECTION ( 'NONE',  ( 1.000000000000000000, 0.000000000000000000, 0.000000000000000000 ) ) ;
#2013 = TOROIDAL_SURFACE ( 'NONE', #21222, 12.11607355459420177, 2.000000000000000000 ) ;
#2014 = CARTESIAN_POINT ( 'NONE',  ( -14.47279130897152122, 18.42499999726882365, 19.92008829642072243 ) ) ;
#2015 = CARTESIAN_POINT ( 'NONE',  ( -32.50000000000000000, 10.00000000000000888, 0.000000000000000000 ) ) ;
#2016 = CYLINDRICAL_SURFACE ( 'NONE', #30194, 32.50000000000000000 ) ;
#2017 = CARTESIAN_POINT ( 'NONE',  ( -19.11951029504797006, 48.37461833240936215, -19.06425588902558133 ) ) ;
#2018 = CARTESIAN_POINT ( 'NONE',  ( -33.58253175000000113, 51.22500000273119269, 10.91162601494193929 ) ) ;
#2019 = CARTESIAN_POINT ( 'NONE',  ( -20.75514604977248112, 63.67500000273116711, 28.56700777964554661 ) ) ;
#2020 = CARTESIAN_POINT ( 'NONE',  ( 27.16883889988624290, 40.17500000273119554, 19.73931689729373673 ) ) ;
#2021 = CARTESIAN_POINT ( 'NONE',  ( 23.41746824999999887, 14.62499999726882294, 0.000000000000000000 ) ) ;
#2022 = VECTOR ( 'NONE', #3479, 1000.000000000000000 ) ;
#2023 = CARTESIAN_POINT ( 'NONE',  ( 19.82091636218621389, 10.19999999999998685, -14.40073868116559197 ) ) ;
#2024 = CARTESIAN_POINT ( 'NONE',  ( -32.50000000000000000, 49.99999999999998579, 0.000000000000000000 ) ) ;
#2025 = EDGE_CURVE ( 'NONE', #24744, #7658, #28169, .T. ) ;
#2026 = CARTESIAN_POINT ( 'NONE',  ( -24.50000000000000711, 4.849999994537633974, 7.960532557706201828 ) ) ;
#2027 = CARTESIAN_POINT ( 'NONE',  ( -26.29305231718578995, 78.20000000000000284, 19.10302069950538595 ) ) ;
#2028 = CARTESIAN_POINT ( 'NONE',  ( 27.16883889988624290, 23.92500000273119198, 19.73931689729373673 ) ) ;
#2029 = CARTESIAN_POINT ( 'NONE',  ( -32.50000000000000000, 62.50000000546238255, 0.000000000000000000 ) ) ;
#2030 = DIRECTION ( 'NONE',  ( -0.7071067811865526798, 0.000000000000000000, -0.7071067811865423547 ) ) ;
#2031 = DIRECTION ( 'NONE',  ( 0.000000000000000000, 1.000000000000000000, 0.000000000000000000 ) ) ;
#2032 = CARTESIAN_POINT ( 'NONE',  ( -15.04653450569338524, 62.26784749907602645, -25.98046417659831775 ) ) ;
#2033 = CARTESIAN_POINT ( 'NONE',  ( 32.50000000000000000, 41.60000000546238397, -10.55989012756945833 ) ) ;
#2034 = DIRECTION ( 'NONE',  ( -1.224646799147353454E-16, 1.000000000000000000, -0.000000000000000000 ) ) ;
#2035 = CARTESIAN_POINT ( 'NONE',  ( 10.37757302488624056, 32.52500000273117564, -31.93888565452638417 ) ) ;
#2036 = CARTESIAN_POINT ( 'NONE',  ( -20.75514604977248112, 65.67500000273118133, 28.56700777964554661 ) ) ;
#2037 = CARTESIAN_POINT ( 'NONE',  ( 26.07999730980477437, 33.77083333333333570, -6.988114217768290004 ) ) ;
#2038 = ORIENTED_EDGE ( 'NONE', *, *, #18277, .T. ) ;
#2039 = CARTESIAN_POINT ( 'NONE',  ( -33.58253175000000113, 67.12500000273118417, 0.000000000000000000 ) ) ;
#2040 = CARTESIAN_POINT ( 'NONE',  ( -7.505752307973343918, 36.34895833333333570, -28.01184896238290989 ) ) ;
#2041 = DIRECTION ( 'NONE',  ( 0.000000000000000000, 0.000000000000000000, 1.000000000000000000 ) ) ;
#2042 = ORIENTED_EDGE ( 'NONE', *, *, #20115, .T. ) ;
#2043 = CARTESIAN_POINT ( 'NONE',  ( 7.543491769121427382, 55.26079833425730214, -28.00173670424548433 ) ) ;
#2044 = CARTESIAN_POINT ( 'NONE',  ( -14.01125832528285109, 57.12277750092398065, 24.18731323226248264 ) ) ;
#2045 = CARTESIAN_POINT ( 'NONE',  ( 10.37757302488624767, 11.72500000273117493, 31.93888565452638417 ) ) ;
#2046 = CARTESIAN_POINT ( 'NONE',  ( -0.04044903255044120238, 14.42930583240935505, -30.02300923189239867 ) ) ;
#2047 = FACE_BOUND ( 'NONE', #31107, .T. ) ;
#2048 = CARTESIAN_POINT ( 'NONE',  ( -2.162160676586881955E-15, 40.87500000273119838, -35.31076352940723240 ) ) ;
#2049 = CARTESIAN_POINT ( 'NONE',  ( 10.04305231718579705, 41.10000000546237686, 30.90933677959248982 ) ) ;
#2050 = CARTESIAN_POINT ( 'NONE',  ( -15.00000000000000000, 76.09999999999999432, 4.873795443493597723 ) ) ;
#2051 = CARTESIAN_POINT ( 'NONE',  ( -27.16883889988624290, 22.92500000273117777, -19.73931689729374028 ) ) ;
#2052 = DIRECTION ( 'NONE',  ( -0.7069718413157907166, -0.01953538259431466736, 0.7069718413158010417 ) ) ;
#2053 = CARTESIAN_POINT ( 'NONE',  ( 33.58253175000000113, 52.47500000273117138, -10.91162601494193751 ) ) ;
#2054 = CARTESIAN_POINT ( 'NONE',  ( 32.50000000000000000, 29.10000000000000853, -10.55989012756945833 ) ) ;
#2055 = CARTESIAN_POINT ( 'NONE',  ( 20.08610463437157279, 29.30000000000000782, -27.64615127144129758 ) ) ;
#2056 = CARTESIAN_POINT ( 'NONE',  ( 23.41746825000000243, 16.72499999726881725, -7.608796670333727974 ) ) ;
#2057 = CARTESIAN_POINT ( 'NONE',  ( -27.16883889988624290, 76.92500000273119554, -19.73931689729374028 ) ) ;
#2058 = CARTESIAN_POINT ( 'NONE',  ( -10.04305231718579172, 70.10000000546237686, -30.90933677959248982 ) ) ;
#2059 = CARTESIAN_POINT ( 'NONE',  ( -10.04305231718578462, 20.90000000546238113, 30.90933677959249337 ) ) ;
#2060 = CARTESIAN_POINT ( 'NONE',  ( -33.58253175000000113, 59.47500000273119269, 10.91162601494193929 ) ) ;
#2061 = CARTESIAN_POINT ( 'NONE',  ( 2.897257156509938333E-15, 74.75000000546236834, 15.77193336357400710 ) ) ;
#2062 = ORIENTED_EDGE ( 'NONE', *, *, #16915, .F. ) ;
#2063 = CARTESIAN_POINT ( 'NONE',  ( -10.37757302488624411, 18.72500000273119625, -31.93888565452638417 ) ) ;
#2064 = CARTESIAN_POINT ( 'NONE',  ( 7.570916362186213000, 10.14999999453763913, -23.30088464923126423 ) ) ;
#2065 = CARTESIAN_POINT ( 'NONE',  ( 6.950374756619721595, 18.88059000092397355, 26.09010956794232428 ) ) ;
#2066 = CARTESIAN_POINT ( 'NONE',  ( 32.50000000000000000, 46.99999999999998579, -3.980102097228898626E-15 ) ) ;
#2067 = CARTESIAN_POINT ( 'NONE',  ( 6.486482029760649416E-15, 39.62500000273117706, 35.31076352940723240 ) ) ;
#2068 = CARTESIAN_POINT ( 'NONE',  ( -10.37757302488624411, 2.975000002731182036, -31.93888565452638417 ) ) ;
#2069 = CARTESIAN_POINT ( 'NONE',  ( 27.16883889988624290, 54.17500000273118843, 19.73931689729373673 ) ) ;
#2070 = CARTESIAN_POINT ( 'NONE',  ( 15.04653450569292872, 45.09152750092398065, -25.98046417659857710 ) ) ;
#2071 = CARTESIAN_POINT ( 'NONE',  ( 7.570916362186207671, 5.599999999999994316, 23.30088464923126779 ) ) ;
#2072 = CARTESIAN_POINT ( 'NONE',  ( 14.97647472619900455, 38.77826416574269075, -26.02091320914876960 ) ) ;
#2073 = CARTESIAN_POINT ( 'NONE',  ( -32.50000000000000000, 58.40000000546237402, -10.55989012756945478 ) ) ;
#2074 = CARTESIAN_POINT ( 'NONE',  ( -8.601468415847518756, 72.57500000273114438, -11.83890561707634781 ) ) ;
#2075 = CARTESIAN_POINT ( 'NONE',  ( 19.82091636218621034, 7.549999994537620829, 14.40073868116559730 ) ) ;
#2076 = B_SPLINE_CURVE_WITH_KNOTS ( 'NONE', 3,
 ( #25351, #32719, #33410, #22780, #11964, #24837, #22603, #15062, #7154, #4074, #33057, #1315, #9562, #22435, #20040, #1830, #12131, #28098, #25178, #14378, #22276, #12308, #20217, #17129, #33232, #30835, #6814, #30485, #30657, #19863, #17637, #11798, #17469, #7327, #32882, #9215 ),
 .UNSPECIFIED., .F., .F.,
 ( 4, 2, 2, 2, 2, 2, 2, 2, 2, 2, 2, 2, 2, 2, 2, 2, 2, 4 ),
 ( 8.685284222369515922E-16, 0.001784781750657605560, 0.003569563501314342892, 0.007139127002627816687, 0.008031517877956187088, 0.008923908753284555753, 0.01070869050394129135, 0.01160108137926966002, 0.01249347225459802868, 0.01427825400525476254, 0.01606303575591149987, 0.01784781750656823027, 0.02141738100788169799, 0.02230977188321005972, 0.02320216275853842838, 0.02498694450919515878, 0.02677172625985189611, 0.02855650801050862303 ),
 .UNSPECIFIED. ) ;
#2077 = CARTESIAN_POINT ( 'NONE',  ( 7.025853678916867295, 67.56732666574268364, 26.06988505166722803 ) ) ;
#2078 = CARTESIAN_POINT ( 'NONE',  ( -26.29305231718578995, 54.19999999999999574, 19.10302069950538595 ) ) ;
#2079 = CARTESIAN_POINT ( 'NONE',  ( 20.08610463437157279, 75.80000000546237970, -27.64615127144129758 ) ) ;
#2080 = CARTESIAN_POINT ( 'NONE',  ( -15.01150461594595775, 14.43489583333332682, 26.00068869287368756 ) ) ;
#2081 = CARTESIAN_POINT ( 'NONE',  ( -33.58253175000000113, 37.47500000273118559, 10.91162601494193929 ) ) ;
#2082 = CARTESIAN_POINT ( 'NONE',  ( -23.41746824999999887, 8.024999997268800200, -7.608796670333730638 ) ) ;
#2083 = ORIENTED_EDGE ( 'NONE', *, *, #26141, .F. ) ;
#2084 = CARTESIAN_POINT ( 'NONE',  ( -20.75514604977248112, 75.67500000273118133, 28.56700777964554661 ) ) ;
#2085 = CARTESIAN_POINT ( 'NONE',  ( 20.08610463437158344, 25.20000000546237473, 27.64615127144129403 ) ) ;
#2086 = CARTESIAN_POINT ( 'NONE',  ( 28.01184896238304134, 40.93229166666666430, 7.505752307972846538 ) ) ;
#2087 = CARTESIAN_POINT ( 'NONE',  ( 32.50000000000000711, 61.40000000546237402, 10.55989012756945122 ) ) ;
#2089 = ORIENTED_EDGE ( 'NONE', *, *, #29548, .T. ) ;
#2088 = ADVANCED_FACE ( 'NONE', ( #12555 ), #4312, .F. ) ;
#2090 = CARTESIAN_POINT ( 'NONE',  ( 3.880418787951132042, 6.198745712990783474, -24.50000000000000355 ) ) ;
#2091 = CARTESIAN_POINT ( 'NONE',  ( -27.16883889988624290, 42.92500000273119554, -19.73931689729374028 ) ) ;
#2092 = CARTESIAN_POINT ( 'NONE',  ( 3.980102097228898626E-15, 80.00000000000001421, 32.50000000000000000 ) ) ;
#2093 = ADVANCED_FACE ( 'NONE', ( #12724 ), #6400, .T. ) ;
#2094 = CARTESIAN_POINT ( 'NONE',  ( 32.50000000000000000, 7.600000005462379526, -10.55989012756945833 ) ) ;
#2095 = CARTESIAN_POINT ( 'NONE',  ( -15.00000000000000000, 77.90000000000000568, -4.873795443493594171 ) ) ;
#2096 = CARTESIAN_POINT ( 'NONE',  ( -15.01150461594642316, 12.14322916666666430, -26.00068869287341045 ) ) ;
#2097 = CARTESIAN_POINT ( 'NONE',  ( -26.29305231718579350, 47.80000000000001137, -19.10302069950537884 ) ) ;
#2098 = CARTESIAN_POINT ( 'NONE',  ( -18.94512977948575738, 1.424999997268805441, -13.76444248337723231 ) ) ;
#2099 = CARTESIAN_POINT ( 'NONE',  ( -33.58253175000000113, 15.27500000273118985, -10.91162601494193218 ) ) ;
#2100 = CARTESIAN_POINT ( 'NONE',  ( -20.08610463437157989, 24.20000000546238184, -27.64615127144129758 ) ) ;
#2101 = CARTESIAN_POINT ( 'NONE',  ( 26.06988505166722803, 22.02045166574269075, -7.025853678916862854 ) ) ;
#2102 = CARTESIAN_POINT ( 'NONE',  ( 11.25946833292375793, 76.17500000273119554, 8.180482586598731842 ) ) ;
#2103 = CARTESIAN_POINT ( 'NONE',  ( -20.75514604977248823, 79.07500000273121543, -28.56700777964554305 ) ) ;
#2104 = DIRECTION ( 'NONE',  ( 0.000000000000000000, 0.000000000000000000, 1.000000000000000000 ) ) ;
#2105 = CARTESIAN_POINT ( 'NONE',  ( 10.37757302488624056, 72.77500000273118985, -31.93888565452638417 ) ) ;
#2106 = ORIENTED_EDGE ( 'NONE', *, *, #949, .T. ) ;
#2107 = CARTESIAN_POINT ( 'NONE',  ( 14.47279130897151589, 14.82499999726881690, 19.92008829642072953 ) ) ;
#2108 = CARTESIAN_POINT ( 'NONE',  ( 18.94512977948575738, 4.424999997268807661, 13.76444248337723408 ) ) ;
#2109 = CARTESIAN_POINT ( 'NONE',  ( -13.97622843553588901, 52.24739583333332860, 24.20753774853756823 ) ) ;
#2110 = CARTESIAN_POINT ( 'NONE',  ( 33.58253175000000113, 58.12500000273116996, -4.112674001490185761E-15 ) ) ;
#2111 = CARTESIAN_POINT ( 'NONE',  ( -20.75514604977248823, 25.07500000273120122, -28.56700777964554305 ) ) ;
#2112 = CARTESIAN_POINT ( 'NONE',  ( 33.58253175000000113, 12.47500000273119447, -10.91162601494193751 ) ) ;
#2113 = CARTESIAN_POINT ( 'NONE',  ( -24.20753774853730889, 31.90885416666666785, 13.97622843553634020 ) ) ;
#2114 = CARTESIAN_POINT ( 'NONE',  ( 7.468012846824777284, 22.31809000092397000, 28.02196122052045268 ) ) ;
#2115 = CARTESIAN_POINT ( 'NONE',  ( -30.02300923189239512, 63.13281250000000000, 2.654126918244515359E-13 ) ) ;
#2116 = CARTESIAN_POINT ( 'NONE',  ( -33.58253175000000113, 5.025000002731194293, -10.91162601494193218 ) ) ;
#2117 = CARTESIAN_POINT ( 'NONE',  ( 11.25946833292375793, 72.17500000273119554, 8.180482586598731842 ) ) ;
#2118 = CARTESIAN_POINT ( 'NONE',  ( 32.50000000000000711, 40.89999999999998437, 10.55989012756945122 ) ) ;
#2119 = CARTESIAN_POINT ( 'NONE',  ( 10.37757302488624056, 46.52500000273118985, -31.93888565452638417 ) ) ;
#2120 = CARTESIAN_POINT ( 'NONE',  ( -23.41746825000000243, 9.524999997268810858, -7.608796670333730638 ) ) ;
#2121 = VERTEX_POINT ( 'NONE', #13415 ) ;
#2122 = CARTESIAN_POINT ( 'NONE',  ( 20.75514604977249178, 52.07500000273119412, 28.56700777964553950 ) ) ;
#2123 = CARTESIAN_POINT ( 'NONE',  ( -26.29305231718579350, 4.300000005462378816, -19.10302069950537884 ) ) ;
#2124 = CARTESIAN_POINT ( 'NONE',  ( 6.950374756619721595, 39.50559000092398065, 26.09010956794232428 ) ) ;
#2125 = CARTESIAN_POINT ( 'NONE',  ( 20.75514604977248467, 76.67500000273116711, -28.56700777964554305 ) ) ;
#2126 = VERTEX_POINT ( 'NONE', #21645 ) ;
#2127 = CARTESIAN_POINT ( 'NONE',  ( -33.58253175000000113, 21.12500000273119483, 0.000000000000000000 ) ) ;
#2128 = CARTESIAN_POINT ( 'NONE',  ( -7.505752307972844761, 14.29166666666666430, 28.01184896238304134 ) ) ;
#2129 = EDGE_CURVE ( 'NONE', #12058, #1865, #8800, .T. ) ;
#2130 = ORIENTED_EDGE ( 'NONE', *, *, #28233, .F. ) ;
#2131 = CARTESIAN_POINT ( 'NONE',  ( -10.04305231718579172, 14.10000000546238219, -30.90933677959248982 ) ) ;
#2132 = CARTESIAN_POINT ( 'NONE',  ( 20.75514604977249178, 69.82500000273118701, 28.56700777964553950 ) ) ;
#2133 = CARTESIAN_POINT ( 'NONE',  ( 28.01184896238290278, 37.20833333333332860, -7.505752307973347470 ) ) ;
#2134 = CARTESIAN_POINT ( 'NONE',  ( -19.82091636218621034, 14.80000000000000782, -14.40073868116559552 ) ) ;
#2135 = DIRECTION ( 'NONE',  ( 0.000000000000000000, -1.000000000000000000, 0.000000000000000000 ) ) ;
#2136 = CARTESIAN_POINT ( 'NONE',  ( 27.16883889988623935, 10.32500000273117635, -19.73931689729374384 ) ) ;
#2137 = CARTESIAN_POINT ( 'NONE',  ( 20.08610463437158344, 28.69999999999999574, 27.64615127144129403 ) ) ;
#2138 = CARTESIAN_POINT ( 'NONE',  ( 0.04044903255045854962, 50.52305583240934794, 30.02300923189239867 ) ) ;
#2139 = CARTESIAN_POINT ( 'NONE',  ( 15.00000000000000000, 73.00000000000001421, -1.836970198721029589E-15 ) ) ;
#2140 = DIRECTION ( 'NONE',  ( 0.000000000000000000, -1.000000000000000000, 0.000000000000000000 ) ) ;
#2141 = CARTESIAN_POINT ( 'NONE',  ( 20.08610463437158344, 54.69999999999998153, 27.64615127144129403 ) ) ;
#2142 = CARTESIAN_POINT ( 'NONE',  ( -32.49999999999985789, 52.10000000000001563, 10.55989012756966083 ) ) ;
#2143 = CARTESIAN_POINT ( 'NONE',  ( 19.82091636218621034, 15.54999999453762705, 14.40073868116559730 ) ) ;
#2144 = CARTESIAN_POINT ( 'NONE',  ( 12.13525491562420910, 73.45000000546237118, -8.816778784387098611 ) ) ;
#2145 = CARTESIAN_POINT ( 'NONE',  ( 24.20753774853756113, 20.45052083333332504, 13.97622843553589789 ) ) ;
#2146 = CARTESIAN_POINT ( 'NONE',  ( 27.16883889988623935, 28.32500000273119412, -19.73931689729374384 ) ) ;
#2147 = CARTESIAN_POINT ( 'NONE',  ( 27.16883889988624290, 77.92500000273118133, 19.73931689729373673 ) ) ;
#2148 = CARTESIAN_POINT ( 'NONE',  ( -20.75514604977248112, 41.67500000273117422, 28.56700777964554661 ) ) ;
#2149 = CARTESIAN_POINT ( 'NONE',  ( -2.162160676586882350E-15, 20.87500000273119127, -35.31076352940722529 ) ) ;
#2150 = CARTESIAN_POINT ( 'NONE',  ( -10.04305231718578462, 12.90000000546237580, 30.90933677959249337 ) ) ;
#2151 = CARTESIAN_POINT ( 'NONE',  ( -20.75514604977248823, 74.82500000273115859, -28.56700777964554305 ) ) ;
#2152 = CARTESIAN_POINT ( 'NONE',  ( 19.82091636218621389, 8.200000000000013500, -14.40073868116559197 ) ) ;
#2153 =( BOUNDED_CURVE ( )  B_SPLINE_CURVE ( 2, ( #19559, #16479, #16321, #24533, #11164, #21800, #3599, #3933, #6512, #29342, #30007, #24696, #1173 ),
 .UNSPECIFIED., .F., .T. ) 
 B_SPLINE_CURVE_WITH_KNOTS ( ( 3, 2, 2, 2, 2, 2, 3 ),
 ( 0.2500000000000000000, 0.2512820512820512775, 0.2538461538461538325, 0.2564102564102563875, 0.2589743589743589980, 0.2615384615384615530, 0.2628205128205128305 ),
 .UNSPECIFIED. ) 
 CURVE ( )  GEOMETRIC_REPRESENTATION_ITEM ( )  RATIONAL_B_SPLINE_CURVE ( ( 0.9755282581475768211, 0.9755282581475768211, 1.000000000000000000, 0.9510565162951535312, 1.000000000000000000, 0.9510565162951535312, 1.000000000000000000, 0.9510565162951535312, 1.000000000000000000, 0.9510565162951535312, 1.000000000000000000, 0.9755282581475768211, 0.9755282581475768211 ) ) 
 REPRESENTATION_ITEM ( '' )  );
#2154 = CARTESIAN_POINT ( 'NONE',  ( 26.29305231718579350, 58.80000000000000426, 19.10302069950537529 ) ) ;
#2155 = CARTESIAN_POINT ( 'NONE',  ( 14.47279130897151767, 14.32499999726880624, 19.92008829642072953 ) ) ;
#2156 = CARTESIAN_POINT ( 'NONE',  ( 27.16883889988623935, 66.32500000273117280, -19.73931689729374384 ) ) ;
#2157 = CARTESIAN_POINT ( 'NONE',  ( 14.47279130897151589, 10.82499999726882756, 19.92008829642072953 ) ) ;
#2158 = CARTESIAN_POINT ( 'NONE',  ( -33.58253175000000113, 75.37500000273118417, 0.000000000000000000 ) ) ;
#2159 = CARTESIAN_POINT ( 'NONE',  ( -33.58253175000000113, 9.125000002731198379, 0.000000000000000000 ) ) ;
#2160 = CARTESIAN_POINT ( 'NONE',  ( -23.41746825000000243, 14.02499999726881263, -7.608796670333730638 ) ) ;
#2161 = CARTESIAN_POINT ( 'NONE',  ( -24.22776226481240514, 16.15923583425731636, 13.94119854578937812 ) ) ;
#2162 = ORIENTED_EDGE ( 'NONE', *, *, #22859, .F. ) ;
#2163 = CARTESIAN_POINT ( 'NONE',  ( 20.75514604977249178, 49.82500000273117990, 28.56700777964553950 ) ) ;
#2164 = ORIENTED_EDGE ( 'NONE', *, *, #33212, .F. ) ;
#2165 = CARTESIAN_POINT ( 'NONE',  ( -28.01184896238290278, 35.48958333333332860, 7.505752307973363457 ) ) ;
#2166 = DIRECTION ( 'NONE',  ( 0.000000000000000000, 0.000000000000000000, 1.000000000000000000 ) ) ;
#2167 = CARTESIAN_POINT ( 'NONE',  ( 10.04305231718579705, 3.100000005462372421, 30.90933677959248982 ) ) ;
#2168 = CARTESIAN_POINT ( 'NONE',  ( 0.000000000000000000, 52.00000000000000711, 32.50000000000000000 ) ) ;
#2169 = PRODUCT_RELATED_PRODUCT_CATEGORY ( 'part', '', ( #4952 ) ) ;
#2170 = CARTESIAN_POINT ( 'NONE',  ( -23.41746825000000243, 6.024999997268805529, -7.608796670333730638 ) ) ;
#2171 = CARTESIAN_POINT ( 'NONE',  ( -18.94512977948575738, 9.424999997268812990, -13.76444248337723231 ) ) ;
#2172 = CARTESIAN_POINT ( 'NONE',  ( -33.58253175000000113, 13.37500000273117351, 0.000000000000000000 ) ) ;
#2173 = CARTESIAN_POINT ( 'NONE',  ( 26.29305231718578995, 15.70000000546237295, -19.10302069950538240 ) ) ;
#2174 = CARTESIAN_POINT ( 'NONE',  ( 26.29305231718578995, 63.20000000000000284, -19.10302069950538240 ) ) ;
#2175 = CARTESIAN_POINT ( 'NONE',  ( 5.779280353836490358E-15, 6.500000000000002665, 32.49999999999999289 ) ) ;
#2176 = CARTESIAN_POINT ( 'NONE',  ( 32.50000000000000000, 73.50000000546236834, -3.980102097228898626E-15 ) ) ;
#2177 = CARTESIAN_POINT ( 'NONE',  ( -15.01150461594642138, 12.14322916666666430, -26.00068869287340334 ) ) ;
#2178 = CARTESIAN_POINT ( 'NONE',  ( 10.37757302488624056, 30.77500000273120051, -31.93888565452638417 ) ) ;
#2179 = CARTESIAN_POINT ( 'NONE',  ( -11.25946833292375793, 79.57500000273121543, 8.180482586598737171 ) ) ;
#2180 = CARTESIAN_POINT ( 'NONE',  ( -28.01184896238290278, 38.92708333333333570, 7.505752307973363457 ) ) ;
#2181 = CARTESIAN_POINT ( 'NONE',  ( 0.000000000000000000, 0.000000000000000000, 0.000000000000000000 ) ) ;
#2182 = CARTESIAN_POINT ( 'NONE',  ( -7.236395654485757944, 13.72499999726881015, -22.27133577429736988 ) ) ;
#2183 = CARTESIAN_POINT ( 'NONE',  ( -26.29305231718579350, 9.800000000000002487, -19.10302069950537884 ) ) ;
#2184 = CARTESIAN_POINT ( 'NONE',  ( -24.50000000000000000, 16.99999999999998579, -3.000384657911015469E-15 ) ) ;
#2185 = CARTESIAN_POINT ( 'NONE',  ( 26.09010956794244507, 56.68190999907602645, 6.950374756619249084 ) ) ;
#2186 = CARTESIAN_POINT ( 'NONE',  ( -27.16883889988624290, 52.92500000273120264, -19.73931689729374028 ) ) ;
#2187 = CARTESIAN_POINT ( 'NONE',  ( 33.58253175000000113, 64.37500000273121259, -4.112674001490185761E-15 ) ) ;
#2188 = CARTESIAN_POINT ( 'NONE',  ( -20.75514604977248112, 41.67500000273117422, 28.56700777964554661 ) ) ;
#2189 = CARTESIAN_POINT ( 'NONE',  ( -7.236395654485763274, 16.02499999726880731, 22.27133577429736633 ) ) ;
#2190 = CARTESIAN_POINT ( 'NONE',  ( 26.07999730980490227, 16.86979166666666075, 6.988114217767821046 ) ) ;
#2191 = CARTESIAN_POINT ( 'NONE',  ( -19.82091636218621034, 8.800000000000002487, -14.40073868116559552 ) ) ;
#2192 = FACE_OUTER_BOUND ( 'NONE', #4061, .T. ) ;
#2193 = CARTESIAN_POINT ( 'NONE',  ( 32.50000000000000711, 78.89999999999999147, 10.55989012756945122 ) ) ;
#2194 = CARTESIAN_POINT ( 'NONE',  ( -2.162160676586881955E-15, 14.62500000273118239, -35.31076352940723240 ) ) ;
#2195 = CARTESIAN_POINT ( 'NONE',  ( 8.601468415847516980, 80.67500000273115290, -11.83890561707634603 ) ) ;
#2196 = LINE ( 'NONE', #10278, #24858 ) ;
#2197 = CARTESIAN_POINT ( 'NONE',  ( -4.934616302121927505E-14, 70.50000000000000000, 32.50000000000000000 ) ) ;
#2198 = CARTESIAN_POINT ( 'NONE',  ( 24.18731323226221974, 15.00222249907602112, -14.01125832528328985 ) ) ;
#2199 = CARTESIAN_POINT ( 'NONE',  ( -20.08610463437157989, 42.20000000546239249, -27.64615127144129758 ) ) ;
#2200 = CARTESIAN_POINT ( 'NONE',  ( 26.29305231718578995, 11.19999999999998863, -19.10302069950538240 ) ) ;
#2201 = CARTESIAN_POINT ( 'NONE',  ( 10.37757302488624056, 24.52500000273119696, -31.93888565452638417 ) ) ;
#2202 = CARTESIAN_POINT ( 'NONE',  ( 6.988114217767829928, 33.19791666666665719, -26.07999730980489872 ) ) ;
#2203 = ORIENTED_EDGE ( 'NONE', *, *, #31596, .T. ) ;
#2204 = CARTESIAN_POINT ( 'NONE',  ( -20.75514604977248823, 66.82500000273118701, -28.56700777964554305 ) ) ;
#2205 = CARTESIAN_POINT ( 'NONE',  ( -20.50609665440969209, 48.95312500000000000, 20.50609665441005092 ) ) ;
#2206 = DIRECTION ( 'NONE',  ( 0.000000000000000000, -1.000000000000000000, 0.000000000000000000 ) ) ;
#2207 = ORIENTED_EDGE ( 'NONE', *, *, #12302, .F. ) ;
#2208 = CARTESIAN_POINT ( 'NONE',  ( 14.97647472619947351, 59.98736083425730925, 26.02091320914850314 ) ) ;
#2209 = CARTESIAN_POINT ( 'NONE',  ( -0.04044903254992426173, 56.83631916759064495, 27.95245687107223276 ) ) ;
#2210 = CARTESIAN_POINT ( 'NONE',  ( 6.486482029760649416E-15, 11.62500000273118950, 35.31076352940723240 ) ) ;
#2211 = CARTESIAN_POINT ( 'NONE',  ( -20.50609665441004736, 67.00000000000000000, -20.50609665440969565 ) ) ;
#2212 = CARTESIAN_POINT ( 'NONE',  ( 3.980102097228898626E-15, 80.00000000000001421, 32.50000000000000000 ) ) ;
#2213 = CARTESIAN_POINT ( 'NONE',  ( 10.37757302488624767, 35.97500000273118559, 31.93888565452638417 ) ) ;
#2214 = CARTESIAN_POINT ( 'NONE',  ( 10.04305231718578817, 41.90000000546237402, -30.90933677959249337 ) ) ;
#2215 = CARTESIAN_POINT ( 'NONE',  ( -12.13525491562420910, 78.19999999999998863, 8.816778784387098611 ) ) ;
#2216 = CARTESIAN_POINT ( 'NONE',  ( -26.00068869287368756, 63.41927083333333570, -15.01150461594595775 ) ) ;
#2217 = CARTESIAN_POINT ( 'NONE',  ( -33.58253175000000113, 23.12500000273118417, 0.000000000000000000 ) ) ;
#2218 = LINE ( 'NONE', #25223, #6094 ) ;
#2219 = CARTESIAN_POINT ( 'NONE',  ( -20.75514604977248112, 49.67500000273118133, 28.56700777964554661 ) ) ;
#2220 =( NAMED_UNIT ( * ) PLANE_ANGLE_UNIT ( ) SI_UNIT ( $, .RADIAN. ) );
#2221 = EDGE_CURVE ( 'NONE', #6130, #17496, #29511, .T. ) ;
#2222 = CARTESIAN_POINT ( 'NONE',  ( -20.08610463437156923, 26.29999999999998295, 27.64615127144130113 ) ) ;
#2223 = CARTESIAN_POINT ( 'NONE',  ( -26.29305231718579350, 27.79999999999999005, -19.10302069950537884 ) ) ;
#2224 = CARTESIAN_POINT ( 'NONE',  ( 23.41746825000000243, 16.52499999726882152, 7.608796670333735079 ) ) ;
#2225 = CARTESIAN_POINT ( 'NONE',  ( -2.162160676586881955E-15, 66.62500000273118417, -35.31076352940723240 ) ) ;
#2226 = CARTESIAN_POINT ( 'NONE',  ( -12.54892211412393266, 66.99999999999995737, 30.22116052075399750 ) ) ;
#2227 = CARTESIAN_POINT ( 'NONE',  ( -8.960552108402744065E-16, 74.87500000273119838, -14.63369212191046209 ) ) ;
#2228 = CARTESIAN_POINT ( 'NONE',  ( 6.486482029760648627E-15, 61.87500000273117706, 35.31076352940722529 ) ) ;
#2229 = CARTESIAN_POINT ( 'NONE',  ( 4.300734207923757602, 80.27500000273118985, -13.23629886949340673 ) ) ;
#2230 = EDGE_CURVE ( 'NONE', #17496, #8542, #20976, .T. ) ;
#2231 = EDGE_CURVE ( 'NONE', #21272, #32007, #8416, .T. ) ;
#2232 = FACE_OUTER_BOUND ( 'NONE', #1009, .T. ) ;
#2233 = CARTESIAN_POINT ( 'NONE',  ( -20.75514604977248823, 16.82500000273120122, -28.56700777964554305 ) ) ;
#2234 = CARTESIAN_POINT ( 'NONE',  ( -19.82091636218621034, 10.54999999453762349, -14.40073868116559552 ) ) ;
#2235 = CARTESIAN_POINT ( 'NONE',  ( 27.95245687107223986, 25.03944416759064495, 0.04044903254993640479 ) ) ;
#2236 = CARTESIAN_POINT ( 'NONE',  ( -11.43271046912435196, 74.02547620226849290, -9.783748258876929782 ) ) ;
#2237 = CARTESIAN_POINT ( 'NONE',  ( -33.58253175000000113, 39.22500000273119269, 10.91162601494193929 ) ) ;
#2238 = LINE ( 'NONE', #20959, #2903 ) ;
#2239 = DIRECTION ( 'NONE',  ( 0.000000000000000000, 1.000000000000000000, 0.000000000000000000 ) ) ;
#2240 = CARTESIAN_POINT ( 'NONE',  ( -28.00173670424549499, 50.96392333425730925, -7.543491769121417612 ) ) ;
#2241 = ADVANCED_FACE ( 'NONE', ( #11007 ), #7919, .T. ) ;
#2242 = LINE ( 'NONE', #25419, #32443 ) ;
#2243 = CARTESIAN_POINT ( 'NONE',  ( -15.04653450569338524, 41.64284749907602645, -25.98046417659831775 ) ) ;
#2244 = CARTESIAN_POINT ( 'NONE',  ( -20.08610463437156923, 62.80000000546237970, 27.64615127144130113 ) ) ;
#2245 = CARTESIAN_POINT ( 'NONE',  ( 8.601468415847516980, 74.67500000273120975, -11.83890561707634781 ) ) ;
#2246 = CARTESIAN_POINT ( 'NONE',  ( 32.50000000000000000, 63.00000000000000000, -3.980102097228898626E-15 ) ) ;
#2247 = CARTESIAN_POINT ( 'NONE',  ( 14.01125832528330051, 63.98659749907601935, 24.18731323226221974 ) ) ;
#2248 = CARTESIAN_POINT ( 'NONE',  ( 24.50000000000000000, 0.09999999999999682754, -7.960532557706203605 ) ) ;
#2249 = CARTESIAN_POINT ( 'NONE',  ( 20.08610463437158344, 77.20000000546238539, 27.64615127144129403 ) ) ;
#2250 = CARTESIAN_POINT ( 'NONE',  ( 2.740863092043355209E-13, 14.14843749999999289, 30.02300923189239512 ) ) ;
#2251 = VECTOR ( 'NONE', #32207, 1000.000000000000000 ) ;
#2252 = CARTESIAN_POINT ( 'NONE',  ( 10.37757302488624767, 35.97500000273119980, 31.93888565452638417 ) ) ;
#2253 = CARTESIAN_POINT ( 'NONE',  ( 14.47279130897151944, 7.424999997268819207, -19.92008829642072598 ) ) ;
#2254 = VERTEX_POINT ( 'NONE', #178 ) ;
#2255 = CARTESIAN_POINT ( 'NONE',  ( -27.16883889988623935, 73.57500000273120122, 19.73931689729374739 ) ) ;
#2256 = CARTESIAN_POINT ( 'NONE',  ( -26.29305231718579350, 26.30000000546238326, -19.10302069950537884 ) ) ;
#2257 = CARTESIAN_POINT ( 'NONE',  ( -30.02300923189239512, 39.07031249999997868, 2.654126918244515359E-13 ) ) ;
#2258 = CARTESIAN_POINT ( 'NONE',  ( -15.01150461594595775, 59.12239583333333570, 26.00068869287368756 ) ) ;
#2259 = CARTESIAN_POINT ( 'NONE',  ( -2.162160676586881955E-15, 54.87500000273119127, -35.31076352940723240 ) ) ;
#2260 = CARTESIAN_POINT ( 'NONE',  ( 32.50000000000000711, 65.40000000546237402, 10.55989012756945122 ) ) ;
#2261 = VERTEX_POINT ( 'NONE', #28849 ) ;
#2262 = FACE_OUTER_BOUND ( 'NONE', #5128, .T. ) ;
#2263 = CARTESIAN_POINT ( 'NONE',  ( -10.37757302488623701, 43.52500000273118275, 31.93888565452638417 ) ) ;
#2264 = CARTESIAN_POINT ( 'NONE',  ( -14.47279130897152122, 15.92499999726881121, 19.92008829642072243 ) ) ;
#2265 = TOROIDAL_SURFACE ( 'NONE', #29108, 12.11607355459420177, 2.000000000000000000 ) ;
#2266 = CARTESIAN_POINT ( 'NONE',  ( -33.58253175000000113, 69.37500000273119838, 0.000000000000000000 ) ) ;
#2267 = CARTESIAN_POINT ( 'NONE',  ( -26.29305231718578995, 6.700000005462392494, 19.10302069950538595 ) ) ;
#2268 = CARTESIAN_POINT ( 'NONE',  ( 10.37757302488624056, 58.52500000273118275, -31.93888565452638417 ) ) ;
#2269 = CARTESIAN_POINT ( 'NONE',  ( -1.778240108872766143E-15, 50.00000000546237544, -32.49999999999999289 ) ) ;
#2270 = CARTESIAN_POINT ( 'NONE',  ( -20.08610463437157989, 49.70000000000000284, -27.64615127144129758 ) ) ;
#2271 = CARTESIAN_POINT ( 'NONE',  ( 18.94512977948576093, 0.8249999972688160099, -13.76444248337722875 ) ) ;
#2272 = CARTESIAN_POINT ( 'NONE',  ( -2.162160676586881955E-15, 12.87500000273117884, -35.31076352940723240 ) ) ;
#2273 = CARTESIAN_POINT ( 'NONE',  ( -3.880418787951136483, 6.551254281546842861, -24.50000000000000000 ) ) ;
#2274 = CARTESIAN_POINT ( 'NONE',  ( 13.94119854578893580, 21.59076416574269430, -24.22776226481265383 ) ) ;
#2275 = CARTESIAN_POINT ( 'NONE',  ( 11.25946833292375793, 80.17500000273119554, 8.180482586598731842 ) ) ;
#2276 = CARTESIAN_POINT ( 'NONE',  ( -20.75514604977248112, 77.67500000273119554, 28.56700777964554661 ) ) ;
#2277 = CARTESIAN_POINT ( 'NONE',  ( 5.779280353836490358E-15, 44.49999999999999289, 32.49999999999999289 ) ) ;
#2278 = CARTESIAN_POINT ( 'NONE',  ( 27.16883889988624290, 72.17500000273118133, 19.73931689729373673 ) ) ;
#2279 = EDGE_LOOP ( 'NONE', ( #16616, #14323, #15089, #592 ) ) ;
#2280 = CARTESIAN_POINT ( 'NONE',  ( 23.41746824999999887, 11.12499999726881938, 0.000000000000000000 ) ) ;
#2281 = CARTESIAN_POINT ( 'NONE',  ( 18.94512977948576093, 4.824999997268819563, -13.76444248337722875 ) ) ;
#2282 = CARTESIAN_POINT ( 'NONE',  ( 26.07999730980477437, 54.39583333333332860, -6.988114217768290004 ) ) ;
#2283 = CARTESIAN_POINT ( 'NONE',  ( -27.16883889988623935, 61.32500000273120833, 19.73931689729374739 ) ) ;
#2284 = CARTESIAN_POINT ( 'NONE',  ( -33.58253175000000113, 17.37500000273119127, 0.000000000000000000 ) ) ;
#2285 = CARTESIAN_POINT ( 'NONE',  ( -33.58253175000000113, 11.47500000273119625, 10.91162601494193929 ) ) ;
#2286 = CARTESIAN_POINT ( 'NONE',  ( -2.428612866367529427E-13, 33.05468750000000000, -27.95245687107223276 ) ) ;
#2287 = PRODUCT_DEFINITION_CONTEXT ( 'detailed design', #5501, 'design' ) ;
#2288 = CARTESIAN_POINT ( 'NONE',  ( 28.02196122052045268, 18.02121500092397710, -7.468012846824774620 ) ) ;
#2289 = CARTESIAN_POINT ( 'NONE',  ( 26.00068869287367335, 65.13802083333334281, 15.01150461594596308 ) ) ;
#2290 = CARTESIAN_POINT ( 'NONE',  ( -10.37757302488624411, 4.725000002731183812, -31.93888565452638417 ) ) ;
#2291 = ADVANCED_FACE ( 'NONE', ( #13746 ), #401, .F. ) ;
#2292 = CARTESIAN_POINT ( 'NONE',  ( -8.601468415847518756, 73.07500000273115859, -11.83890561707634603 ) ) ;
#2293 = CARTESIAN_POINT ( 'NONE',  ( -20.08610463437157989, 39.70000000000000284, -27.64615127144129758 ) ) ;
#2294 = AXIS2_PLACEMENT_3D ( 'NONE', #9518, #16753, #24632 ) ;
#2295 = CARTESIAN_POINT ( 'NONE',  ( 6.486482029760648627E-15, 47.62500000273118417, 35.31076352940722529 ) ) ;
#2296 = CARTESIAN_POINT ( 'NONE',  ( -14.47279130897151589, 11.32499999726881157, -19.92008829642072598 ) ) ;
#2297 = FACE_OUTER_BOUND ( 'NONE', #130, .T. ) ;
#2298 = ORIENTED_EDGE ( 'NONE', *, *, #30160, .T. ) ;
#2299 = CARTESIAN_POINT ( 'NONE',  ( 10.37757302488624056, 56.77500000273121117, -31.93888565452638417 ) ) ;
#2300 = CARTESIAN_POINT ( 'NONE',  ( 1.093617666956751375E-13, 60.00000000546238255, -32.50000000000000711 ) ) ;
#2301 = CARTESIAN_POINT ( 'NONE',  ( -19.11951029504763611, 40.07850666759064495, 19.06425588902592239 ) ) ;
#2302 = CARTESIAN_POINT ( 'NONE',  ( 20.75514604977248467, 74.67500000273118133, -28.56700777964554305 ) ) ;
#2303 = ORIENTED_EDGE ( 'NONE', *, *, #8928, .F. ) ;
#2304 = CARTESIAN_POINT ( 'NONE',  ( 27.16883889988624290, 25.92500000273119554, 19.73931689729373673 ) ) ;
#2305 = CARTESIAN_POINT ( 'NONE',  ( 28.01184896238304134, 20.30729166666666430, 7.505752307972846538 ) ) ;
#2306 = ORIENTED_EDGE ( 'NONE', *, *, #4748, .F. ) ;
#2307 = CARTESIAN_POINT ( 'NONE',  ( 32.50000000000000000, 29.60000000546238041, -10.55989012756945833 ) ) ;
#2308 = CARTESIAN_POINT ( 'NONE',  ( 27.16883889988624290, 63.92500000273118843, 19.73931689729373673 ) ) ;
#2309 = CARTESIAN_POINT ( 'NONE',  ( 15.01150461594643204, 37.92447916666666430, 26.00068869287340334 ) ) ;
#2310 = CARTESIAN_POINT ( 'NONE',  ( -15.14183272437242600, 17.30000000000000782, 20.84094480462497856 ) ) ;
#2311 = CARTESIAN_POINT ( 'NONE',  ( 3.980102097228898626E-15, 80.00000000000001421, 32.50000000000000000 ) ) ;
#2312 = CARTESIAN_POINT ( 'NONE',  ( 33.58253175000000113, 6.125000002731195714, -4.112674001490185761E-15 ) ) ;
#2313 = DIRECTION ( 'NONE',  ( 0.000000000000000000, 0.000000000000000000, 1.000000000000000000 ) ) ;
#2314 = CARTESIAN_POINT ( 'NONE',  ( -0.04044903255044120238, 52.24180583240936215, -30.02300923189239867 ) ) ;
#2315 = CARTESIAN_POINT ( 'NONE',  ( -4.635254915624211769, 75.59999999999999432, -14.26584774442730286 ) ) ;
#2316 = CARTESIAN_POINT ( 'NONE',  ( 9.270509831248425314, 80.69999999999998863, 12.75976212528059683 ) ) ;
#2317 = CARTESIAN_POINT ( 'NONE',  ( -1.137977401836464321E-14, 66.99999999999998579, 46.18802153517007270 ) ) ;
#2318 = CARTESIAN_POINT ( 'NONE',  ( 26.29305231718579350, 16.79999999999999716, 19.10302069950537529 ) ) ;
#2319 = CARTESIAN_POINT ( 'NONE',  ( -15.14183272437242600, 13.04999999453763770, 20.84094480462497856 ) ) ;
#2320 = CARTESIAN_POINT ( 'NONE',  ( 12.13525491562420910, 71.45000000546237118, -8.816778784387098611 ) ) ;
#2321 = CARTESIAN_POINT ( 'NONE',  ( 6.988114217767829928, 22.88541666666666430, -26.07999730980489872 ) ) ;
#2322 = CARTESIAN_POINT ( 'NONE',  ( 10.37757302488624767, 31.72500000273117848, 31.93888565452638417 ) ) ;
#2323 = CARTESIAN_POINT ( 'NONE',  ( 10.37757302488624056, 76.52500000273120406, -31.93888565452638417 ) ) ;
#2324 = CARTESIAN_POINT ( 'NONE',  ( 33.58253175000000113, 36.47500000273119269, -10.91162601494193751 ) ) ;
#2325 = CARTESIAN_POINT ( 'NONE',  ( 33.58253175000000113, 24.37500000273118417, -4.112674001490185761E-15 ) ) ;
#2326 = CARTESIAN_POINT ( 'NONE',  ( -32.50000000000000000, 64.00000000000000000, 0.000000000000000000 ) ) ;
#2327 = CARTESIAN_POINT ( 'NONE',  ( -10.04305231718579172, 26.10000000546236620, -30.90933677959248982 ) ) ;
#2328 = CARTESIAN_POINT ( 'NONE',  ( -32.50000000000000000, 59.99999999999998579, 0.000000000000000000 ) ) ;
#2329 = AXIS2_PLACEMENT_3D ( 'NONE', #5294, #29129, #33951 ) ;
#2330 = CARTESIAN_POINT ( 'NONE',  ( 18.94512977948575738, 18.42499999726882010, 13.76444248337723408 ) ) ;
#2331 = CARTESIAN_POINT ( 'NONE',  ( 10.37757302488624056, 66.52500000273120406, -31.93888565452638417 ) ) ;
#2332 = EDGE_CURVE ( 'NONE', #6218, #23029, #17197, .T. ) ;
#2333 = AXIS2_PLACEMENT_3D ( 'NONE', #21565, #16419, #19157 ) ;
#2334 = CARTESIAN_POINT ( 'NONE',  ( -7.236395654485757944, 5.724999997268803931, -22.27133577429736988 ) ) ;
#2335 = CARTESIAN_POINT ( 'NONE',  ( -33.58253175000000113, 75.47500000273116427, 10.91162601494193929 ) ) ;
#2336 = CARTESIAN_POINT ( 'NONE',  ( -10.37757302488623701, 5.525000002731205839, 31.93888565452638417 ) ) ;
#2337 = CARTESIAN_POINT ( 'NONE',  ( 18.94512977948576093, 2.824999997268817786, -13.76444248337722875 ) ) ;
#2338 = CARTESIAN_POINT ( 'NONE',  ( 26.06988505166735592, 11.43267333425730925, 7.025853678916393896 ) ) ;
#2339 = ORIENTED_EDGE ( 'NONE', *, *, #18402, .F. ) ;
#2340 = CARTESIAN_POINT ( 'NONE',  ( 27.16883889988624290, 43.92500000273118133, 19.73931689729373673 ) ) ;
#2341 = ORIENTED_EDGE ( 'NONE', *, *, #33551, .T. ) ;
#2342 = ORIENTED_EDGE ( 'NONE', *, *, #24940, .F. ) ;
#2343 = CARTESIAN_POINT ( 'NONE',  ( 30.02300923189239512, 44.22656249999997868, -2.619432448724977703E-13 ) ) ;
#2344 = CARTESIAN_POINT ( 'NONE',  ( 24.50000000000000000, 19.74999999453763877, 0.000000000000000000 ) ) ;
#2345 = CARTESIAN_POINT ( 'NONE',  ( 26.29305231718578995, 1.700000005462373842, -19.10302069950538240 ) ) ;
#2346 = CARTESIAN_POINT ( 'NONE',  ( -18.94512977948576093, 4.324999997268818674, 13.76444248337722698 ) ) ;
#2347 = CARTESIAN_POINT ( 'NONE',  ( 7.236395654485760609, 15.02499999726880731, -22.27133577429736633 ) ) ;
#2348 = CARTESIAN_POINT ( 'NONE',  ( 10.37757302488624056, 16.77500000273118985, -31.93888565452638417 ) ) ;
#2349 = CARTESIAN_POINT ( 'NONE',  ( -10.04305231718579172, 20.10000000546238752, -30.90933677959248982 ) ) ;
#2350 = AXIS2_PLACEMENT_3D ( 'NONE', #3763, #24691, #6833 ) ;
#2351 = CARTESIAN_POINT ( 'NONE',  ( 10.04305231718579705, 66.59999999999999432, 30.90933677959248982 ) ) ;
#2352 = DIRECTION ( 'NONE',  ( 0.000000000000000000, -0.000000000000000000, 1.000000000000000000 ) ) ;
#2353 = CYLINDRICAL_SURFACE ( 'NONE', #25262, 32.50000000000000000 ) ;
#2354 = CARTESIAN_POINT ( 'NONE',  ( 20.53372385742072481, 62.42225666759065206, -20.47846945139902175 ) ) ;
#2355 = CARTESIAN_POINT ( 'NONE',  ( 15.01150461594596486, 40.21614583333332860, -26.00068869287367690 ) ) ;
#2356 = APPLICATION_PROTOCOL_DEFINITION ( 'draft international standard', 'automotive_design', 1998, #21934 ) ;
#2357 = CIRCLE ( 'NONE', #6728, 12.11607355459420354 ) ;
#2358 = CARTESIAN_POINT ( 'NONE',  ( 1.555960095263670572E-15, 16.24999999453762101, -24.50000000000000000 ) ) ;
#2359 = CARTESIAN_POINT ( 'NONE',  ( 1.507698388325705758E-15, 17.62499999726881938, -24.62258325217400312 ) ) ;
#2360 = CARTESIAN_POINT ( 'NONE',  ( -32.50000000000000000, 7.900000000000012790, -10.55989012756945478 ) ) ;
#2361 = CARTESIAN_POINT ( 'NONE',  ( -2.375766604868045029, 73.55125428154683220, -14.99999999999999822 ) ) ;
#2362 = CARTESIAN_POINT ( 'NONE',  ( -24.22776226481266448, 48.23138916574269786, -13.94119854578892514 ) ) ;
#2363 =( BOUNDED_CURVE ( )  B_SPLINE_CURVE ( 2, ( #13188, #18355, #10283, #28626, #33609, #31373, #18183, #21097, #18523, #26063, #20762, #7864, #15432 ),
 .UNSPECIFIED., .F., .T. ) 
 B_SPLINE_CURVE_WITH_KNOTS ( ( 3, 2, 2, 2, 2, 2, 3 ),
 ( 0.8611111111111111605, 0.8666666666666666963, 0.8777777777777777679, 0.8888888888888888395, 0.9000000000000000222, 0.9111111111111110938, 0.9166666666666666297 ),
 .UNSPECIFIED. ) 
 CURVE ( )  GEOMETRIC_REPRESENTATION_ITEM ( )  RATIONAL_B_SPLINE_CURVE ( ( 0.9755282581475768211, 0.9755282581475770431, 1.000000000000000000, 0.9510565162951535312, 1.000000000000000000, 0.9510565162951535312, 1.000000000000000000, 0.9510565162951535312, 1.000000000000000000, 0.9510565162951535312, 1.000000000000000000, 0.9755282581475770431, 0.9755282581475768211 ) ) 
 REPRESENTATION_ITEM ( '' )  );
#2364 = CARTESIAN_POINT ( 'NONE',  ( -33.58253175000000113, 51.12500000273117706, 0.000000000000000000 ) ) ;
#2365 = CARTESIAN_POINT ( 'NONE',  ( 20.75514604977249178, 60.07500000273119412, 28.56700777964553950 ) ) ;
#2366 = CARTESIAN_POINT ( 'NONE',  ( 33.58253175000000823, 38.27500000273119696, 10.91162601494192685 ) ) ;
#2367 = FACE_OUTER_BOUND ( 'NONE', #33613, .T. ) ;
#2368 = B_SPLINE_CURVE_WITH_KNOTS ( 'NONE', 3,
 ( #13729, #11643, #22127, #32240, #9070, #31901, #19550, #16976, #29653, #32403, #8396, #16642, #994, #6333, #18883, #11479, #13569, #5833, #16471, #3259, #24196, #29491, #666, #5995, #12148, #30852, #4260, #25546, #32737, #25195, #27947, #25025 ),
 .UNSPECIFIED., .F., .F.,
 ( 4, 2, 2, 2, 2, 2, 2, 2, 2, 2, 2, 2, 2, 2, 2, 4 ),
 ( 0.000000000000000000, 0.002298871809599534188, 0.004597743619199068377, 0.006896615428798602565, 0.009195487238398136753, 0.01149435904799767094, 0.01379323085759720513, 0.01609210266719673932, 0.01839097447679627351, 0.02298871809599534188, 0.02528758990559487607, 0.02758646171519441026, 0.02988533352479394445, 0.03218420533439347864, 0.03448307714399301283, 0.03678194895359254701 ),
 .UNSPECIFIED. ) ;
#2369 = CARTESIAN_POINT ( 'NONE',  ( 13.97622843553633842, 17.29947916666666430, 24.20753774853730889 ) ) ;
#2370 = CARTESIAN_POINT ( 'NONE',  ( 23.95873412499999944, 1.437499995903229744, 0.000000000000000000 ) ) ;
#2371 = DIRECTION ( 'NONE',  ( -1.000000000000000000, 0.000000000000000000, 0.000000000000000000 ) ) ;
#2372 = CARTESIAN_POINT ( 'NONE',  ( -27.16883889988624290, 16.92500000273118488, -19.73931689729374028 ) ) ;
#2373 = CARTESIAN_POINT ( 'NONE',  ( -32.50000000000000000, 78.50000000546236834, 0.000000000000000000 ) ) ;
#2374 = DIRECTION ( 'NONE',  ( -0.000000000000000000, 1.000000000000000000, -0.000000000000000000 ) ) ;
#2375 = CARTESIAN_POINT ( 'NONE',  ( 3.880418787951172011, 11.55125428154683576, 24.49999999999998579 ) ) ;
#2376 = CARTESIAN_POINT ( 'NONE',  ( 24.22776226481265383, 19.01263916574269075, 13.94119854578893580 ) ) ;
#2377 = EDGE_CURVE ( 'NONE', #17974, #13948, #20725, .T. ) ;
#2378 = CARTESIAN_POINT ( 'NONE',  ( 10.04305231718578817, 35.90000000546238113, -30.90933677959249337 ) ) ;
#2379 = EDGE_CURVE ( 'NONE', #7355, #7743, #13581, .T. ) ;
#2380 = CARTESIAN_POINT ( 'NONE',  ( -26.29305231718578995, 66.19999999999998863, 19.10302069950538595 ) ) ;
#2381 = CARTESIAN_POINT ( 'NONE',  ( 6.486482029760648627E-15, 27.62500000273118062, 35.31076352940722529 ) ) ;
#2382 = CARTESIAN_POINT ( 'NONE',  ( -13.97622843553632421, 43.08072916666666430, -24.20753774853731599 ) ) ;
#2383 = AXIS2_PLACEMENT_3D ( 'NONE', #26930, #10991, #16152 ) ;
#2384 = VERTEX_POINT ( 'NONE', #3778 ) ;
#2385 = CARTESIAN_POINT ( 'NONE',  ( 27.16883889988624290, 59.92500000273119554, 19.73931689729373673 ) ) ;
#2386 = CARTESIAN_POINT ( 'NONE',  ( 15.01150461594643204, 44.79947916666667140, 26.00068869287340334 ) ) ;
#2387 = ORIENTED_EDGE ( 'NONE', *, *, #22718, .T. ) ;
#2388 = CARTESIAN_POINT ( 'NONE',  ( -25.98046417659859486, 61.41965250092398776, -15.04653450569291628 ) ) ;
#2389 = CARTESIAN_POINT ( 'NONE',  ( -24.22776226481240514, 60.84673583425731636, 13.94119854578937812 ) ) ;
#2390 = ORIENTED_EDGE ( 'NONE', *, *, #16303, .F. ) ;
#2391 = CARTESIAN_POINT ( 'NONE',  ( 33.58253175000000113, 14.22500000273119625, -10.91162601494193751 ) ) ;
#2392 = CARTESIAN_POINT ( 'NONE',  ( -28.00173670424535644, 20.30170166574269075, 7.543491769121936308 ) ) ;
#2393 = DIRECTION ( 'NONE',  ( -0.000000000000000000, 1.000000000000000000, -0.000000000000000000 ) ) ;
#2394 = CARTESIAN_POINT ( 'NONE',  ( -33.58253175000000113, 33.47500000273119269, 10.91162601494193929 ) ) ;
#2395 = CARTESIAN_POINT ( 'NONE',  ( 32.50000000000000000, 37.50000000546238255, -3.980102097228898626E-15 ) ) ;
#2396 = EDGE_CURVE ( 'NONE', #3518, #19128, #27625, .T. ) ;
#2397 = CARTESIAN_POINT ( 'NONE',  ( 9.270509831248425314, 76.70000000000003126, 12.75976212528059683 ) ) ;
#2398 = CARTESIAN_POINT ( 'NONE',  ( -20.50609665441004736, 67.00000000000000000, -20.50609665440969565 ) ) ;
#2399 = CARTESIAN_POINT ( 'NONE',  ( 10.37757302488624767, 23.72500000273119980, 31.93888565452638417 ) ) ;
#2400 = CARTESIAN_POINT ( 'NONE',  ( 32.50000000000000000, 77.09999999999998010, -10.55989012756945833 ) ) ;
#2401 = CARTESIAN_POINT ( 'NONE',  ( -2.162160676586881955E-15, 48.87500000273117706, -35.31076352940723240 ) ) ;
#2402 = SURFACE_SIDE_STYLE ('',( #5653 ) ) ;
#2403 = CARTESIAN_POINT ( 'NONE',  ( -32.50000000000000000, 27.89999999999999147, -10.55989012756945478 ) ) ;
#2404 = CARTESIAN_POINT ( 'NONE',  ( 26.29305231718578995, 27.20000000000000284, -19.10302069950538240 ) ) ;
#2405 = CARTESIAN_POINT ( 'NONE',  ( 15.14183272437241889, 5.699999999999993960, 20.84094480462498211 ) ) ;
#2406 = CARTESIAN_POINT ( 'NONE',  ( -27.16883889988623935, 67.32500000273117280, 19.73931689729374739 ) ) ;
#2407 = CARTESIAN_POINT ( 'NONE',  ( -32.87414713444680103, 67.00000000000000000, -6.322578566051472393 ) ) ;
#2408 = AXIS2_PLACEMENT_3D ( 'NONE', #21011, #215, #25978 ) ;
#2409 = CARTESIAN_POINT ( 'NONE',  ( 4.300734207923757602, 74.77500000273118985, -13.23629886949340673 ) ) ;
#2410 = CARTESIAN_POINT ( 'NONE',  ( -10.37757302488623701, 61.77500000273117564, 31.93888565452638417 ) ) ;
#2411 = VECTOR ( 'NONE', #14860, 1000.000000000000000 ) ;
#2412 = CARTESIAN_POINT ( 'NONE',  ( 32.50000000000000711, 7.400000005462386454, 10.55989012756945122 ) ) ;
#2413 = CARTESIAN_POINT ( 'NONE',  ( 10.37757302488624767, 13.72500000273119092, 31.93888565452638417 ) ) ;
#2414 = CARTESIAN_POINT ( 'NONE',  ( 27.95245687107223986, 31.91444416759064495, 0.04044903254993640479 ) ) ;
#2415 = CARTESIAN_POINT ( 'NONE',  ( 19.82091636218621389, 1.949999994537626735, -14.40073868116559197 ) ) ;
#2416 = CARTESIAN_POINT ( 'NONE',  ( -10.37757302488624411, 34.72500000273119269, -31.93888565452638417 ) ) ;
#2417 = PLANE ( 'NONE',  #7272 ) ;
#2418 = FACE_OUTER_BOUND ( 'NONE', #11699, .T. ) ;
#2419 = CARTESIAN_POINT ( 'NONE',  ( -8.601468415847515203, 79.17500000273116711, 11.83890561707634959 ) ) ;
#2420 = CARTESIAN_POINT ( 'NONE',  ( 20.47846945139867003, 49.23399333240936215, -20.53372385742107653 ) ) ;
#2421 = CARTESIAN_POINT ( 'NONE',  ( -20.08610463437157989, 52.20000000546236407, -27.64615127144129758 ) ) ;
#2422 = CARTESIAN_POINT ( 'NONE',  ( -11.25946833292375793, 75.57500000273120122, 8.180482586598737171 ) ) ;
#2423 = CARTESIAN_POINT ( 'NONE',  ( 5.147494310547481966, 61.44874571845315359, -32.49999999999998579 ) ) ;
#2424 = CARTESIAN_POINT ( 'NONE',  ( -13.97622843553632421, 15.58072916666666607, -24.20753774853731599 ) ) ;
#2425 = CARTESIAN_POINT ( 'NONE',  ( 26.29305231718579350, 63.30000000546237260, 19.10302069950537529 ) ) ;
#2426 = CARTESIAN_POINT ( 'NONE',  ( -20.08610463437157989, 78.20000000546235697, -27.64615127144129758 ) ) ;
#2427 = CARTESIAN_POINT ( 'NONE',  ( -28.01184896238304134, 22.02604166666666430, -7.505752307972844761 ) ) ;
#2428 = CARTESIAN_POINT ( 'NONE',  ( 33.58253175000000823, 32.27500000273117564, 10.91162601494192863 ) ) ;
#2429 = CARTESIAN_POINT ( 'NONE',  ( 23.41746824999999887, 9.024999997268826846, 7.608796670333735079 ) ) ;
#2430 = VERTEX_POINT ( 'NONE', #11664 ) ;
#2431 = CARTESIAN_POINT ( 'NONE',  ( 20.75514604977249178, 78.07500000273117280, 28.56700777964553950 ) ) ;
#2432 = CARTESIAN_POINT ( 'NONE',  ( 32.50000000000000000, 21.60000000546237331, -10.55989012756945833 ) ) ;
#2433 = EDGE_CURVE ( 'NONE', #28550, #7938, #3992, .T. ) ;
#2434 = CARTESIAN_POINT ( 'NONE',  ( -15.01150461594595775, 45.37239583333333570, 26.00068869287368756 ) ) ;
#2435 = CARTESIAN_POINT ( 'NONE',  ( 26.00068869287367335, 61.70052083333331439, 15.01150461594596308 ) ) ;
#2436 = CARTESIAN_POINT ( 'NONE',  ( -33.58253175000000113, 55.47500000273119980, 10.91162601494193929 ) ) ;
#2437 = CARTESIAN_POINT ( 'NONE',  ( -32.50000000000000000, 56.60000000546236976, 10.55989012756946366 ) ) ;
#2438 = FACE_OUTER_BOUND ( 'NONE', #21729, .T. ) ;
#2439 = CARTESIAN_POINT ( 'NONE',  ( 27.16883889988623935, 40.32500000273120122, -19.73931689729374384 ) ) ;
#2440 = CARTESIAN_POINT ( 'NONE',  ( -4.635254915624208216, 76.65000000546234560, 14.26584774442730463 ) ) ;
#2441 = CARTESIAN_POINT ( 'NONE',  ( -33.58253175000000113, 67.27500000273117564, -10.91162601494193218 ) ) ;
#2442 = CARTESIAN_POINT ( 'NONE',  ( 10.04305231718579705, 3.100000005462372421, 30.90933677959248982 ) ) ;
#2443 = ADVANCED_FACE ( 'NONE', ( #22312 ), #9419, .T. ) ;
#2444 = CARTESIAN_POINT ( 'NONE',  ( -20.75514604977248823, 58.82500000273117990, -28.56700777964554305 ) ) ;
#2445 = CARTESIAN_POINT ( 'NONE',  ( 0.000000000000000000, 80.00000000000001421, 0.000000000000000000 ) ) ;
#2446 = CARTESIAN_POINT ( 'NONE',  ( -32.50000000000000000, 44.10000000000000142, 10.55989012756946366 ) ) ;
#2447 = LINE ( 'NONE', #10176, #26928 ) ;
#2448 = CARTESIAN_POINT ( 'NONE',  ( 10.37757302488624767, 13.97500000273119092, 31.93888565452638417 ) ) ;
#2449 = CARTESIAN_POINT ( 'NONE',  ( -26.29305231718578995, 74.19999999999998863, 19.10302069950538595 ) ) ;
#2450 = CARTESIAN_POINT ( 'NONE',  ( -19.06425588902558133, 37.20274333240935505, 19.11951029504797006 ) ) ;
#2451 = CARTESIAN_POINT ( 'NONE',  ( -13.91746824999999532, 77.27500000273117564, -4.522059556121115875 ) ) ;
#2452 = CARTESIAN_POINT ( 'NONE',  ( 20.75514604977249178, 78.07500000273118701, 28.56700777964553950 ) ) ;
#2453 = DIRECTION ( 'NONE',  ( 0.2588190451025257355, -0.9659258262890668689, 0.000000000000000000 ) ) ;
#2454 = CARTESIAN_POINT ( 'NONE',  ( -2.162160676586881955E-15, 76.87500000273115575, -35.31076352940723240 ) ) ;
#2455 = ORIENTED_EDGE ( 'NONE', *, *, #27322, .T. ) ;
#2456 = CARTESIAN_POINT ( 'NONE',  ( -23.41746825000000598, 12.22499999726881370, 7.608796670333726198 ) ) ;
#2457 = CARTESIAN_POINT ( 'NONE',  ( 14.47279130897151944, 2.924999997268816099, -19.92008829642072598 ) ) ;
#2458 = CARTESIAN_POINT ( 'NONE',  ( -2.428612866367529427E-13, 57.11718750000000711, -27.95245687107222921 ) ) ;
#2459 = CARTESIAN_POINT ( 'NONE',  ( -33.58253175000000113, 57.02500000273118275, -10.91162601494193218 ) ) ;
#2460 = CARTESIAN_POINT ( 'NONE',  ( 33.58253175000000823, 20.27500000273117564, 10.91162601494192863 ) ) ;
#2461 = CARTESIAN_POINT ( 'NONE',  ( 33.58253175000000823, 4.275000002731189852, 10.91162601494192863 ) ) ;
#2462 = CARTESIAN_POINT ( 'NONE',  ( -6.988114217767819270, 41.79166666666666430, 26.07999730980490583 ) ) ;
#2463 = CARTESIAN_POINT ( 'NONE',  ( 28.02196122052045268, 24.89621500092397710, -7.468012846824774620 ) ) ;
#2464 = CARTESIAN_POINT ( 'NONE',  ( 26.02091320914876960, 19.01263916574269075, 14.97647472619900455 ) ) ;
#2465 = CARTESIAN_POINT ( 'NONE',  ( 20.75514604977248467, 4.425000002731183990, -28.56700777964554305 ) ) ;
#2466 =( BOUNDED_CURVE ( )  B_SPLINE_CURVE ( 2, ( #11820, #6338, #3594, #16981, #9235, #14068, #29337, #13733, #5839, #24529, #11484, #14236, #8904 ),
 .UNSPECIFIED., .F., .T. ) 
 B_SPLINE_CURVE_WITH_KNOTS ( ( 3, 2, 2, 2, 2, 2, 3 ),
 ( 0.2371794871794871973, 0.2384615384615384748, 0.2410256410256410298, 0.2435897435897435848, 0.2461538461538461675, 0.2487179487179487225, 0.2500000000000000000 ),
 .UNSPECIFIED. ) 
 CURVE ( )  GEOMETRIC_REPRESENTATION_ITEM ( )  RATIONAL_B_SPLINE_CURVE ( ( 0.9755282581475768211, 0.9755282581475770431, 1.000000000000000000, 0.9510565162951535312, 1.000000000000000000, 0.9510565162951535312, 1.000000000000000000, 0.9510565162951535312, 1.000000000000000000, 0.9510565162951535312, 1.000000000000000000, 0.9755282581475768211, 0.9755282581475768211 ) ) 
 REPRESENTATION_ITEM ( '' )  );
#2467 = CYLINDRICAL_SURFACE ( 'NONE', #158, 32.50000000000000000 ) ;
#2468 = CARTESIAN_POINT ( 'NONE',  ( 20.75514604977249178, 43.82500000273119412, 28.56700777964553950 ) ) ;
#2469 = CARTESIAN_POINT ( 'NONE',  ( 7.236395654485760609, 7.024999997268826846, -22.27133577429736633 ) ) ;
#2470 = PRODUCT_DEFINITION_SHAPE ( 'NONE', 'NONE',  #33992 ) ;
#2471 = DIRECTION ( 'NONE',  ( 0.000000000000000000, 0.000000000000000000, -1.000000000000000000 ) ) ;
#2472 = ORIENTED_EDGE ( 'NONE', *, *, #1363, .F. ) ;
#2473 = CARTESIAN_POINT ( 'NONE',  ( -10.37757302488623701, 53.77500000273120406, 31.93888565452638417 ) ) ;
#2474 = CARTESIAN_POINT ( 'NONE',  ( 32.50000000000000711, 59.40000000546237402, 10.55989012756945122 ) ) ;
#2475 = CARTESIAN_POINT ( 'NONE',  ( -26.06988505166735237, 40.65142333425730214, -7.025853678916388567 ) ) ;
#2476 = CARTESIAN_POINT ( 'NONE',  ( -10.37757302488624411, 72.97500000273119269, -31.93888565452638417 ) ) ;
#2477 = ORIENTED_EDGE ( 'NONE', *, *, #6511, .T. ) ;
#2478 = CARTESIAN_POINT ( 'NONE',  ( 20.75514604977248467, 26.42500000273118843, -28.56700777964554305 ) ) ;
#2479 = CARTESIAN_POINT ( 'NONE',  ( -28.01184896238304134, 18.58854166666666430, -7.505752307972844761 ) ) ;
#2480 = COLOUR_RGB ( '', 0.66274510, 0.83137255, 0.94901961) ;
#2481 = EDGE_LOOP ( 'NONE', ( #22705, #4855, #29179, #20689 ) ) ;
#2482 = CARTESIAN_POINT ( 'NONE',  ( -10.04305231718578462, 58.39999999999999147, 30.90933677959249337 ) ) ;
#2483 = CARTESIAN_POINT ( 'NONE',  ( 20.75514604977248467, 62.42500000273118133, -28.56700777964554305 ) ) ;
#2484 = CARTESIAN_POINT ( 'NONE',  ( -15.01150461594595775, 48.80989583333332860, 26.00068869287368756 ) ) ;
#2485 = CYLINDRICAL_SURFACE ( 'NONE', #26189, 30.00000000000000000 ) ;
#2486 = CARTESIAN_POINT ( 'NONE',  ( 7.236395654485755280, 2.724999997268801266, 22.27133577429736988 ) ) ;
#2487 = CARTESIAN_POINT ( 'NONE',  ( -10.37757302488623701, 3.525000002731204507, 31.93888565452638417 ) ) ;
#2488 = CARTESIAN_POINT ( 'NONE',  ( 7.543491769121922985, 60.69232666574269075, 28.00173670424535644 ) ) ;
#2489 = CARTESIAN_POINT ( 'NONE',  ( 33.58253175000000113, 78.37500000273116996, -4.112674001490185761E-15 ) ) ;
#2490 = CARTESIAN_POINT ( 'NONE',  ( -20.50609665441004736, 67.00000000000000000, -20.50609665440969565 ) ) ;
#2491 = CARTESIAN_POINT ( 'NONE',  ( -10.04305231718579172, 69.59999999999999432, -30.90933677959248982 ) ) ;
#2492 = CARTESIAN_POINT ( 'NONE',  ( 6.277390505771533514E-15, 16.50000000000000000, 34.17252228774368916 ) ) ;
#2493 = CARTESIAN_POINT ( 'NONE',  ( -13.97622843553632777, 56.83072916666665719, -24.20753774853731599 ) ) ;
#2494 = CARTESIAN_POINT ( 'NONE',  ( 7.570916362186213000, 14.14999999453761603, -23.30088464923126423 ) ) ;
#2495 = CARTESIAN_POINT ( 'NONE',  ( -12.13525491562420910, 72.45000000546237118, 8.816778784387098611 ) ) ;
#2496 = CARTESIAN_POINT ( 'NONE',  ( 13.97622843553589966, 26.46614583333332149, -24.20753774853756113 ) ) ;
#2497 = CARTESIAN_POINT ( 'NONE',  ( -2.162160676586881955E-15, 32.62500000273119838, -35.31076352940723240 ) ) ;
#2498 = PRODUCT_DEFINITION_SHAPE ( 'NONE', 'NONE',  #23384 ) ;
#2499 = CARTESIAN_POINT ( 'NONE',  ( 20.75514604977248467, 76.42500000273118133, -28.56700777964554305 ) ) ;
#2500 = CARTESIAN_POINT ( 'NONE',  ( -33.58253175000000113, 35.47500000273118559, 10.91162601494193929 ) ) ;
#2501 = CARTESIAN_POINT ( 'NONE',  ( 20.75514604977248467, 22.67500000273119198, -28.56700777964554305 ) ) ;
#2502 = CARTESIAN_POINT ( 'NONE',  ( -9.270509831248423538, 79.70000000000000284, -12.75976212528059861 ) ) ;
#2503 = CARTESIAN_POINT ( 'NONE',  ( 7.025853678916403666, 44.94829833425730925, -26.06988505166735237 ) ) ;
#2504 = CARTESIAN_POINT ( 'NONE',  ( 27.16883889988624290, 75.92500000273119554, 19.73931689729373673 ) ) ;
#2505 = PRESENTATION_LAYER_ASSIGNMENT (  '', '', ( #29870 ) ) ;
#2506 = CARTESIAN_POINT ( 'NONE',  ( -5.147494310547213736, 26.05125428700921475, -32.50000000000007105 ) ) ;
#2507 = CARTESIAN_POINT ( 'NONE',  ( -26.29305231718579350, 59.80000000000000426, -19.10302069950537884 ) ) ;
#2508 = DIRECTION ( 'NONE',  ( 0.000000000000000000, 0.000000000000000000, -1.000000000000000000 ) ) ;
#2509 = CARTESIAN_POINT ( 'NONE',  ( 20.75514604977248467, 62.42500000273118133, -28.56700777964554305 ) ) ;
#2510 = CARTESIAN_POINT ( 'NONE',  ( -18.94512977948575738, 5.924999997268809437, -13.76444248337723231 ) ) ;
#2511 = CARTESIAN_POINT ( 'NONE',  ( -33.58253175000000113, 73.47500000273117848, 10.91162601494193929 ) ) ;
#2512 = CARTESIAN_POINT ( 'NONE',  ( 33.58253175000000113, 8.225000002731182036, -10.91162601494193574 ) ) ;
#2513 = VECTOR ( 'NONE', #32270, 1000.000000000000000 ) ;
#2514 = CARTESIAN_POINT ( 'NONE',  ( 1.507698388325705758E-15, 3.124999997268809615, -24.62258325217400312 ) ) ;
#2515 = CIRCLE ( 'NONE', #852, 12.00000000000000000 ) ;
#2516 = CARTESIAN_POINT ( 'NONE',  ( 26.06988505166735592, 14.87017333425730747, 7.025853678916393896 ) ) ;
#2517 = ORIENTED_EDGE ( 'NONE', *, *, #3604, .F. ) ;
#2518 = CARTESIAN_POINT ( 'NONE',  ( -10.37757302488624411, 44.72500000273120691, -31.93888565452638417 ) ) ;
#2519 = ORIENTED_EDGE ( 'NONE', *, *, #7482, .F. ) ;
#2520 = CARTESIAN_POINT ( 'NONE',  ( -20.50609665441004736, 42.93750000000000000, -20.50609665440969565 ) ) ;
#2521 = CARTESIAN_POINT ( 'NONE',  ( 3.880418787951102289, 10.44874571845314470, -24.50000000000000711 ) ) ;
#2522 = CARTESIAN_POINT ( 'NONE',  ( -32.50000000000000000, 6.400000005462388231, -10.55989012756945478 ) ) ;
#2523 = CARTESIAN_POINT ( 'NONE',  ( -1.778240108872766143E-15, 71.50000000000001421, -32.49999999999999289 ) ) ;
#2524 = CARTESIAN_POINT ( 'NONE',  ( -23.41746824999999887, 2.124999997268811391, -2.867812753649727150E-15 ) ) ;
#2525 = CARTESIAN_POINT ( 'NONE',  ( -7.570916362186210335, 0.5999999999999894307, -23.30088464923126779 ) ) ;
#2526 = CARTESIAN_POINT ( 'NONE',  ( 33.58253175000000823, 18.27500000273118275, 10.91162601494192863 ) ) ;
#2527 = EDGE_CURVE ( 'NONE', #22201, #20335, #24215, .T. ) ;
#2528 = CARTESIAN_POINT ( 'NONE',  ( -10.04305231718579172, 67.59999999999999432, -30.90933677959248982 ) ) ;
#2529 = CARTESIAN_POINT ( 'NONE',  ( -19.82091636218621034, 4.799999999999998934, -14.40073868116559552 ) ) ;
#2530 = CARTESIAN_POINT ( 'NONE',  ( -32.50000000000000000, 30.00000000000000000, 0.000000000000000000 ) ) ;
#2531 = CARTESIAN_POINT ( 'NONE',  ( 15.01150461594643204, 13.86197916666666430, 26.00068869287340334 ) ) ;
#2532 = CARTESIAN_POINT ( 'NONE',  ( -8.601468415847515203, 73.67500000273120975, 11.83890561707634959 ) ) ;
#2533 = CARTESIAN_POINT ( 'NONE',  ( -20.50609665441004736, 39.49999999999999289, -20.50609665440969565 ) ) ;
#2534 = APPLICATION_PROTOCOL_DEFINITION ( 'draft international standard', 'automotive_design', 1998, #25441 ) ;
#2535 = EDGE_CURVE ( 'NONE', #2384, #4493, #31224, .T. ) ;
#2536 = CARTESIAN_POINT ( 'NONE',  ( -40.00000000000000711, 52.00000000000000711, -23.09401076758504345 ) ) ;
#2537 = CARTESIAN_POINT ( 'NONE',  ( -14.47279130897151589, 17.82499999726881157, -19.92008829642072598 ) ) ;
#2538 = CARTESIAN_POINT ( 'NONE',  ( -26.29305231718579350, 7.800000000000001599, -19.10302069950537884 ) ) ;
#2539 = CARTESIAN_POINT ( 'NONE',  ( -1.778240108872766143E-15, 18.00000000546237544, -32.49999999999999289 ) ) ;
#2540 = CARTESIAN_POINT ( 'NONE',  ( -26.06988505166722803, 54.67670166574269075, 7.025853678916877953 ) ) ;
#2541 = CARTESIAN_POINT ( 'NONE',  ( -27.16883889988624290, 48.92500000273120264, -19.73931689729374028 ) ) ;
#2542 = AXIS2_PLACEMENT_3D ( 'NONE', #19089, #31, #24235 ) ;
#2543 = CARTESIAN_POINT ( 'NONE',  ( -33.58253175000000113, 53.47500000273117848, 10.91162601494193929 ) ) ;
#2544 = CARTESIAN_POINT ( 'NONE',  ( -10.37757302488623701, 41.77500000273118275, 31.93888565452638417 ) ) ;
#2545 = DIRECTION ( 'NONE',  ( -0.000000000000000000, -1.000000000000000000, -0.000000000000000000 ) ) ;
#2546 = CARTESIAN_POINT ( 'NONE',  ( 19.09188309203661049, 12.85937500000000000, -19.09188309203694445 ) ) ;
#2547 = CARTESIAN_POINT ( 'NONE',  ( -20.08610463437157989, 61.69999999999999574, -27.64615127144129758 ) ) ;
#2548 = DIRECTION ( 'NONE',  ( 1.000000000000000000, 0.000000000000000000, 0.000000000000000000 ) ) ;
#2549 = CARTESIAN_POINT ( 'NONE',  ( -10.04305231718578462, 78.40000000000000568, 30.90933677959249337 ) ) ;
#2550 = CARTESIAN_POINT ( 'NONE',  ( 27.16883889988623935, 12.32500000273119234, -19.73931689729374384 ) ) ;
#2551 = CARTESIAN_POINT ( 'NONE',  ( 2.694222958124179176E-15, -45.00000000000001421, 0.000000000000000000 ) ) ;
#2552 = CARTESIAN_POINT ( 'NONE',  ( 0.000000000000000000, 102.0000000000000284, 0.000000000000000000 ) ) ;
#2553 = CARTESIAN_POINT ( 'NONE',  ( 24.50000000000000000, 12.09999999999999609, -7.960532557706203605 ) ) ;
#2554 = CARTESIAN_POINT ( 'NONE',  ( -0.04044903255042732459, 21.30430583240935860, -27.95245687107223986 ) ) ;
#2555 = CARTESIAN_POINT ( 'NONE',  ( -32.50000000000000000, 38.40000000546235981, -10.55989012756945478 ) ) ;
#2556 = CARTESIAN_POINT ( 'NONE',  ( -24.50000000000000000, 10.74999999453762811, -3.000384657911015469E-15 ) ) ;
#2557 = CARTESIAN_POINT ( 'NONE',  ( -10.37757302488623701, 25.52500000273119696, 31.93888565452638417 ) ) ;
#2558 = CARTESIAN_POINT ( 'NONE',  ( -19.09188309203694445, 46.37500000000000000, -19.09188309203661049 ) ) ;
#2559 = ORIENTED_EDGE ( 'NONE', *, *, #9203, .F. ) ;
#2560 = CARTESIAN_POINT ( 'NONE',  ( 33.58253175000000113, 62.12500000273117706, -4.112674001490185761E-15 ) ) ;
#2561 = CARTESIAN_POINT ( 'NONE',  ( -15.01150461594642138, 46.51822916666666430, -26.00068869287340334 ) ) ;
#2562 = EDGE_LOOP ( 'NONE', ( #9167, #24597 ) ) ;
#2563 = CARTESIAN_POINT ( 'NONE',  ( 15.01150461594596308, 12.71614583333333037, -26.00068869287367335 ) ) ;
#2564 = CARTESIAN_POINT ( 'NONE',  ( 0.04044903254992426173, 10.43006916759064495, -30.02300923189239867 ) ) ;
#2565 = VERTEX_POINT ( 'NONE', #33097 ) ;
#2566 = CARTESIAN_POINT ( 'NONE',  ( -27.16883889988624290, 6.925000002731204418, -19.73931689729374028 ) ) ;
#2567 = CARTESIAN_POINT ( 'NONE',  ( 1.076200423132605543E-16, 52.00000000000000711, -46.18802153517007980 ) ) ;
#2568 = CIRCLE ( 'NONE', #27225, 30.50000000000000000 ) ;
#2569 = CARTESIAN_POINT ( 'NONE',  ( -20.75514604977248112, 35.67500000273118843, 28.56700777964554661 ) ) ;
#2570 = CARTESIAN_POINT ( 'NONE',  ( -2.092463501923844636E-15, 40.00000000546237544, -34.17252228774368916 ) ) ;
#2571 = EDGE_CURVE ( 'NONE', #18361, #11875, #25218, .T. ) ;
#2572 =( BOUNDED_CURVE ( )  B_SPLINE_CURVE ( 2, ( #31231, #4981, #15460, #7723, #18211, #14768, #25233, #1708, #12186, #15970, #28992, #28824, #18717 ),
 .UNSPECIFIED., .F., .T. ) 
 B_SPLINE_CURVE_WITH_KNOTS ( ( 3, 2, 2, 2, 2, 2, 3 ),
 ( 0.5320512820512820484, 0.5333333333333333259, 0.5358974358974358809, 0.5384615384615384359, 0.5410256410256409909, 0.5435897435897435459, 0.5448717948717948234 ),
 .UNSPECIFIED. ) 
 CURVE ( )  GEOMETRIC_REPRESENTATION_ITEM ( )  RATIONAL_B_SPLINE_CURVE ( ( 0.9755282581475768211, 0.9755282581475768211, 1.000000000000000000, 0.9510565162951535312, 1.000000000000000000, 0.9510565162951535312, 1.000000000000000000, 0.9510565162951535312, 1.000000000000000000, 0.9510565162951535312, 1.000000000000000000, 0.9755282581475768211, 0.9755282581475768211 ) ) 
 REPRESENTATION_ITEM ( '' )  );
#2573 = CARTESIAN_POINT ( 'NONE',  ( 15.00000000000000355, 74.90000000000003411, 4.873795443493592394 ) ) ;
#2574 = CARTESIAN_POINT ( 'NONE',  ( -28.01184896238290278, 66.42708333333332860, 7.505752307973363457 ) ) ;
#2575 = CARTESIAN_POINT ( 'NONE',  ( 33.58253175000000113, 20.12500000273118062, -4.112674001490185761E-15 ) ) ;
#2576 = CARTESIAN_POINT ( 'NONE',  ( 26.29305231718579350, 76.80000000000001137, 19.10302069950537529 ) ) ;
#2577 = CARTESIAN_POINT ( 'NONE',  ( 20.75514604977249178, 52.07500000273119412, 28.56700777964553950 ) ) ;
#2578 = AXIS2_PLACEMENT_3D ( 'NONE', #30953, #25809, #17935 ) ;
#2579 = CARTESIAN_POINT ( 'NONE',  ( -10.04305231718578462, 32.39999999999999858, 30.90933677959249337 ) ) ;
#2580 = CARTESIAN_POINT ( 'NONE',  ( -20.08610463437156923, 26.29999999999998295, 27.64615127144130113 ) ) ;
#2581 = CARTESIAN_POINT ( 'NONE',  ( -24.50000000000000355, 2.899999999999995470, -7.960532557706207157 ) ) ;
#2582 = CARTESIAN_POINT ( 'NONE',  ( 10.37757302488624056, 68.52500000273120406, -31.93888565452638417 ) ) ;
#2583 = CARTESIAN_POINT ( 'NONE',  ( -32.50000000000000000, 77.90000000000000568, -10.55989012756945300 ) ) ;
#2584 = CARTESIAN_POINT ( 'NONE',  ( 12.65897589331677153, 74.00000000000004263, -5.871086419100934428 ) ) ;
#2585 = CARTESIAN_POINT ( 'NONE',  ( -20.75514604977248823, 61.07500000273119412, -28.56700777964554305 ) ) ;
#2586 = DIRECTION ( 'NONE',  ( 0.000000000000000000, -1.000000000000000000, 0.000000000000000000 ) ) ;
#2587 = CARTESIAN_POINT ( 'NONE',  ( 10.37757302488624767, 11.72500000273118914, 31.93888565452638417 ) ) ;
#2588 = CARTESIAN_POINT ( 'NONE',  ( -24.22776226481240514, 33.34673583425730214, 13.94119854578937812 ) ) ;
#2589 = DIRECTION ( 'NONE',  ( -0.000000000000000000, 1.000000000000000000, -0.000000000000000000 ) ) ;
#2590 = LINE ( 'NONE', #28030, #25348 ) ;
#2591 = CARTESIAN_POINT ( 'NONE',  ( 33.58253175000000113, 32.22500000273117848, -10.91162601494193751 ) ) ;
#2592 = DIRECTION ( 'NONE',  ( -0.000000000000000000, -1.000000000000000000, -0.000000000000000000 ) ) ;
#2593 = CARTESIAN_POINT ( 'NONE',  ( 11.45223628611453215, -57.99999999999999289, 1.402494451086933009E-15 ) ) ;
#2594 = CARTESIAN_POINT ( 'NONE',  ( 4.300734207923761154, 79.47500000273116427, 13.23629886949340495 ) ) ;
#2595 = CARTESIAN_POINT ( 'NONE',  ( 0.04044903255045854962, 47.08555583240935505, 30.02300923189239867 ) ) ;
#2596 = CARTESIAN_POINT ( 'NONE',  ( -20.08610463437157989, 56.20000000546239249, -27.64615127144129758 ) ) ;
#2597 = CARTESIAN_POINT ( 'NONE',  ( -13.91746824999999532, 77.27500000273117564, -4.522059556121115875 ) ) ;
#2598 =( NAMED_UNIT ( * ) SI_UNIT ( $, .STERADIAN. ) SOLID_ANGLE_UNIT ( ) );
#2599 = CARTESIAN_POINT ( 'NONE',  ( 19.09188309203694800, 20.59374999999999645, 19.09188309203660694 ) ) ;
#2600 = CARTESIAN_POINT ( 'NONE',  ( -5.147494310547423346, 54.44874571845315359, 32.50000000000000000 ) ) ;
#2601 = AXIS2_PLACEMENT_3D ( 'NONE', #3611, #27453, #1355 ) ;
#2602 = CARTESIAN_POINT ( 'NONE',  ( -26.29305231718579350, 70.30000000546237970, -19.10302069950537884 ) ) ;
#2603 = CARTESIAN_POINT ( 'NONE',  ( 15.01150461594643204, 17.29947916666666430, 26.00068869287340334 ) ) ;
#2604 = CARTESIAN_POINT ( 'NONE',  ( 27.16883889988624290, 32.17500000273120264, 19.73931689729373673 ) ) ;
#2605 = CARTESIAN_POINT ( 'NONE',  ( -14.47279130897152299, 12.42499999726880588, 19.92008829642072243 ) ) ;
#2606 = ORIENTED_EDGE ( 'NONE', *, *, #25136, .F. ) ;
#2607 = CARTESIAN_POINT ( 'NONE',  ( 20.47846945139902530, 42.65663166759063785, 20.53372385742071771 ) ) ;
#2608 = CARTESIAN_POINT ( 'NONE',  ( 10.04305231718579705, 21.10000000546237331, 30.90933677959248982 ) ) ;
#2609 = CARTESIAN_POINT ( 'NONE',  ( -15.01150461594642138, 46.51822916666666430, -26.00068869287340334 ) ) ;
#2610 = CARTESIAN_POINT ( 'NONE',  ( 26.00068869287367335, 65.13802083333334281, 15.01150461594596308 ) ) ;
#2611 = CARTESIAN_POINT ( 'NONE',  ( 33.58253175000000113, 54.37500000273118417, -4.112674001490185761E-15 ) ) ;
#2612 = CARTESIAN_POINT ( 'NONE',  ( -26.29305231718578995, 54.70000000546237828, 19.10302069950538595 ) ) ;
#2613 = CARTESIAN_POINT ( 'NONE',  ( 7.570916362186207671, 5.349999994537641079, 23.30088464923126779 ) ) ;
#2614 = CARTESIAN_POINT ( 'NONE',  ( 10.37757302488624767, 43.72500000273119269, 31.93888565452638417 ) ) ;
#2615 = CARTESIAN_POINT ( 'NONE',  ( -12.13525491562420910, 72.19999999999998863, 8.816778784387098611 ) ) ;
#2616 = CARTESIAN_POINT ( 'NONE',  ( -33.58253175000000113, 71.37500000273119838, 0.000000000000000000 ) ) ;
#2617 = CARTESIAN_POINT ( 'NONE',  ( 32.50000000000000711, 1.400000005462371799, 10.55989012756945122 ) ) ;
#2618 = CARTESIAN_POINT ( 'NONE',  ( -2.162160676586882350E-15, 62.62500000273117706, -35.31076352940722529 ) ) ;
#2619 = CARTESIAN_POINT ( 'NONE',  ( -28.01184896238290278, 21.73958333333332860, 7.505752307973363457 ) ) ;
#2620 = CARTESIAN_POINT ( 'NONE',  ( -32.50000000000000000, 45.99999999999998579, 0.000000000000000000 ) ) ;
#2621 = CARTESIAN_POINT ( 'NONE',  ( -18.94512977948576093, 5.824999997268820451, 13.76444248337722698 ) ) ;
#2622 = CARTESIAN_POINT ( 'NONE',  ( -2.162160676586881955E-15, 8.875000002731189497, -35.31076352940723240 ) ) ;
#2623 = CARTESIAN_POINT ( 'NONE',  ( -5.147494577961174933, 66.94874572125284828, 32.49999991311200631 ) ) ;
#2624 = CARTESIAN_POINT ( 'NONE',  ( -24.22776226481266448, 37.91888916574269075, -13.94119854578892514 ) ) ;
#2625 = CARTESIAN_POINT ( 'NONE',  ( 8.601468415847516980, 78.67500000273119554, -11.83890561707634781 ) ) ;
#2626 = CARTESIAN_POINT ( 'NONE',  ( -11.54700538379251817, 96.00000000000002842, 19.99999999999999645 ) ) ;
#2627 = DIRECTION ( 'NONE',  ( 0.000000000000000000, 1.000000000000000000, 0.000000000000000000 ) ) ;
#2628 = VECTOR ( 'NONE', #19450, 1000.000000000000114 ) ;
#2629 = CARTESIAN_POINT ( 'NONE',  ( -27.16883889988624290, 77.17500000273118133, -19.73931689729374028 ) ) ;
#2630 = ORIENTED_EDGE ( 'NONE', *, *, #12936, .T. ) ;
#2631 = DIRECTION ( 'NONE',  ( 0.000000000000000000, -1.000000000000000000, 0.000000000000000000 ) ) ;
#2632 = CARTESIAN_POINT ( 'NONE',  ( 19.09188309203661049, 57.54687500000000000, -19.09188309203694445 ) ) ;
#2633 = CARTESIAN_POINT ( 'NONE',  ( -20.75514604977248823, 56.82500000273117990, -28.56700777964554305 ) ) ;
#2634 = CARTESIAN_POINT ( 'NONE',  ( 27.16883889988623935, 14.57500000273119412, -19.73931689729374384 ) ) ;
#2635 = CARTESIAN_POINT ( 'NONE',  ( 10.37757302488624056, 2.775000002731189852, -31.93888565452638417 ) ) ;
#2636 = CARTESIAN_POINT ( 'NONE',  ( 2.584737979205442066E-13, 38.21093750000000000, 27.95245687107223276 ) ) ;
#2637 = CARTESIAN_POINT ( 'NONE',  ( -20.53372385742071771, 29.76600666759063429, 20.47846945139902530 ) ) ;
#2638 = CARTESIAN_POINT ( 'NONE',  ( 0.04044903255045854962, 19.58555583240935860, 30.02300923189239867 ) ) ;
#2639 = CARTESIAN_POINT ( 'NONE',  ( 20.08610463437157279, 73.80000000546239391, -27.64615127144129758 ) ) ;
#2640 = CARTESIAN_POINT ( 'NONE',  ( 32.46390416700889148, 52.00000000000002842, 8.309214287527991516 ) ) ;
#2641 = CARTESIAN_POINT ( 'NONE',  ( 33.58253175000000113, 38.12500000273119838, -4.112674001490185761E-15 ) ) ;
#2642 = CARTESIAN_POINT ( 'NONE',  ( 6.950374756619257965, 45.51003499907601935, -26.09010956794244507 ) ) ;
#2643 = CARTESIAN_POINT ( 'NONE',  ( -14.47279130897152122, 9.924999997268825425, 19.92008829642072243 ) ) ;
#2644 = CARTESIAN_POINT ( 'NONE',  ( -26.29305231718578995, 2.700000005462388497, 19.10302069950538595 ) ) ;
#2645 = EDGE_LOOP ( 'NONE', ( #22385, #6844, #9366, #19276 ) ) ;
#2646 = CARTESIAN_POINT ( 'NONE',  ( 6.486482029760649416E-15, 53.87500000273118417, 35.31076352940723240 ) ) ;
#2647 = CARTESIAN_POINT ( 'NONE',  ( -4.635254915624208216, 70.65000000546240244, 14.26584774442730463 ) ) ;
#2648 = CARTESIAN_POINT ( 'NONE',  ( 26.09010956794232428, 42.08371500092398065, -6.950374756619718042 ) ) ;
#2649 = CARTESIAN_POINT ( 'NONE',  ( -27.16883889988624290, 77.17500000273119554, -19.73931689729374028 ) ) ;
#2650 = EDGE_LOOP ( 'NONE', ( #21661, #22225, #26066, #12471 ) ) ;
#2651 = APPLICATION_CONTEXT ( 'automotive_design' ) ;
#2652 = CARTESIAN_POINT ( 'NONE',  ( -10.37757302488623701, 23.52500000273117919, 31.93888565452638417 ) ) ;
#2653 = CARTESIAN_POINT ( 'NONE',  ( 30.02300923189239512, 13.28906249999999289, -2.619432448724977703E-13 ) ) ;
#2654 = VECTOR ( 'NONE', #16217, 1000.000000000000000 ) ;
#2655 = EDGE_LOOP ( 'NONE', ( #11680, #2341, #6891 ) ) ;
#2656 = CARTESIAN_POINT ( 'NONE',  ( -10.37757302488624411, 62.72500000273117848, -31.93888565452638417 ) ) ;
#2657 = CARTESIAN_POINT ( 'NONE',  ( -20.50609665440969209, 52.39062499999999289, 20.50609665441005092 ) ) ;
#2658 = CARTESIAN_POINT ( 'NONE',  ( -19.82091636218621034, 6.549999994537619941, -14.40073868116559552 ) ) ;
#2659 = CARTESIAN_POINT ( 'NONE',  ( -18.94512977948576093, 4.324999997268818674, 13.76444248337722698 ) ) ;
#2660 = ADVANCED_FACE ( 'NONE', ( #12691, #12522 ), #4281, .F. ) ;
#2661 = CARTESIAN_POINT ( 'NONE',  ( -10.37757302488624411, 2.725000002731181592, -31.93888565452638417 ) ) ;
#2662 = CARTESIAN_POINT ( 'NONE',  ( -15.00000000000000000, 78.25000000546239676, 0.000000000000000000 ) ) ;
#2663 = CARTESIAN_POINT ( 'NONE',  ( -28.00173670424535644, 61.55170166574269786, 7.543491769121936308 ) ) ;
#2664 = CARTESIAN_POINT ( 'NONE',  ( 5.779280353836490358E-15, 57.00000000546238965, 32.49999999999999289 ) ) ;
#2665 = CARTESIAN_POINT ( 'NONE',  ( 9.270509831248421762, 81.29999999999999716, -12.75976212528059861 ) ) ;
#2666 = CARTESIAN_POINT ( 'NONE',  ( -1.778240108872766143E-15, 9.499999999999992895, -32.49999999999999289 ) ) ;
#2667 = ADVANCED_FACE ( 'NONE', ( #20423, #2047 ), #4449, .F. ) ;
#2668 = CARTESIAN_POINT ( 'NONE',  ( -26.29305231718579350, 13.79999999999999361, -19.10302069950537884 ) ) ;
#2669 = CARTESIAN_POINT ( 'NONE',  ( 26.07999730980477437, 64.70833333333334281, -6.988114217768290004 ) ) ;
#2670 = CARTESIAN_POINT ( 'NONE',  ( -7.570916362186210335, 10.34999999453761710, -23.30088464923126779 ) ) ;
#2671 = CARTESIAN_POINT ( 'NONE',  ( -9.270509831248425314, 71.95000000546238539, -12.75976212528059861 ) ) ;
#2672 = CARTESIAN_POINT ( 'NONE',  ( -2.428612866367529427E-13, 29.61718749999999645, -27.95245687107222921 ) ) ;
#2673 =( BOUNDED_SURFACE ( )  B_SPLINE_SURFACE ( 1, 2, ( 
 ( #20020, #12111, #9194, #25331, #15043, #33034, #9887, #1987, #19679, #24988, #20364, #27566, #12462, #1634, #22932, #9712, #33388, #1471, #7134, #1295, #25157, #4393, #30812, #22583, #7305, #30125, #1809, #11777, #6795, #6628, #22257, #9538, #17789, #17107, #4053, #11946, #22415, #6965, #32863, #9360, #12285, #22759, #19841, #33210, #12977, #15388, #2334, #18311, #2510, #18478, #23279, #2685, #10574, #33565, #4907, #31664, #10403, #28922, #28583, #8159, #33914, #20882, #7994, #13144, #21221, #31331, #26190, #257, #7823, #28757, #5253, #18649, #29087, #5422, #31501, #15735, #10063, #15902, #18139, #12807, #10239, #23617, #28418, #21052, #15213, #13318, #86, #17968, #23452, #26357, #31161, #2847, #25676, #10742, #25844, #23791, #5080, #2157, #26018, #12631, #23101, #20543, #30988, #7488, #33744, #20720, #15566, #7653, #591, #29425, #22049, #5927, #16404, #18813, #29256, #6256, #3683, #29582, #5759, #8824, #16735, #13824, #19309, #26528, #29751, #27192, #18980, #13988, #3021, #24293, #3354, #24450, #13492, #11245, #926, #19475, #8493, #8660, #428, #5591, #24125, #16073, #21722, #764, #32496, #26859, #14156, #10913, #32167, #6085, #26694, #23957, #11405, #16239, #19144, #24613, #16567, #27022, #3517, #21882, #32332, #1087, #11569, #8995, #11082, #21385, #31830, #8323, #3190, #13661, #31997, #21551, #33171, #4525, #27526, #1255, #9675, #17067, #4015, #27871, #14489 ),
 ( #25295, #9499, #1765, #17409, #30426, #24947, #6925, #4353, #12072, #14829, #22723, #12246, #14322, #25119, #17236, #3847, #19980, #20155, #4187, #15001, #30600, #24777, #30084, #25470, #32663, #7095, #6757, #17579, #28039, #1947, #19641, #12423, #33350, #9318, #32991, #22893, #22379, #9848, #11736, #29925, #6427, #1429, #22216, #16900, #19805, #27362, #9158, #6590, #11907, #32827, #30253, #27696, #14659, #1594, #22542, #31288, #13106, #4870, #25977, #23064, #28884, #17931, #4696, #10027, #2469, #12935, #15350, #7446, #31122, #5382, #20682, #25641, #12593, #18268, #23411, #33701, #10202, #10365, #18440, #33524, #7265, #30775, #18095, #23579, #10533, #20843, #15861, #45, #33872, #2120, #15524, #28381, #7782, #2643, #17751, #28716, #7615, #25804, #28542, #21010, #5212, #31460, #20325, #20501, #26147, #15695, #7953, #2296, #12768, #26317, #2806, #13273, #30949, #23748, #23242, #214, #28210, #15176, #5039, #24086, #16200, #18941, #11367, #11205, #885, #10700, #10873, #16523, #32124, #24248, #26654, #5722, #21843, #13621, #3149, #21348, #13946, #19265, #8280, #16031, #24409, #31789, #18772, #8620, #29216, #554, #11040, #32288, #29386, #21508, #8781, #6042, #719, #26975, #19102, #21676, #31957, #29540, #3475, #26818, #29707, #6210, #16691, #29047, #5886, #8450, #18608, #27148, #3641, #16363, #14115, #24573, #5550, #3314, #21181, #13449, #31623, #13780, #8121, #26486, #2981 ) ),
 .UNSPECIFIED., .F., .F., .T. ) 
 B_SPLINE_SURFACE_WITH_KNOTS ( ( 2, 2 ),
 ( 3, 2, 2, 2, 2, 2, 2, 2, 2, 2, 2, 2, 2, 2, 2, 2, 2, 2, 2, 2, 2, 2, 2, 2, 2, 2, 2, 2, 2, 2, 2, 2, 2, 2, 2, 2, 2, 2, 2, 2, 2, 2, 2, 2, 2, 2, 2, 2, 2, 2, 2, 2, 2, 2, 2, 2, 2, 2, 2, 2, 2, 2, 2, 2, 2, 2, 2, 2, 2, 2, 2, 2, 2, 2, 2, 2, 2, 2, 2, 2, 2, 2, 2, 2, 2, 2, 2, 2, 2, 2, 3 ),
 ( 0.000000000000000000, 1.000000000000000000 ),
 ( 0.000000000000000000, 0.01111111111111111154, 0.02222222222222222307, 0.03333333333333333287, 0.04444444444444444614, 0.05555555555555555247, 0.06666666666666666574, 0.07777777777777777901, 0.08888888888888889228, 0.1000000000000000056, 0.1111111111111111049, 0.1222222222222222182, 0.1333333333333333315, 0.1444444444444444309, 0.1555555555555555580, 0.1666666666666666574, 0.1777777777777777846, 0.1888888888888888840, 0.2000000000000000111, 0.2111111111111111105, 0.2222222222222222099, 0.2333333333333333370, 0.2444444444444444364, 0.2555555555555555358, 0.2666666666666666630, 0.2777777777777777901, 0.2888888888888888618, 0.2999999999999999889, 0.3111111111111111160, 0.3222222222222222432, 0.3333333333333333148, 0.3444444444444444420, 0.3555555555555555691, 0.3666666666666666408, 0.3777777777777777679, 0.3888888888888888951, 0.4000000000000000222, 0.4111111111111110938, 0.4222222222222222210, 0.4333333333333333481, 0.4444444444444444198, 0.4555555555555555469, 0.4666666666666666741, 0.4777777777777778012, 0.4888888888888888729, 0.5000000000000000000, 0.5111111111111110716, 0.5222222222222222543, 0.5333333333333333259, 0.5444444444444443976, 0.5555555555555555802, 0.5666666666666666519, 0.5777777777777777235, 0.5888888888888889062, 0.5999999999999999778, 0.6111111111111111605, 0.6222222222222222321, 0.6333333333333333037, 0.6444444444444444864, 0.6555555555555555580, 0.6666666666666666297, 0.6777777777777778123, 0.6888888888888888840, 0.6999999999999999556, 0.7111111111111111382, 0.7222222222222222099, 0.7333333333333332815, 0.7444444444444444642, 0.7555555555555555358, 0.7666666666666667185, 0.7777777777777777901, 0.7888888888888888618, 0.8000000000000000444, 0.8111111111111111160, 0.8222222222222221877, 0.8333333333333333703, 0.8444444444444444420, 0.8555555555555555136, 0.8666666666666666963, 0.8777777777777777679, 0.8888888888888888395, 0.9000000000000000222, 0.9111111111111110938, 0.9222222222222222765, 0.9333333333333333481, 0.9444444444444444198, 0.9555555555555556024, 0.9666666666666666741, 0.9777777777777777457, 0.9888888888888889284, 1.000000000000000000 ),
 .UNSPECIFIED. ) 
 GEOMETRIC_REPRESENTATION_ITEM ( )  RATIONAL_B_SPLINE_SURFACE ( (
 ( 1.000000000000000000, 0.9510565162951535312, 1.000000000000000000, 0.9510565162951535312, 1.000000000000000000, 0.9510565162951535312, 1.000000000000000000, 0.9510565162951535312, 1.000000000000000000, 0.9510565162951535312, 1.000000000000000000, 0.9510565162951535312, 1.000000000000000000, 0.9510565162951535312, 1.000000000000000000, 0.9510565162951535312, 1.000000000000000000, 0.9510565162951535312, 1.000000000000000000, 0.9510565162951535312, 1.000000000000000000, 0.9510565162951535312, 1.000000000000000000, 0.9510565162951535312, 1.000000000000000000, 0.9510565162951535312, 1.000000000000000000, 0.9510565162951535312, 1.000000000000000000, 0.9510565162951535312, 1.000000000000000000, 0.9510565162951535312, 1.000000000000000000, 0.9510565162951535312, 1.000000000000000000, 0.9510565162951535312, 1.000000000000000000, 0.9510565162951535312, 1.000000000000000000, 0.9510565162951535312, 1.000000000000000000, 0.9510565162951535312, 1.000000000000000000, 0.9510565162951535312, 1.000000000000000000, 0.9510565162951535312, 1.000000000000000000, 0.9510565162951535312, 1.000000000000000000, 0.9510565162951535312, 1.000000000000000000, 0.9510565162951535312, 1.000000000000000000, 0.9510565162951535312, 1.000000000000000000, 0.9510565162951535312, 1.000000000000000000, 0.9510565162951535312, 1.000000000000000000, 0.9510565162951535312, 1.000000000000000000, 0.9510565162951535312, 1.000000000000000000, 0.9510565162951535312, 1.000000000000000000, 0.9510565162951535312, 1.000000000000000000, 0.9510565162951535312, 1.000000000000000000, 0.9510565162951535312, 1.000000000000000000, 0.9510565162951535312, 1.000000000000000000, 0.9510565162951535312, 1.000000000000000000, 0.9510565162951535312, 1.000000000000000000, 0.9510565162951535312, 1.000000000000000000, 0.9510565162951535312, 1.000000000000000000, 0.9510565162951535312, 1.000000000000000000, 0.9510565162951535312, 1.000000000000000000, 0.9510565162951535312, 1.000000000000000000, 0.9510565162951535312, 1.000000000000000000, 0.9510565162951535312, 1.000000000000000000, 0.9510565162951535312, 1.000000000000000000, 0.9510565162951535312, 1.000000000000000000, 0.9510565162951535312, 1.000000000000000000, 0.9510565162951535312, 1.000000000000000000, 0.9510565162951535312, 1.000000000000000000, 0.9510565162951535312, 1.000000000000000000, 0.9510565162951535312, 1.000000000000000000, 0.9510565162951535312, 1.000000000000000000, 0.9510565162951535312, 1.000000000000000000, 0.9510565162951535312, 1.000000000000000000, 0.9510565162951535312, 1.000000000000000000, 0.9510565162951535312, 1.000000000000000000, 0.9510565162951535312, 1.000000000000000000, 0.9510565162951535312, 1.000000000000000000, 0.9510565162951535312, 1.000000000000000000, 0.9510565162951535312, 1.000000000000000000, 0.9510565162951535312, 1.000000000000000000, 0.9510565162951535312, 1.000000000000000000, 0.9510565162951535312, 1.000000000000000000, 0.9510565162951535312, 1.000000000000000000, 0.9510565162951535312, 1.000000000000000000, 0.9510565162951535312, 1.000000000000000000, 0.9510565162951535312, 1.000000000000000000, 0.9510565162951535312, 1.000000000000000000, 0.9510565162951535312, 1.000000000000000000, 0.9510565162951535312, 1.000000000000000000, 0.9510565162951535312, 1.000000000000000000, 0.9510565162951535312, 1.000000000000000000, 0.9510565162951535312, 1.000000000000000000, 0.9510565162951535312, 1.000000000000000000, 0.9510565162951535312, 1.000000000000000000, 0.9510565162951535312, 1.000000000000000000, 0.9510565162951535312, 1.000000000000000000, 0.9510565162951535312, 1.000000000000000000, 0.9510565162951535312, 1.000000000000000000, 0.9510565162951535312, 1.000000000000000000, 0.9510565162951535312, 1.000000000000000000, 0.9510565162951535312, 1.000000000000000000, 0.9510565162951535312, 1.000000000000000000, 0.9510565162951535312, 1.000000000000000000, 0.9510565162951535312, 1.000000000000000000, 0.9510565162951535312, 1.000000000000000000, 0.9510565162951535312, 1.000000000000000000, 0.9510565162951535312, 1.000000000000000000, 0.9510565162951535312, 1.000000000000000000),
 ( 1.000000000000000000, 0.9510565162951535312, 1.000000000000000000, 0.9510565162951535312, 1.000000000000000000, 0.9510565162951535312, 1.000000000000000000, 0.9510565162951535312, 1.000000000000000000, 0.9510565162951535312, 1.000000000000000000, 0.9510565162951535312, 1.000000000000000000, 0.9510565162951535312, 1.000000000000000000, 0.9510565162951535312, 1.000000000000000000, 0.9510565162951535312, 1.000000000000000000, 0.9510565162951535312, 1.000000000000000000, 0.9510565162951535312, 1.000000000000000000, 0.9510565162951535312, 1.000000000000000000, 0.9510565162951535312, 1.000000000000000000, 0.9510565162951535312, 1.000000000000000000, 0.9510565162951535312, 1.000000000000000000, 0.9510565162951535312, 1.000000000000000000, 0.9510565162951535312, 1.000000000000000000, 0.9510565162951535312, 1.000000000000000000, 0.9510565162951535312, 1.000000000000000000, 0.9510565162951535312, 1.000000000000000000, 0.9510565162951535312, 1.000000000000000000, 0.9510565162951535312, 1.000000000000000000, 0.9510565162951535312, 1.000000000000000000, 0.9510565162951535312, 1.000000000000000000, 0.9510565162951535312, 1.000000000000000000, 0.9510565162951535312, 1.000000000000000000, 0.9510565162951535312, 1.000000000000000000, 0.9510565162951535312, 1.000000000000000000, 0.9510565162951535312, 1.000000000000000000, 0.9510565162951535312, 1.000000000000000000, 0.9510565162951535312, 1.000000000000000000, 0.9510565162951535312, 1.000000000000000000, 0.9510565162951535312, 1.000000000000000000, 0.9510565162951535312, 1.000000000000000000, 0.9510565162951535312, 1.000000000000000000, 0.9510565162951535312, 1.000000000000000000, 0.9510565162951535312, 1.000000000000000000, 0.9510565162951535312, 1.000000000000000000, 0.9510565162951535312, 1.000000000000000000, 0.9510565162951535312, 1.000000000000000000, 0.9510565162951535312, 1.000000000000000000, 0.9510565162951535312, 1.000000000000000000, 0.9510565162951535312, 1.000000000000000000, 0.9510565162951535312, 1.000000000000000000, 0.9510565162951535312, 1.000000000000000000, 0.9510565162951535312, 1.000000000000000000, 0.9510565162951535312, 1.000000000000000000, 0.9510565162951535312, 1.000000000000000000, 0.9510565162951535312, 1.000000000000000000, 0.9510565162951535312, 1.000000000000000000, 0.9510565162951535312, 1.000000000000000000, 0.9510565162951535312, 1.000000000000000000, 0.9510565162951535312, 1.000000000000000000, 0.9510565162951535312, 1.000000000000000000, 0.9510565162951535312, 1.000000000000000000, 0.9510565162951535312, 1.000000000000000000, 0.9510565162951535312, 1.000000000000000000, 0.9510565162951535312, 1.000000000000000000, 0.9510565162951535312, 1.000000000000000000, 0.9510565162951535312, 1.000000000000000000, 0.9510565162951535312, 1.000000000000000000, 0.9510565162951535312, 1.000000000000000000, 0.9510565162951535312, 1.000000000000000000, 0.9510565162951535312, 1.000000000000000000, 0.9510565162951535312, 1.000000000000000000, 0.9510565162951535312, 1.000000000000000000, 0.9510565162951535312, 1.000000000000000000, 0.9510565162951535312, 1.000000000000000000, 0.9510565162951535312, 1.000000000000000000, 0.9510565162951535312, 1.000000000000000000, 0.9510565162951535312, 1.000000000000000000, 0.9510565162951535312, 1.000000000000000000, 0.9510565162951535312, 1.000000000000000000, 0.9510565162951535312, 1.000000000000000000, 0.9510565162951535312, 1.000000000000000000, 0.9510565162951535312, 1.000000000000000000, 0.9510565162951535312, 1.000000000000000000, 0.9510565162951535312, 1.000000000000000000, 0.9510565162951535312, 1.000000000000000000, 0.9510565162951535312, 1.000000000000000000, 0.9510565162951535312, 1.000000000000000000, 0.9510565162951535312, 1.000000000000000000, 0.9510565162951535312, 1.000000000000000000, 0.9510565162951535312, 1.000000000000000000, 0.9510565162951535312, 1.000000000000000000, 0.9510565162951535312, 1.000000000000000000, 0.9510565162951535312, 1.000000000000000000, 0.9510565162951535312, 1.000000000000000000, 0.9510565162951535312, 1.000000000000000000, 0.9510565162951535312, 1.000000000000000000) ) ) 
 REPRESENTATION_ITEM ( '' )  SURFACE ( )  );
#2674 = CARTESIAN_POINT ( 'NONE',  ( 33.58253175000000113, 30.12500000273118772, -4.112674001490185761E-15 ) ) ;
#2675 = CARTESIAN_POINT ( 'NONE',  ( -10.37757302488623701, 71.52500000273118985, 31.93888565452638417 ) ) ;
#2676 = CARTESIAN_POINT ( 'NONE',  ( 33.58253175000000113, 34.37500000273117706, -4.112674001490185761E-15 ) ) ;
#2677 = CARTESIAN_POINT ( 'NONE',  ( 33.58253175000000113, 18.37500000273117706, -4.112674001490185761E-15 ) ) ;
#2678 = CARTESIAN_POINT ( 'NONE',  ( -32.50000000000000000, 63.89999999999998437, -10.55989012756945300 ) ) ;
#2679 = CARTESIAN_POINT ( 'NONE',  ( 27.95245687107223986, 55.97694416759064495, 0.04044903254993640479 ) ) ;
#2680 = CARTESIAN_POINT ( 'NONE',  ( -20.75514604977248112, 77.42500000273119554, 28.56700777964554661 ) ) ;
#2681 = ADVANCED_FACE ( 'NONE', ( #33276, #14755 ), #20772, .F. ) ;
#2682 = CARTESIAN_POINT ( 'NONE',  ( -10.04305231718578462, 54.39999999999999147, 30.90933677959249337 ) ) ;
#2683 = CARTESIAN_POINT ( 'NONE',  ( -23.41746825000000243, 15.72499999726882081, 7.608796670333725309 ) ) ;
#2684 = CARTESIAN_POINT ( 'NONE',  ( 27.16883889988624290, 65.92500000273118133, 19.73931689729373673 ) ) ;
#2685 = CARTESIAN_POINT ( 'NONE',  ( -23.41746825000000598, 6.224999997268799490, 7.608796670333726198 ) ) ;
#2686 = CARTESIAN_POINT ( 'NONE',  ( 27.16883889988624290, 72.17500000273118133, 19.73931689729373673 ) ) ;
#2687 = CARTESIAN_POINT ( 'NONE',  ( -27.16883889988624290, 4.925000002731189319, -19.73931689729374028 ) ) ;
#2688 = CARTESIAN_POINT ( 'NONE',  ( -14.47279130897152122, 18.42499999726882365, 19.92008829642072243 ) ) ;
#2689 = CARTESIAN_POINT ( 'NONE',  ( 26.09010956794232428, 11.14621500092397532, -6.950374756619718042 ) ) ;
#2690 = ORIENTED_EDGE ( 'NONE', *, *, #25523, .T. ) ;
#2691 = CARTESIAN_POINT ( 'NONE',  ( -33.58253175000000113, 41.02500000273118985, -10.91162601494193218 ) ) ;
#2692 = VERTEX_POINT ( 'NONE', #30872 ) ;
#2693 = CARTESIAN_POINT ( 'NONE',  ( -2.584737979205441561E-13, 43.36718749999999289, -30.02300923189239512 ) ) ;
#2694 = CARTESIAN_POINT ( 'NONE',  ( 32.50000000000000711, 11.40000000546237757, 10.55989012756945122 ) ) ;
#2695 = CARTESIAN_POINT ( 'NONE',  ( 32.50000000000000000, 5.500000005462371888, -3.980102097228898626E-15 ) ) ;
#2696 = CARTESIAN_POINT ( 'NONE',  ( -27.16883889988624290, 78.92500000273116711, -19.73931689729374028 ) ) ;
#2697 = CARTESIAN_POINT ( 'NONE',  ( -20.50609665441004736, 18.87499999999999645, -20.50609665440969565 ) ) ;
#2698 = CARTESIAN_POINT ( 'NONE',  ( 18.94512977948575738, 18.42499999726882010, 13.76444248337723408 ) ) ;
#2699 = CARTESIAN_POINT ( 'NONE',  ( 20.75514604977249178, 16.07500000273119412, 28.56700777964553950 ) ) ;
#2700 = CARTESIAN_POINT ( 'NONE',  ( -32.50000000000000000, 62.00000000000000000, 0.000000000000000000 ) ) ;
#2701 = DIRECTION ( 'NONE',  ( 0.000000000000000000, 1.000000000000000000, 0.000000000000000000 ) ) ;
#2702 = DIRECTION ( 'NONE',  ( 0.000000000000000000, 0.000000000000000000, 1.000000000000000000 ) ) ;
#2703 = CARTESIAN_POINT ( 'NONE',  ( 7.543491769121922985, 33.19232666574268364, 28.00173670424535644 ) ) ;
#2704 = CARTESIAN_POINT ( 'NONE',  ( 4.300734207923757602, 78.77500000273118985, -13.23629886949340673 ) ) ;
#2705 = CARTESIAN_POINT ( 'NONE',  ( 15.01150461594643382, 37.92447916666666430, 26.00068869287340334 ) ) ;
#2706 = DIRECTION ( 'NONE',  ( 0.000000000000000000, -1.000000000000000000, 0.000000000000000000 ) ) ;
#2707 = CARTESIAN_POINT ( 'NONE',  ( 19.82091636218621034, 15.80000000000000782, 14.40073868116559730 ) ) ;
#2708 = CARTESIAN_POINT ( 'NONE',  ( 20.08610463437158344, 2.700000000000001954, 27.64615127144129403 ) ) ;
#2709 = CARTESIAN_POINT ( 'NONE',  ( -2.375766604868041476, 74.44874571845315359, 14.99999999999999822 ) ) ;
#2710 = CARTESIAN_POINT ( 'NONE',  ( -6.950374756619247307, 64.41628499907602645, 26.09010956794245217 ) ) ;
#2711 = CARTESIAN_POINT ( 'NONE',  ( 33.58253175000000113, 48.22500000273119269, -10.91162601494193751 ) ) ;
#2712 = CARTESIAN_POINT ( 'NONE',  ( 33.58253175000000113, 56.47500000273116427, -10.91162601494193751 ) ) ;
#2713 = CARTESIAN_POINT ( 'NONE',  ( 27.16883889988624290, 34.17500000273118843, 19.73931689729373673 ) ) ;
#2714 = DIRECTION ( 'NONE',  ( 0.7069718413157916048, 0.01953538259431456675, -0.7069718413158002646 ) ) ;
#2715 = CARTESIAN_POINT ( 'NONE',  ( 26.29305231718579350, 15.30000000546238859, 19.10302069950537529 ) ) ;
#2716 = CYLINDRICAL_SURFACE ( 'NONE', #25592, 24.50000000000000000 ) ;
#2717 = CARTESIAN_POINT ( 'NONE',  ( -2.815509657234710744E-16, -20.70096189432334555, 0.000000000000000000 ) ) ;
#2718 = CARTESIAN_POINT ( 'NONE',  ( 27.16883889988623935, 14.32500000273119412, -19.73931689729374384 ) ) ;
#2719 = CARTESIAN_POINT ( 'NONE',  ( 5.147494310547434893, 6.551254281546842861, 32.49999999999999289 ) ) ;
#2720 = FACE_OUTER_BOUND ( 'NONE', #7788, .T. ) ;
#2721 = CARTESIAN_POINT ( 'NONE',  ( 15.14183272437242067, 9.449999994537636283, 20.84094480462498211 ) ) ;
#2722 = CARTESIAN_POINT ( 'NONE',  ( 24.22776226481265383, 15.57513916574268720, 13.94119854578893580 ) ) ;
#2723 = CARTESIAN_POINT ( 'NONE',  ( -32.50000000000000000, 34.40000000546236691, -10.55989012756945478 ) ) ;
#2724 = EDGE_CURVE ( 'NONE', #32915, #3462, #740, .T. ) ;
#2725 = CARTESIAN_POINT ( 'NONE',  ( -10.37757302488623701, 23.52500000273119340, 31.93888565452638417 ) ) ;
#2726 = CARTESIAN_POINT ( 'NONE',  ( 26.07999730980477437, 44.08333333333332860, -6.988114217768290004 ) ) ;
#2727 = ORIENTED_EDGE ( 'NONE', *, *, #33353, .T. ) ;
#2728 = CARTESIAN_POINT ( 'NONE',  ( -10.37757302488623701, 61.52500000273118985, 31.93888565452638417 ) ) ;
#2729 = EDGE_LOOP ( 'NONE', ( #11660, #5888, #17586, #12988 ) ) ;
#2730 = CARTESIAN_POINT ( 'NONE',  ( -15.01150461594642138, 19.01822916666666785, -26.00068869287340334 ) ) ;
#2731 = CARTESIAN_POINT ( 'NONE',  ( -7.468012846824771955, 10.28684000092397532, -28.02196122052045624 ) ) ;
#2732 = ORIENTED_EDGE ( 'NONE', *, *, #3020, .F. ) ;
#2733 = CARTESIAN_POINT ( 'NONE',  ( -33.58253175000000113, 5.225000002731188253, 10.91162601494193929 ) ) ;
#2734 = DIRECTION ( 'NONE',  ( -0.000000000000000000, 1.000000000000000000, -0.000000000000000000 ) ) ;
#2735 = CARTESIAN_POINT ( 'NONE',  ( 27.16883889988624290, 34.17500000273118843, 19.73931689729373673 ) ) ;
#2736 = CARTESIAN_POINT ( 'NONE',  ( 26.29305231718578995, 39.70000000546236407, -19.10302069950538240 ) ) ;
#2737 = CARTESIAN_POINT ( 'NONE',  ( -2.092463501923844636E-15, 79.49999999999998579, -34.17252228774368916 ) ) ;
#2738 = CARTESIAN_POINT ( 'NONE',  ( 15.01150461594596308, 64.27864583333332860, -26.00068869287367335 ) ) ;
#2739 = CARTESIAN_POINT ( 'NONE',  ( 19.82091636218621389, 5.949999994537630066, -14.40073868116559197 ) ) ;
#2740 = CARTESIAN_POINT ( 'NONE',  ( 33.58253175000000113, 50.37500000273120548, -4.112674001490185761E-15 ) ) ;
#2741 = CARTESIAN_POINT ( 'NONE',  ( 26.29305231718578995, 21.19999999999998153, -19.10302069950538240 ) ) ;
#2742 = CARTESIAN_POINT ( 'NONE',  ( 26.29305231718579350, 24.79999999999999005, 19.10302069950537529 ) ) ;
#2743 = CARTESIAN_POINT ( 'NONE',  ( -24.50000000000000000, 7.000000000000006217, -3.000384657911015469E-15 ) ) ;
#2744 = CARTESIAN_POINT ( 'NONE',  ( 20.75514604977249178, 69.82500000273118701, 28.56700777964553950 ) ) ;
#2745 = CARTESIAN_POINT ( 'NONE',  ( -32.79451539931719140, 66.99999999999994316, 5.771861194046820742 ) ) ;
#2746 = CARTESIAN_POINT ( 'NONE',  ( -10.58590195883389207, 74.00000000000001421, -10.62726115788808201 ) ) ;
#2747 = CARTESIAN_POINT ( 'NONE',  ( 27.16883889988623935, 60.57500000273119412, -19.73931689729374384 ) ) ;
#2748 = CARTESIAN_POINT ( 'NONE',  ( -4.934616302121927505E-14, 72.50000000000001421, 32.50000000000000000 ) ) ;
#2749 = CARTESIAN_POINT ( 'NONE',  ( -20.75514604977248823, 14.82500000273117635, -28.56700777964554305 ) ) ;
#2750 = CARTESIAN_POINT ( 'NONE',  ( 6.950374756619721595, 25.75559000092397710, 26.09010956794232428 ) ) ;
#2751 = CARTESIAN_POINT ( 'NONE',  ( 24.50000000000000000, 9.749999994537628112, 0.000000000000000000 ) ) ;
#2752 = CARTESIAN_POINT ( 'NONE',  ( 10.37757302488624056, 4.775000002731177418, -31.93888565452638417 ) ) ;
#2753 = CARTESIAN_POINT ( 'NONE',  ( -33.58253175000000113, 33.12500000273120548, 0.000000000000000000 ) ) ;
#2754 = CARTESIAN_POINT ( 'NONE',  ( 0.000000000000000000, 80.00000000000001421, 0.000000000000000000 ) ) ;
#2755 = CARTESIAN_POINT ( 'NONE',  ( 10.04305231718578817, 19.40000000000000213, -30.90933677959249337 ) ) ;
#2756 = CARTESIAN_POINT ( 'NONE',  ( 2.688165632520823219E-15, 75.37500000273118417, 14.63369212191046209 ) ) ;
#2757 = CARTESIAN_POINT ( 'NONE',  ( -14.97647472619899389, 43.93451416574269075, 26.02091320914878025 ) ) ;
#2758 = CARTESIAN_POINT ( 'NONE',  ( 10.04305231718578817, 53.90000000546239534, -30.90933677959249337 ) ) ;
#2759 = EDGE_CURVE ( 'NONE', #8583, #21853, #17675, .T. ) ;
#2760 = CARTESIAN_POINT ( 'NONE',  ( 11.25946833292375793, 76.57500000273120122, -8.180482586598735395 ) ) ;
#2761 = CARTESIAN_POINT ( 'NONE',  ( -6.988114217768288228, 15.72395833333332860, -26.07999730980477437 ) ) ;
#2762 =( BOUNDED_CURVE ( )  B_SPLINE_CURVE ( 2, ( #15329, #30407, #33502, #25448, #2449, #12915, #19959, #17559, #10178, #28361, #23220, #4848, #20478 ),
 .UNSPECIFIED., .F., .T. ) 
 B_SPLINE_CURVE_WITH_KNOTS ( ( 3, 2, 2, 2, 2, 2, 3 ),
 ( 0.07051282051282051211, 0.07179487179487178961, 0.07435897435897435848, 0.07692307692307692735, 0.07948717948717948234, 0.08205128205128205121, 0.08333333333333334259 ),
 .UNSPECIFIED. ) 
 CURVE ( )  GEOMETRIC_REPRESENTATION_ITEM ( )  RATIONAL_B_SPLINE_CURVE ( ( 0.9755282581475768211, 0.9755282581475768211, 1.000000000000000000, 0.9510565162951535312, 1.000000000000000000, 0.9510565162951535312, 1.000000000000000000, 0.9510565162951535312, 1.000000000000000000, 0.9510565162951535312, 1.000000000000000000, 0.9755282581475765991, 0.9755282581475767101 ) ) 
 REPRESENTATION_ITEM ( '' )  );
#2763 = CARTESIAN_POINT ( 'NONE',  ( -18.94512977948576093, 4.324999997268818674, 13.76444248337722698 ) ) ;
#2764 = EDGE_CURVE ( 'NONE', #21391, #5051, #15272, .T. ) ;
#2765 = CARTESIAN_POINT ( 'NONE',  ( -32.50000000000000000, 72.40000000546235981, -10.55989012756945478 ) ) ;
#2766 = CARTESIAN_POINT ( 'NONE',  ( -28.01184896238304134, 18.58854166666666430, -7.505752307972844761 ) ) ;
#2767 = CARTESIAN_POINT ( 'NONE',  ( -33.58253175000000113, 31.47500000273117493, 10.91162601494193929 ) ) ;
#2768 =( BOUNDED_CURVE ( )  B_SPLINE_CURVE ( 2, ( #26802, #21990, #3296, #19585, #6367, #19085, #11023, #32438, #9104, #27301, #703, #30033, #17011 ),
 .UNSPECIFIED., .F., .T. ) 
 B_SPLINE_CURVE_WITH_KNOTS ( ( 3, 2, 2, 2, 2, 2, 3 ),
 ( 0.08333333333333334259, 0.08888888888888889228, 0.1000000000000000056, 0.1111111111111111049, 0.1222222222222222182, 0.1333333333333333315, 0.1388888888888888673 ),
 .UNSPECIFIED. ) 
 CURVE ( )  GEOMETRIC_REPRESENTATION_ITEM ( )  RATIONAL_B_SPLINE_CURVE ( ( 0.9755282581475768211, 0.9755282581475768211, 1.000000000000000000, 0.9510565162951535312, 1.000000000000000000, 0.9510565162951535312, 1.000000000000000000, 0.9510565162951535312, 1.000000000000000000, 0.9510565162951535312, 1.000000000000000000, 0.9755282581475768211, 0.9755282581475768211 ) ) 
 REPRESENTATION_ITEM ( '' )  );
#2769 = CARTESIAN_POINT ( 'NONE',  ( -23.41746824999999887, 12.12499999726882116, -2.867812753649727150E-15 ) ) ;
#2770 = VERTEX_POINT ( 'NONE', #1870 ) ;
#2771 = CARTESIAN_POINT ( 'NONE',  ( 20.53372385742072481, 38.35975666759064495, -20.47846945139902175 ) ) ;
#2772 = CARTESIAN_POINT ( 'NONE',  ( -26.29305231718579350, 18.30000000546237615, -19.10302069950537884 ) ) ;
#2773 = CARTESIAN_POINT ( 'NONE',  ( 2.740863092043355209E-13, 51.96093750000000000, 30.02300923189239512 ) ) ;
#2774 = DIRECTION ( 'NONE',  ( -0.000000000000000000, -1.000000000000000000, -0.000000000000000000 ) ) ;
#2775 = CARTESIAN_POINT ( 'NONE',  ( 33.58253175000000113, 54.47500000273117138, -10.91162601494193751 ) ) ;
#2776 = CARTESIAN_POINT ( 'NONE',  ( -20.08610463437157989, 54.20000000546237118, -27.64615127144129758 ) ) ;
#2777 = CARTESIAN_POINT ( 'NONE',  ( -13.91746824999999532, 77.47500000273117848, 4.522059556121122093 ) ) ;
#2778 = CARTESIAN_POINT ( 'NONE',  ( -10.37757302488623701, 39.52500000273118275, 31.93888565452638417 ) ) ;
#2779 = CARTESIAN_POINT ( 'NONE',  ( 20.08610463437158344, 54.69999999999998153, 27.64615127144129403 ) ) ;
#2780 = CARTESIAN_POINT ( 'NONE',  ( 10.37757302488624767, 67.97500000273117848, 31.93888565452638417 ) ) ;
#2781 = LINE ( 'NONE', #21154, #30983 ) ;
#2782 = CARTESIAN_POINT ( 'NONE',  ( -33.58253175000000113, 61.02500000273118985, -10.91162601494193041 ) ) ;
#2783 = CARTESIAN_POINT ( 'NONE',  ( -30.02300923189239867, 25.32031250000000000, 2.654126918244514854E-13 ) ) ;
#2784 = CARTESIAN_POINT ( 'NONE',  ( -32.50000000000000000, 46.09999999999999432, 10.55989012756946366 ) ) ;
#2785 = CARTESIAN_POINT ( 'NONE',  ( 18.94512977948575738, 2.424999997268806329, 13.76444248337723408 ) ) ;
#2786 = CARTESIAN_POINT ( 'NONE',  ( 33.58253175000000113, 8.475000002731173154, -10.91162601494193751 ) ) ;
#2787 = CARTESIAN_POINT ( 'NONE',  ( 2.445080149700053643E-15, 72.75000000546238255, 15.00000000000000000 ) ) ;
#2788 = CARTESIAN_POINT ( 'NONE',  ( -19.11951029504797006, 34.62461833240934794, -19.06425588902558133 ) ) ;
#2789 = CARTESIAN_POINT ( 'NONE',  ( 30.00000000000001066, -91.00000000000000000, 0.000000000000000000 ) ) ;
#2790 = CYLINDRICAL_SURFACE ( 'NONE', #29718, 32.50000000000000000 ) ;
#2791 = DIRECTION ( 'NONE',  ( -0.000000000000000000, 1.000000000000000000, -0.000000000000000000 ) ) ;
#2792 = CARTESIAN_POINT ( 'NONE',  ( -33.58253175000000113, 73.37500000273118417, 0.000000000000000000 ) ) ;
#2793 = ORIENTED_EDGE ( 'NONE', *, *, #24665, .F. ) ;
#2794 = CARTESIAN_POINT ( 'NONE',  ( -7.236395654485757944, 17.72499999726881370, -22.27133577429736988 ) ) ;
#2795 = CARTESIAN_POINT ( 'NONE',  ( 2.584737979205441561E-13, 55.39843749999999289, 27.95245687107222921 ) ) ;
#2796 = CARTESIAN_POINT ( 'NONE',  ( 33.58253175000000113, 56.22500000273117138, -10.91162601494193751 ) ) ;
#2797 = CARTESIAN_POINT ( 'NONE',  ( 27.16883889988623935, 18.57500000273119767, -19.73931689729374384 ) ) ;
#2798 = CARTESIAN_POINT ( 'NONE',  ( 27.16883889988623935, 6.575000002731187898, -19.73931689729374384 ) ) ;
#2799 = CARTESIAN_POINT ( 'NONE',  ( -19.09188309203694445, 39.49999999999999289, -19.09188309203661049 ) ) ;
#2800 = CARTESIAN_POINT ( 'NONE',  ( 7.468012846824777284, 32.63059000092395934, 28.02196122052045268 ) ) ;
#2801 = CARTESIAN_POINT ( 'NONE',  ( 30.02300923189239867, 15.28868083240935505, -0.04044903255044467877 ) ) ;
#2802 = CARTESIAN_POINT ( 'NONE',  ( 10.04305231718578817, 71.90000000546238823, -30.90933677959249337 ) ) ;
#2803 = CARTESIAN_POINT ( 'NONE',  ( 20.18813247507400988, 51.99999999999998579, -25.94218825114888105 ) ) ;
#2804 = CARTESIAN_POINT ( 'NONE',  ( -33.58253175000000113, 39.22500000273119269, 10.91162601494193929 ) ) ;
#2805 = CARTESIAN_POINT ( 'NONE',  ( 26.06988505166722803, 49.52045166574269075, -7.025853678916862854 ) ) ;
#2806 = CARTESIAN_POINT ( 'NONE',  ( -23.41746824999999887, 11.62499999726881938, -2.867812753649727150E-15 ) ) ;
#2807 = CARTESIAN_POINT ( 'NONE',  ( -1.778240108872766143E-15, 2.000000005462374997, -32.49999999999999289 ) ) ;
#2808 = ORIENTED_EDGE ( 'NONE', *, *, #26669, .F. ) ;
#2809 = CARTESIAN_POINT ( 'NONE',  ( -33.58253175000000113, 51.27500000273118275, -10.91162601494193218 ) ) ;
#2810 = LINE ( 'NONE', #26980, #2022 ) ;
#2811 = CARTESIAN_POINT ( 'NONE',  ( 7.025853678916403666, 41.51079833425730214, -26.06988505166735237 ) ) ;
#2812 = CARTESIAN_POINT ( 'NONE',  ( 33.58253175000000823, 70.27500000273118985, 10.91162601494192863 ) ) ;
#2813 = EDGE_LOOP ( 'NONE', ( #32705, #11051, #23902, #10204 ) ) ;
#2814 = CARTESIAN_POINT ( 'NONE',  ( 6.486482029760649416E-15, 23.62500000273119127, 35.31076352940723240 ) ) ;
#2815 = CARTESIAN_POINT ( 'NONE',  ( -28.01184896238290278, 28.61458333333333215, 7.505752307973363457 ) ) ;
#2816 = ORIENTED_EDGE ( 'NONE', *, *, #21130, .T. ) ;
#2817 = CARTESIAN_POINT ( 'NONE',  ( -26.29305231718579350, 14.30000000546238681, -19.10302069950537884 ) ) ;
#2818 = CARTESIAN_POINT ( 'NONE',  ( 27.16883889988623935, 62.32500000273119412, -19.73931689729374384 ) ) ;
#2819 = CARTESIAN_POINT ( 'NONE',  ( -30.02300923189239512, 52.82031249999997868, 2.654126918244515359E-13 ) ) ;
#2820 = DIRECTION ( 'NONE',  ( 0.000000000000000000, -1.000000000000000000, 0.000000000000000000 ) ) ;
#2821 = CARTESIAN_POINT ( 'NONE',  ( 23.41746824999999887, 7.024999997268802865, 7.608796670333735079 ) ) ;
#2822 = EDGE_CURVE ( 'NONE', #4956, #8605, #4255, .T. ) ;
#2823 = CARTESIAN_POINT ( 'NONE',  ( -20.75514604977248112, 5.425000002731182214, 28.56700777964554661 ) ) ;
#2824 = CARTESIAN_POINT ( 'NONE',  ( -27.16883889988623935, 29.57500000273119412, 19.73931689729374739 ) ) ;
#2825 = CARTESIAN_POINT ( 'NONE',  ( 10.04305231718578817, 5.900000005462368691, -30.90933677959249337 ) ) ;
#2826 = CARTESIAN_POINT ( 'NONE',  ( 26.02091320914876960, 60.26263916574269786, 14.97647472619900455 ) ) ;
#2827 = CARTESIAN_POINT ( 'NONE',  ( -24.50000000000000000, 14.89999999999999503, -7.960532557706207157 ) ) ;
#2828 = CARTESIAN_POINT ( 'NONE',  ( -13.91746824999999532, 78.97500000273117848, 4.522059556121122093 ) ) ;
#2829 = CARTESIAN_POINT ( 'NONE',  ( 10.04305231718579705, 8.599999999999996092, 30.90933677959248982 ) ) ;
#2830 = CARTESIAN_POINT ( 'NONE',  ( -32.50000000000000000, 18.09999999999998010, 10.55989012756946366 ) ) ;
#2831 = CARTESIAN_POINT ( 'NONE',  ( -19.09188309203694445, 60.12500000000000000, -19.09188309203661049 ) ) ;
#2832 = CARTESIAN_POINT ( 'NONE',  ( -24.50000000000000355, 18.64999999453763380, -7.960532557706207157 ) ) ;
#2833 = CARTESIAN_POINT ( 'NONE',  ( 13.91746824999999532, 79.97500000273117848, -4.522059556121118540 ) ) ;
#2834 = CARTESIAN_POINT ( 'NONE',  ( -24.20753774853730889, 35.34635416666666430, 13.97622843553633842 ) ) ;
#2835 = CARTESIAN_POINT ( 'NONE',  ( 33.58253175000000113, 22.12500000273118062, -4.112674001490185761E-15 ) ) ;
#2836 = CARTESIAN_POINT ( 'NONE',  ( 27.16883889988624290, 71.92500000273120975, 19.73931689729373673 ) ) ;
#2837 = AXIS2_PLACEMENT_3D ( 'NONE', #5449, #28608, #23309 ) ;
#2838 = CARTESIAN_POINT ( 'NONE',  ( 10.37757302488624056, 36.77500000273118985, -31.93888565452638417 ) ) ;
#2839 = CARTESIAN_POINT ( 'NONE',  ( 10.37757302488624056, 12.77500000273118452, -31.93888565452638417 ) ) ;
#2840 = CARTESIAN_POINT ( 'NONE',  ( -3.880418787951136483, 6.551254281546842861, -24.50000000000000000 ) ) ;
#2841 = CARTESIAN_POINT ( 'NONE',  ( 24.22776226481241224, 59.12798583425730925, -13.94119854578936923 ) ) ;
#2842 = CARTESIAN_POINT ( 'NONE',  ( -10.37757302488623701, 77.52500000273118985, 31.93888565452638417 ) ) ;
#2843 = CYLINDRICAL_SURFACE ( 'NONE', #14633, 32.50000000000000000 ) ;
#2844 = CARTESIAN_POINT ( 'NONE',  ( 20.08610463437158344, 56.69999999999998153, 27.64615127144129403 ) ) ;
#2845 = CARTESIAN_POINT ( 'NONE',  ( 15.00000000000000000, 79.35000000546239107, -4.873795443493596835 ) ) ;
#2846 = CARTESIAN_POINT ( 'NONE',  ( 27.16883889988623935, 60.32500000273119412, -19.73931689729374384 ) ) ;
#2847 = CARTESIAN_POINT ( 'NONE',  ( -23.41746825000000598, 10.22499999726881903, 7.608796670333726198 ) ) ;
#2848 = ORIENTED_EDGE ( 'NONE', *, *, #15661, .T. ) ;
#2849 = CARTESIAN_POINT ( 'NONE',  ( 10.37757302488624056, 74.77500000273117564, -31.93888565452638417 ) ) ;
#2850 = CARTESIAN_POINT ( 'NONE',  ( -32.50000000000000000, 62.09999999999998721, 10.55989012756946366 ) ) ;
#2851 = CARTESIAN_POINT ( 'NONE',  ( -7.236395654485757944, 15.72499999726881192, -22.27133577429736988 ) ) ;
#2852 = CARTESIAN_POINT ( 'NONE',  ( 7.025853678916403666, 14.01079833425730747, -26.06988505166735237 ) ) ;
#2853 = EDGE_CURVE ( 'NONE', #27023, #19766, #20254, .T. ) ;
#2854 = ORIENTED_EDGE ( 'NONE', *, *, #32725, .T. ) ;
#2855 = CARTESIAN_POINT ( 'NONE',  ( 27.16883889988624290, 41.92500000273118133, 19.73931689729373673 ) ) ;
#2856 = CARTESIAN_POINT ( 'NONE',  ( 24.50000000000000000, -16.99999999999999289, 3.000384657911015469E-15 ) ) ;
#2857 = ORIENTED_EDGE ( 'NONE', *, *, #17508, .T. ) ;
#2858 = CARTESIAN_POINT ( 'NONE',  ( 7.505752307973351023, 41.50520833333333570, 28.01184896238290278 ) ) ;
#2859 = CARTESIAN_POINT ( 'NONE',  ( -32.50000000000000000, 60.50000000546238965, 0.000000000000000000 ) ) ;
#2860 = CARTESIAN_POINT ( 'NONE',  ( -26.29305231718579350, 6.300000005462380592, -19.10302069950537884 ) ) ;
#2861 = CARTESIAN_POINT ( 'NONE',  ( -20.75514604977248823, 78.82500000273120122, -28.56700777964554305 ) ) ;
#2862 = CARTESIAN_POINT ( 'NONE',  ( 7.505752307973351023, 17.44270833333333215, 28.01184896238290278 ) ) ;
#2863 = EDGE_CURVE ( 'NONE', #24126, #29527, #11362, .T. ) ;
#2864 = CARTESIAN_POINT ( 'NONE',  ( -23.41746825000000243, 15.52499999726882507, -7.608796670333730638 ) ) ;
#2865 = CARTESIAN_POINT ( 'NONE',  ( 10.37757302488624056, 10.77500000273118275, -31.93888565452638417 ) ) ;
#2866 =( BOUNDED_CURVE ( )  B_SPLINE_CURVE ( 2, ( #25754, #18386, #15979, #10651, #31408, #15294, #13055, #33988, #28491, #15811, #26435, #12544, #12713 ),
 .UNSPECIFIED., .F., .F. ) 
 B_SPLINE_CURVE_WITH_KNOTS ( ( 3, 2, 2, 2, 2, 2, 3 ),
 ( 0.1730769230769230727, 0.1743589743589743501, 0.1769230769230769329, 0.1794871794871794879, 0.1820512820512820429, 0.1846153846153846256, 0.1858974358974359031 ),
 .UNSPECIFIED. ) 
 CURVE ( )  GEOMETRIC_REPRESENTATION_ITEM ( )  RATIONAL_B_SPLINE_CURVE ( ( 0.9755282581475768211, 0.9755282581475768211, 1.000000000000000000, 0.9510565162951535312, 1.000000000000000000, 0.9510565162951535312, 1.000000000000000000, 0.9510565162951535312, 1.000000000000000000, 0.9510565162951535312, 1.000000000000000000, 0.9755282581475768211, 0.9755282581475768211 ) ) 
 REPRESENTATION_ITEM ( '' )  );
#2867 = CARTESIAN_POINT ( 'NONE',  ( -2.092463501923844636E-15, 59.50000000000001421, -34.17252228774368916 ) ) ;
#2868 = CARTESIAN_POINT ( 'NONE',  ( 4.300734207923757602, 80.27500000273118985, -13.23629886949340673 ) ) ;
#2869 = CYLINDRICAL_SURFACE ( 'NONE', #23639, 24.50000000000000000 ) ;
#2870 = CARTESIAN_POINT ( 'NONE',  ( -28.02196122052058413, 34.33815999907601224, -7.468012846824272799 ) ) ;
#2871 = CARTESIAN_POINT ( 'NONE',  ( 13.91746824999999532, 78.47500000273116427, -4.522059556121118540 ) ) ;
#2872 = CARTESIAN_POINT ( 'NONE',  ( 28.01184896238290278, 44.08333333333332860, -7.505752307973347470 ) ) ;
#2873 = ITEM_DEFINED_TRANSFORMATION ( 'NONE', 'NONE', #4082,  #1376 ) ;
#2874 = ADVANCED_FACE ( 'NONE', ( #5478 ), #31637, .T. ) ;
#2875 = CARTESIAN_POINT ( 'NONE',  ( 0.000000000000000000, 82.00000000000001421, 0.000000000000000000 ) ) ;
#2876 = CARTESIAN_POINT ( 'NONE',  ( -1.756012107511856980E-14, 6.249999994537623671, -24.50000000000000000 ) ) ;
#2877 = CARTESIAN_POINT ( 'NONE',  ( 32.50000000000000000, 3.000000000000002665, -3.980102097228898626E-15 ) ) ;
#2878 = CARTESIAN_POINT ( 'NONE',  ( 0.000000000000000000, 80.00000000000001421, 0.000000000000000000 ) ) ;
#2879 = CARTESIAN_POINT ( 'NONE',  ( -0.04044903255042732459, 62.55430583240935505, -27.95245687107223986 ) ) ;
#2880 = CARTESIAN_POINT ( 'NONE',  ( 10.37757302488624056, 42.52500000273118275, -31.93888565452638417 ) ) ;
#2881 = AXIS2_PLACEMENT_3D ( 'NONE', #29621, #3394, #6124 ) ;
#2882 = CARTESIAN_POINT ( 'NONE',  ( -9.270509831248425314, 71.95000000546239960, -12.75976212528059861 ) ) ;
#2883 = CARTESIAN_POINT ( 'NONE',  ( 33.58253175000000113, 56.37500000273119838, -4.112674001490185761E-15 ) ) ;
#2884 = CARTESIAN_POINT ( 'NONE',  ( -20.75514604977248823, 37.07500000273120122, -28.56700777964554305 ) ) ;
#2885 = CARTESIAN_POINT ( 'NONE',  ( 26.29305231718578995, 23.70000000546237828, -19.10302069950538240 ) ) ;
#2886 = CARTESIAN_POINT ( 'NONE',  ( -26.07999730980477437, 25.17708333333332860, 6.988114217768305103 ) ) ;
#2887 = CARTESIAN_POINT ( 'NONE',  ( -4.223320258572819786E-15, 9.499999999999992895, 24.50000000000000000 ) ) ;
#2888 = CARTESIAN_POINT ( 'NONE',  ( 32.50000000000000711, 51.40000000546238823, 10.55989012756945122 ) ) ;
#2889 = CARTESIAN_POINT ( 'NONE',  ( -32.50000000000000000, 72.00000000000000000, 0.000000000000000000 ) ) ;
#2890 = CARTESIAN_POINT ( 'NONE',  ( -20.75514604977248112, 15.42500000273118843, 28.56700777964554661 ) ) ;
#2891 = CARTESIAN_POINT ( 'NONE',  ( -3.880418787951174675, 12.30125427608447275, -24.49999999999998579 ) ) ;
#2892 = CARTESIAN_POINT ( 'NONE',  ( 7.570916362186213000, 10.14999999453763913, -23.30088464923126423 ) ) ;
#2893 = CARTESIAN_POINT ( 'NONE',  ( 6.950374756619257965, 18.01003499907601935, -26.09010956794244507 ) ) ;
#2894 = CARTESIAN_POINT ( 'NONE',  ( -10.04305231718578462, 34.90000000546238113, 30.90933677959249337 ) ) ;
#2895 = CARTESIAN_POINT ( 'NONE',  ( -20.08610463437157989, 11.70000000000000817, -27.64615127144129758 ) ) ;
#2896 = CARTESIAN_POINT ( 'NONE',  ( 6.486482029760648627E-15, 25.62500000273118417, 35.31076352940722529 ) ) ;
#2897 = CARTESIAN_POINT ( 'NONE',  ( 27.95245687107222921, 40.78906249999998579, -2.463307335887066074E-13 ) ) ;
#2898 = ORIENTED_EDGE ( 'NONE', *, *, #20671, .T. ) ;
#2899 = CARTESIAN_POINT ( 'NONE',  ( -2.162160676586881955E-15, 64.62500000273121259, -35.31076352940723240 ) ) ;
#2900 = ORIENTED_EDGE ( 'NONE', *, *, #181, .F. ) ;
#2901 = CARTESIAN_POINT ( 'NONE',  ( -20.50609665440969209, 14.57812499999999645, 20.50609665441005092 ) ) ;
#2902 = CARTESIAN_POINT ( 'NONE',  ( 7.543491769121427382, 17.44829833425730925, -28.00173670424548433 ) ) ;
#2903 = VECTOR ( 'NONE', #2592, 1000.000000000000000 ) ;
#2904 = CARTESIAN_POINT ( 'NONE',  ( -20.75514604977248823, 6.825000002731195892, -28.56700777964554305 ) ) ;
#2905 = VERTEX_POINT ( 'NONE', #2567 ) ;
#2906 = CARTESIAN_POINT ( 'NONE',  ( 0.000000000000000000, 80.00000000000001421, 0.000000000000000000 ) ) ;
#2907 = CARTESIAN_POINT ( 'NONE',  ( 33.58253175000000823, 28.27500000273118985, 10.91162601494192863 ) ) ;
#2908 =( BOUNDED_CURVE ( )  B_SPLINE_CURVE ( 2, ( #17410, #22724, #12074, #28382, #30427, #4527, #20156, #27872, #33172, #7616, #1948, #33525, #12769 ),
 .UNSPECIFIED., .F., .F. ) 
 B_SPLINE_CURVE_WITH_KNOTS ( ( 3, 2, 2, 2, 2, 2, 3 ),
 ( 0.7243589743589743390, 0.7256410256410256165, 0.7282051282051281715, 0.7307692307692307265, 0.7333333333333332815, 0.7358974358974359475, 0.7371794871794872250 ),
 .UNSPECIFIED. ) 
 CURVE ( )  GEOMETRIC_REPRESENTATION_ITEM ( )  RATIONAL_B_SPLINE_CURVE ( ( 0.9755282581475768211, 0.9755282581475768211, 1.000000000000000000, 0.9510565162951535312, 1.000000000000000000, 0.9510565162951535312, 1.000000000000000000, 0.9510565162951535312, 1.000000000000000000, 0.9510565162951535312, 1.000000000000000000, 0.9755282581475768211, 0.9755282581475768211 ) ) 
 REPRESENTATION_ITEM ( '' )  );
#2909 = CARTESIAN_POINT ( 'NONE',  ( 6.277390505771533514E-15, 35.00000000546237544, 34.17252228774368916 ) ) ;
#2910 = CARTESIAN_POINT ( 'NONE',  ( 32.50000000000000711, 76.89999999999999147, 10.55989012756945122 ) ) ;
#2911 = DIRECTION ( 'NONE',  ( -0.000000000000000000, -1.000000000000000000, -0.000000000000000000 ) ) ;
#2912 = CARTESIAN_POINT ( 'NONE',  ( 2.489536152421872915E-14, 77.50000000000001421, -32.49999999999999289 ) ) ;
#2913 = CARTESIAN_POINT ( 'NONE',  ( 27.16883889988623935, 42.57500000273117990, -19.73931689729374384 ) ) ;
#2914 = SHAPE_DEFINITION_REPRESENTATION ( #5242, #5873 ) ;
#2915 = CARTESIAN_POINT ( 'NONE',  ( 26.29305231718579350, 20.80000000000000071, 19.10302069950537529 ) ) ;
#2916 = CARTESIAN_POINT ( 'NONE',  ( 20.08610463437157279, 23.29999999999999361, -27.64615127144129758 ) ) ;
#2917 = CARTESIAN_POINT ( 'NONE',  ( -15.14183272437241889, 8.700000000000017053, -20.84094480462497856 ) ) ;
#2918 = CARTESIAN_POINT ( 'NONE',  ( -20.75514604977248112, 69.42500000273116711, 28.56700777964554661 ) ) ;
#2919 = CARTESIAN_POINT ( 'NONE',  ( 2.489536152421872915E-14, 76.00000000546238255, -32.49999999999999289 ) ) ;
#2920 = CARTESIAN_POINT ( 'NONE',  ( -10.37757302488624411, 56.97500000273119980, -31.93888565452638417 ) ) ;
#2921 = CARTESIAN_POINT ( 'NONE',  ( 10.04305231718578817, 7.900000005462370467, -30.90933677959249337 ) ) ;
#2922 = CARTESIAN_POINT ( 'NONE',  ( -27.16883889988623935, 9.325000002731176352, 19.73931689729374739 ) ) ;
#2923 = CARTESIAN_POINT ( 'NONE',  ( -26.09010956794232428, 30.05246500092397000, 6.950374756619732253 ) ) ;
#2924 = CARTESIAN_POINT ( 'NONE',  ( 24.50000000000000000, 9.649999994537628467, 7.960532557706212486 ) ) ;
#2925 = CARTESIAN_POINT ( 'NONE',  ( -17.00271606754838416, 51.99999999999998579, 28.39578712880047462 ) ) ;
#2926 = CARTESIAN_POINT ( 'NONE',  ( 33.58253175000000113, 32.12500000273120548, -4.112674001490185761E-15 ) ) ;
#2927 = CARTESIAN_POINT ( 'NONE',  ( -20.08610463437156923, 18.80000000546237260, 27.64615127144130113 ) ) ;
#2928 = CARTESIAN_POINT ( 'NONE',  ( 33.58253175000000823, 52.27500000273118275, 10.91162601494192685 ) ) ;
#2929 = VECTOR ( 'NONE', #28226, 1000.000000000000000 ) ;
#2930 = CARTESIAN_POINT ( 'NONE',  ( 8.601468415847516980, 78.17500000273120975, -11.83890561707634603 ) ) ;
#2931 = CARTESIAN_POINT ( 'NONE',  ( -0.04044903255044120238, 48.80430583240936215, -30.02300923189239867 ) ) ;
#2932 = CARTESIAN_POINT ( 'NONE',  ( -20.08610463437157989, 54.20000000546237118, -27.64615127144129758 ) ) ;
#2933 = CARTESIAN_POINT ( 'NONE',  ( -4.300734207923755825, 75.77500000273118985, 13.23629886949340673 ) ) ;
#2934 = FILL_AREA_STYLE_COLOUR ( '', #19452 ) ;
#2935 = CARTESIAN_POINT ( 'NONE',  ( 27.95245687107222921, 13.28906249999999289, -2.463307335887066074E-13 ) ) ;
#2936 = CARTESIAN_POINT ( 'NONE',  ( -20.08610463437157989, 70.20000000546237118, -27.64615127144129758 ) ) ;
#2937 = CARTESIAN_POINT ( 'NONE',  ( 28.01184896238304134, 20.30729166666666430, 7.505752307972846538 ) ) ;
#2938 = CARTESIAN_POINT ( 'NONE',  ( -27.16883889988623935, 31.57500000273118346, 19.73931689729374739 ) ) ;
#2939 = CARTESIAN_POINT ( 'NONE',  ( 23.41746824999999887, 11.22499999726881548, -7.608796670333727974 ) ) ;
#2940 = EDGE_LOOP ( 'NONE', ( #4959, #14793, #18981, #27682 ) ) ;
#2941 = CARTESIAN_POINT ( 'NONE',  ( -28.00173670424549499, 37.21392333425730214, -7.543491769121417612 ) ) ;
#2942 = CARTESIAN_POINT ( 'NONE',  ( -32.50000000000000000, 16.40000000546239178, -10.55989012756945478 ) ) ;
#2943 = CARTESIAN_POINT ( 'NONE',  ( -20.50609665440969209, 52.39062499999999289, 20.50609665441005092 ) ) ;
#2944 = CARTESIAN_POINT ( 'NONE',  ( -20.50609665441004736, 67.00000000000000000, -20.50609665440969565 ) ) ;
#2945 = CARTESIAN_POINT ( 'NONE',  ( 33.58253175000000823, 52.27500000273118985, 10.91162601494192863 ) ) ;
#2946 = CARTESIAN_POINT ( 'NONE',  ( 6.277390505771533514E-15, 59.00000000546238255, 34.17252228774368916 ) ) ;
#2947 = CARTESIAN_POINT ( 'NONE',  ( -13.91746824999999532, 77.27500000273117564, -4.522059556121115875 ) ) ;
#2948 = CARTESIAN_POINT ( 'NONE',  ( 27.16883889988624290, 37.92500000273118843, 19.73931689729373673 ) ) ;
#2949 = DIRECTION ( 'NONE',  ( 0.000000000000000000, -0.000000000000000000, -1.000000000000000000 ) ) ;
#2950 = CARTESIAN_POINT ( 'NONE',  ( -2.162160676586881955E-15, 66.87500000273119838, -35.31076352940723240 ) ) ;
#2951 = CARTESIAN_POINT ( 'NONE',  ( -26.29305231718578995, 0.7000000054623867207, 19.10302069950538595 ) ) ;
#2952 = VECTOR ( 'NONE', #28754, 1000.000000000000114 ) ;
#2953 = CARTESIAN_POINT ( 'NONE',  ( 6.486482029760648627E-15, 59.62500000273118417, 35.31076352940722529 ) ) ;
#2954 = CARTESIAN_POINT ( 'NONE',  ( -15.01150461594595775, 21.30989583333332504, 26.00068869287368756 ) ) ;
#2955 = CARTESIAN_POINT ( 'NONE',  ( -32.50000000000000000, 37.89999999999999858, -10.55989012756945478 ) ) ;
#2956 = CARTESIAN_POINT ( 'NONE',  ( -18.94512977948575738, 7.424999997268811214, -13.76444248337723231 ) ) ;
#2957 = ADVANCED_FACE ( 'NONE', ( #15621 ), #18365, .T. ) ;
#2958 = CARTESIAN_POINT ( 'NONE',  ( 33.58253175000000823, 8.275000002731179194, 10.91162601494192863 ) ) ;
#2959 = CARTESIAN_POINT ( 'NONE',  ( 3.880418787951134707, 19.30125427608447808, 24.50000000000000000 ) ) ;
#2960 = CARTESIAN_POINT ( 'NONE',  ( -26.06988505166722803, 34.05170166574267654, 7.025853678916877953 ) ) ;
#2961 = CARTESIAN_POINT ( 'NONE',  ( 5.779280353836490358E-15, 53.00000000546238255, 32.49999999999999289 ) ) ;
#2962 = CARTESIAN_POINT ( 'NONE',  ( 20.75514604977249178, 70.07500000273120122, 28.56700777964553950 ) ) ;
#2963 = DIRECTION ( 'NONE',  ( -0.000000000000000000, -1.000000000000000000, -0.000000000000000000 ) ) ;
#2964 = ADVANCED_FACE ( 'NONE', ( #28810 ), #8047, .T. ) ;
#2965 = CARTESIAN_POINT ( 'NONE',  ( -27.16883889988623935, 67.57500000273118701, 19.73931689729374739 ) ) ;
#2966 = VERTEX_POINT ( 'NONE', #10799 ) ;
#2967 = CARTESIAN_POINT ( 'NONE',  ( -23.41746825000000243, 18.02499999726880731, -7.608796670333730638 ) ) ;
#2968 = CARTESIAN_POINT ( 'NONE',  ( -13.97622843553588901, 62.55989583333332860, 24.20753774853756823 ) ) ;
#2969 = CARTESIAN_POINT ( 'NONE',  ( 10.37757302488624767, 51.72500000273121401, 31.93888565452638417 ) ) ;
#2970 = CARTESIAN_POINT ( 'NONE',  ( 20.75514604977248467, 18.67500000273120264, -28.56700777964554305 ) ) ;
#2971 = CARTESIAN_POINT ( 'NONE',  ( -33.58253175000000113, 3.275000002731191628, -10.91162601494193218 ) ) ;
#2972 = CARTESIAN_POINT ( 'NONE',  ( 13.97622843553633842, 41.36197916666665719, 24.20753774853730889 ) ) ;
#2973 =( BOUNDED_CURVE ( )  B_SPLINE_CURVE ( 2, ( #18754, #2959, #5361, #18588, #8430, #16012, #26466 ),
 .UNSPECIFIED., .F., .T. ) 
 B_SPLINE_CURVE_WITH_KNOTS ( ( 3, 2, 2, 3 ),
 ( 0.9722222222222222099, 0.9777777777777777457, 0.9888888888888889284, 1.000000000000000000 ),
 .UNSPECIFIED. ) 
 CURVE ( )  GEOMETRIC_REPRESENTATION_ITEM ( )  RATIONAL_B_SPLINE_CURVE ( ( 0.9755282581475768211, 0.9755282581475768211, 1.000000000000000000, 0.9510565162951535312, 1.000000000000000000, 0.9510565162951535312, 1.000000000000000000 ) ) 
 REPRESENTATION_ITEM ( '' )  );
#2974 = CARTESIAN_POINT ( 'NONE',  ( -30.02300923189239867, 30.19569416759064140, -0.04044903254991731589 ) ) ;
#2975 = CARTESIAN_POINT ( 'NONE',  ( 15.04653450569339945, 22.73659749907601935, 25.98046417659831775 ) ) ;
#2976 = CARTESIAN_POINT ( 'NONE',  ( 32.50000000000000000, 75.50000000546238255, -3.980102097228898626E-15 ) ) ;
#2977 = CARTESIAN_POINT ( 'NONE',  ( 31.78338918835718729, 52.00000000000002132, -9.699108655006703827 ) ) ;
#2978 = VECTOR ( 'NONE', #33292, 1000.000000000000000 ) ;
#2979 = CARTESIAN_POINT ( 'NONE',  ( 6.486482029760648627E-15, 37.62500000273118417, 35.31076352940722529 ) ) ;
#2980 = CARTESIAN_POINT ( 'NONE',  ( 26.06988505166722803, 46.08295166574269075, -7.025853678916862854 ) ) ;
#2981 = CARTESIAN_POINT ( 'NONE',  ( 23.41746824999999887, 18.62499999726882649, 0.000000000000000000 ) ) ;
#2982 = FACE_OUTER_BOUND ( 'NONE', #23459, .T. ) ;
#2983 = ORIENTED_EDGE ( 'NONE', *, *, #609, .F. ) ;
#2984 = CARTESIAN_POINT ( 'NONE',  ( -10.37757302488623701, 49.77500000273120406, 31.93888565452638417 ) ) ;
#2985 = CARTESIAN_POINT ( 'NONE',  ( 15.00000000000000355, 76.90000000000000568, 4.873795443493592394 ) ) ;
#2986 = CARTESIAN_POINT ( 'NONE',  ( 27.95245687107223986, 49.10194416759064495, 0.04044903254993640479 ) ) ;
#2987 = CARTESIAN_POINT ( 'NONE',  ( 6.486482029760649416E-15, 71.87500000273116996, 35.31076352940723240 ) ) ;
#2988 = ORIENTED_EDGE ( 'NONE', *, *, #22050, .F. ) ;
#2989 = CARTESIAN_POINT ( 'NONE',  ( -33.58253175000000113, 15.12500000273118950, 0.000000000000000000 ) ) ;
#2990 = CARTESIAN_POINT ( 'NONE',  ( -15.01150461594595775, 24.74739583333332504, 26.00068869287368756 ) ) ;
#2991 = EDGE_LOOP ( 'NONE', ( #1711, #23249, #6389, #2164 ) ) ;
#2992 = CARTESIAN_POINT ( 'NONE',  ( 20.75514604977248467, 60.42500000273118133, -28.56700777964554305 ) ) ;
#2993 = CARTESIAN_POINT ( 'NONE',  ( -28.01184896238290278, 45.80208333333333570, 7.505752307973363457 ) ) ;
#2994 = CARTESIAN_POINT ( 'NONE',  ( -20.08610463437156923, 18.80000000546237615, 27.64615127144130113 ) ) ;
#2995 = CARTESIAN_POINT ( 'NONE',  ( -7.570916362186210335, 16.60000000000000497, -23.30088464923126779 ) ) ;
#2996 = CARTESIAN_POINT ( 'NONE',  ( 14.47279130897151767, 6.824999997268808904, 19.92008829642072953 ) ) ;
#2997 = CARTESIAN_POINT ( 'NONE',  ( -27.16883889988623935, 5.325000002731172799, 19.73931689729374739 ) ) ;
#2998 = CARTESIAN_POINT ( 'NONE',  ( -27.16883889988624290, 29.17500000273118133, -19.73931689729374028 ) ) ;
#2999 = FACE_OUTER_BOUND ( 'NONE', #2645, .T. ) ;
#3000 = CARTESIAN_POINT ( 'NONE',  ( -30.02300923189239867, 58.25743083240935505, 0.04044903255044988294 ) ) ;
#3001 = CYLINDRICAL_SURFACE ( 'NONE', #24012, 32.50000000000000000 ) ;
#3002 = CARTESIAN_POINT ( 'NONE',  ( 13.91746824999999532, 79.97500000273117848, -4.522059556121118540 ) ) ;
#3003 = CARTESIAN_POINT ( 'NONE',  ( 5.779280353836490358E-15, 60.49999999999998579, 32.49999999999999289 ) ) ;
#3004 = CARTESIAN_POINT ( 'NONE',  ( -10.04305231718579172, 15.59999999999998899, -30.90933677959248982 ) ) ;
#3005 = CARTESIAN_POINT ( 'NONE',  ( 26.07999730980490227, 61.55729166666666430, 6.988114217767821046 ) ) ;
#3006 = ADVANCED_FACE ( 'NONE', ( #8379 ), #3078, .F. ) ;
#3007 = CARTESIAN_POINT ( 'NONE',  ( -24.50000000000000000, 16.74999999453763522, -3.000384657911015469E-15 ) ) ;
#3008 = CARTESIAN_POINT ( 'NONE',  ( 8.601468415847520532, 77.57500000273118701, 11.83890561707634781 ) ) ;
#3009 = CARTESIAN_POINT ( 'NONE',  ( 24.20753774853756113, 30.76302083333332504, 13.97622843553589789 ) ) ;
#3010 = CARTESIAN_POINT ( 'NONE',  ( 20.75514604977249178, 27.82500000273116925, 28.56700777964553950 ) ) ;
#3011 = CARTESIAN_POINT ( 'NONE',  ( -33.58253175000000113, 73.12500000273118417, 0.000000000000000000 ) ) ;
#3012 = CARTESIAN_POINT ( 'NONE',  ( -10.37757302488623701, 35.77500000273118985, 31.93888565452638417 ) ) ;
#3013 = CARTESIAN_POINT ( 'NONE',  ( 20.75514604977248467, 16.67500000273117422, -28.56700777964554305 ) ) ;
#3014 = CARTESIAN_POINT ( 'NONE',  ( 14.01125832528286352, 58.84152750092397355, -24.18731323226246843 ) ) ;
#3015 = CARTESIAN_POINT ( 'NONE',  ( -27.16883889988623935, 71.32500000273117280, 19.73931689729374739 ) ) ;
#3016 = CARTESIAN_POINT ( 'NONE',  ( 10.04305231718578817, 3.900000005462367358, -30.90933677959249337 ) ) ;
#3017 = CARTESIAN_POINT ( 'NONE',  ( -2.092463501923844636E-15, 51.50000000000000711, -34.17252228774368916 ) ) ;
#3018 = CARTESIAN_POINT ( 'NONE',  ( -8.891200544363830713E-16, 71.75000000546238255, -15.00000000000000000 ) ) ;
#3019 = CARTESIAN_POINT ( 'NONE',  ( -33.58253175000000113, 59.02500000273120406, -10.91162601494193041 ) ) ;
#3020 = EDGE_CURVE ( 'NONE', #33486, #14415, #23846, .T. ) ;
#3021 = CARTESIAN_POINT ( 'NONE',  ( -18.94512977948575738, 13.92499999726881654, -13.76444248337723231 ) ) ;
#3022 = VECTOR ( 'NONE', #33435, 1000.000000000000000 ) ;
#3023 = ORIENTED_EDGE ( 'NONE', *, *, #32629, .T. ) ;
#3024 = CARTESIAN_POINT ( 'NONE',  ( 10.37757302488624767, 65.97500000273119269, 31.93888565452638417 ) ) ;
#3025 = CARTESIAN_POINT ( 'NONE',  ( -20.08610463437157989, 61.69999999999999574, -27.64615127144129758 ) ) ;
#3026 = CARTESIAN_POINT ( 'NONE',  ( -23.41746825000000598, 1.724999997268824581, 7.608796670333726198 ) ) ;
#3027 = CARTESIAN_POINT ( 'NONE',  ( -13.94119854578936923, 23.89361083425731280, -24.22776226481241224 ) ) ;
#3028 = ORIENTED_EDGE ( 'NONE', *, *, #2332, .F. ) ;
#3029 = CARTESIAN_POINT ( 'NONE',  ( -10.37757302488624411, 40.72500000273119980, -31.93888565452638417 ) ) ;
#3030 = CARTESIAN_POINT ( 'NONE',  ( -26.29305231718579350, 68.30000000546237970, -19.10302069950537884 ) ) ;
#3031 = EDGE_LOOP ( 'NONE', ( #5870, #24956 ) ) ;
#3032 = CARTESIAN_POINT ( 'NONE',  ( -15.01150461594595775, 45.37239583333333570, 26.00068869287368756 ) ) ;
#3033 = CARTESIAN_POINT ( 'NONE',  ( 32.50000000000000711, 4.899999999999990585, 10.55989012756945122 ) ) ;
#3034 = CARTESIAN_POINT ( 'NONE',  ( 5.147494310547426899, 59.44874571845315359, -32.50000000000000000 ) ) ;
#3035 = CARTESIAN_POINT ( 'NONE',  ( 20.08610463437158344, 27.20000000546237118, 27.64615127144129403 ) ) ;
#3036 = CARTESIAN_POINT ( 'NONE',  ( 28.01184896238304134, 23.74479166666666430, 7.505752307972846538 ) ) ;
#3037 = CARTESIAN_POINT ( 'NONE',  ( -14.47279130897151589, 17.32499999726882933, -19.92008829642072598 ) ) ;
#3038 = CARTESIAN_POINT ( 'NONE',  ( -10.37757302488624411, 8.975000002731187365, -31.93888565452638417 ) ) ;
#3039 = AXIS2_PLACEMENT_3D ( 'NONE', #4768, #14730, #15246 ) ;
#3040 = CARTESIAN_POINT ( 'NONE',  ( -2.092463501923844636E-15, 61.50000000000000000, -34.17252228774368916 ) ) ;
#3041 = CARTESIAN_POINT ( 'NONE',  ( -13.91746824999999887, 78.87500000273118417, 0.000000000000000000 ) ) ;
#3042 = DIRECTION ( 'NONE',  ( 0.000000000000000000, 1.000000000000000000, 0.000000000000000000 ) ) ;
#3043 = CARTESIAN_POINT ( 'NONE',  ( -15.04653450569338524, 31.33034749907602290, -25.98046417659831775 ) ) ;
#3044 = CARTESIAN_POINT ( 'NONE',  ( 8.601468415847516980, 78.67500000273119554, -11.83890561707634781 ) ) ;
#3045 = CARTESIAN_POINT ( 'NONE',  ( 26.00068869287341045, 50.81510416666666430, -15.01150461594642493 ) ) ;
#3046 = FACE_OUTER_BOUND ( 'NONE', #9410, .T. ) ;
#3047 = DIRECTION ( 'NONE',  ( -0.7071067811865462405, 0.7071067811865489050, 0.000000000000000000 ) ) ;
#3048 = CARTESIAN_POINT ( 'NONE',  ( -32.50000000000000000, 2.099999999999991651, 10.55989012756946366 ) ) ;
#3049 = VECTOR ( 'NONE', #18827, 1000.000000000000000 ) ;
#3050 = CARTESIAN_POINT ( 'NONE',  ( 32.50000000000000000, 17.60000000546238397, -10.55989012756945833 ) ) ;
#3051 = CARTESIAN_POINT ( 'NONE',  ( -13.94119854578892514, 61.12201416574268364, 24.22776226481266448 ) ) ;
#3052 = CARTESIAN_POINT ( 'NONE',  ( -27.16883889988623935, 45.32500000273117990, 19.73931689729374739 ) ) ;
#3053 = CARTESIAN_POINT ( 'NONE',  ( -8.601468415847515203, 79.17500000273116711, 11.83890561707634959 ) ) ;
#3054 = CARTESIAN_POINT ( 'NONE',  ( -33.58253175000000113, 57.47500000273119269, 10.91162601494193929 ) ) ;
#3055 = CARTESIAN_POINT ( 'NONE',  ( 33.58253175000000113, 34.47500000273119269, -10.91162601494193574 ) ) ;
#3056 = CARTESIAN_POINT ( 'NONE',  ( 10.04305231718579705, 23.10000000546236265, 30.90933677959248982 ) ) ;
#3057 = CARTESIAN_POINT ( 'NONE',  ( 13.97622843553633842, 20.73697916666666075, 24.20753774853730889 ) ) ;
#3058 = CARTESIAN_POINT ( 'NONE',  ( -4.223320258572819786E-15, 11.24999999453762456, 24.50000000000000000 ) ) ;
#3059 = CARTESIAN_POINT ( 'NONE',  ( 26.29305231718578995, 31.20000000000000639, -19.10302069950538240 ) ) ;
#3060 = CARTESIAN_POINT ( 'NONE',  ( -10.04305231718579172, 75.59999999999998010, -30.90933677959248982 ) ) ;
#3061 = VECTOR ( 'NONE', #7554, 1000.000000000000000 ) ;
#3062 = CARTESIAN_POINT ( 'NONE',  ( -33.58253175000000113, 11.02500000273117919, -10.91162601494193218 ) ) ;
#3063 = CARTESIAN_POINT ( 'NONE',  ( -23.41746824999999887, 3.524999997268825958, -7.608796670333730638 ) ) ;
#3064 = CIRCLE ( 'NONE', #11810, 15.00000000000000000 ) ;
#3065 = FACE_OUTER_BOUND ( 'NONE', #27303, .T. ) ;
#3066 = CARTESIAN_POINT ( 'NONE',  ( 14.01125832528330051, 26.17409749907601935, 24.18731323226221974 ) ) ;
#3067 = CARTESIAN_POINT ( 'NONE',  ( -19.82091636218621034, 12.80000000000000604, -14.40073868116559552 ) ) ;
#3068 = CARTESIAN_POINT ( 'NONE',  ( -10.37757302488623701, 17.52500000273118985, 31.93888565452638417 ) ) ;
#3069 = CARTESIAN_POINT ( 'NONE',  ( 6.988114217768294445, 48.38020833333332860, 26.07999730980477437 ) ) ;
#3070 = ORIENTED_EDGE ( 'NONE', *, *, #20795, .T. ) ;
#3071 = CARTESIAN_POINT ( 'NONE',  ( -20.75514604977248112, 61.42500000273118133, 28.56700777964554661 ) ) ;
#3072 =( BOUNDED_CURVE ( )  B_SPLINE_CURVE ( 2, ( #29163, #24036, #504, #10990, #21462, #26929, #31905, #21628, #8399, #5837, #3262, #24200, #32073 ),
 .UNSPECIFIED., .F., .T. ) 
 B_SPLINE_CURVE_WITH_KNOTS ( ( 3, 2, 2, 2, 2, 2, 3 ),
 ( 0.1858974358974359031, 0.1871794871794871806, 0.1897435897435897356, 0.1923076923076923184, 0.1948717948717948734, 0.1974358974358974284, 0.1987179487179487336 ),
 .UNSPECIFIED. ) 
 CURVE ( )  GEOMETRIC_REPRESENTATION_ITEM ( )  RATIONAL_B_SPLINE_CURVE ( ( 0.9755282581475768211, 0.9755282581475768211, 1.000000000000000000, 0.9510565162951535312, 1.000000000000000000, 0.9510565162951535312, 1.000000000000000000, 0.9510565162951535312, 1.000000000000000000, 0.9510565162951535312, 1.000000000000000000, 0.9755282581475764880, 0.9755282581475768211 ) ) 
 REPRESENTATION_ITEM ( '' )  );
#3073 = ORIENTED_EDGE ( 'NONE', *, *, #13138, .T. ) ;
#3074 = CARTESIAN_POINT ( 'NONE',  ( -2.584737979205441561E-13, 12.42968749999999289, -30.02300923189239512 ) ) ;
#3075 = CARTESIAN_POINT ( 'NONE',  ( -0.04044903254990864921, 19.02381916759064495, 30.02300923189239867 ) ) ;
#3076 = CARTESIAN_POINT ( 'NONE',  ( -33.58253175000000113, 7.025000002731188964, -10.91162601494193218 ) ) ;
#3077 = VERTEX_POINT ( 'NONE', #26246 ) ;
#3078 = PLANE ( 'NONE',  #11914 ) ;
#3079 = CARTESIAN_POINT ( 'NONE',  ( -33.58253175000000113, 29.27500000273118630, -10.91162601494193218 ) ) ;
#3080 = CARTESIAN_POINT ( 'NONE',  ( 32.50000000000000711, 39.40000000546236691, 10.55989012756945122 ) ) ;
#3081 = AXIS2_PLACEMENT_3D ( 'NONE', #13260, #2631, #31944 ) ;
#3082 = CARTESIAN_POINT ( 'NONE',  ( -32.50000000000000000, 77.90000000000001990, -10.55989012756945478 ) ) ;
#3083 = CARTESIAN_POINT ( 'NONE',  ( 5.204170427930421283E-15, -70.99969134886156041, 0.000000000000000000 ) ) ;
#3084 = LINE ( 'NONE', #22111, #29632 ) ;
#3085 = CARTESIAN_POINT ( 'NONE',  ( -20.75514604977248823, 43.07500000273118701, -28.56700777964554305 ) ) ;
#3086 = CARTESIAN_POINT ( 'NONE',  ( -32.50000000000000000, 23.90000000000000213, -10.55989012756945478 ) ) ;
#3087 = CARTESIAN_POINT ( 'NONE',  ( -32.50000000000000000, 20.10000000000000497, 10.55989012756946366 ) ) ;
#3088 = CARTESIAN_POINT ( 'NONE',  ( -15.14183272437241889, 2.700000000000001954, -20.84094480462497856 ) ) ;
#3089 = EDGE_CURVE ( 'NONE', #5024, #24073, #13710, .T. ) ;
#3090 = CARTESIAN_POINT ( 'NONE',  ( -2.162160676586881955E-15, 62.62500000273116996, -35.31076352940723240 ) ) ;
#3091 = CARTESIAN_POINT ( 'NONE',  ( -20.08610463437157989, 77.70000000000001705, -27.64615127144129758 ) ) ;
#3092 = CARTESIAN_POINT ( 'NONE',  ( -0.3491184494335538013, 73.99999999999998579, -14.58811049051102415 ) ) ;
#3093 = CARTESIAN_POINT ( 'NONE',  ( -27.16883889988624290, 51.17500000273117422, -19.73931689729374028 ) ) ;
#3094 = CARTESIAN_POINT ( 'NONE',  ( 23.41746824999999887, 2.724999997268822138, -7.608796670333727974 ) ) ;
#3095 = CARTESIAN_POINT ( 'NONE',  ( 10.04305231718579705, 39.10000000546237686, 30.90933677959248982 ) ) ;
#3096 = CARTESIAN_POINT ( 'NONE',  ( 33.58253175000000113, 6.225000002731185589, -10.91162601494193751 ) ) ;
#3097 = CARTESIAN_POINT ( 'NONE',  ( 19.06425588902592239, 28.90663166759063785, 19.11951029504763611 ) ) ;
#3098 = CARTESIAN_POINT ( 'NONE',  ( 22.34582402162608616, 66.99999999999998579, -24.25905220314542277 ) ) ;
#3099 = CARTESIAN_POINT ( 'NONE',  ( 1.093617666956751375E-13, 66.00000000546238255, -32.50000000000000711 ) ) ;
#3100 = UNCERTAINTY_MEASURE_WITH_UNIT (LENGTH_MEASURE( 1.000000000000000082E-05 ), #27441, 'distance_accuracy_value', 'NONE');
#3101 = CARTESIAN_POINT ( 'NONE',  ( -27.16883889988624290, 32.92500000273117422, -19.73931689729374028 ) ) ;
#3102 = CARTESIAN_POINT ( 'NONE',  ( -32.50000000000000000, 18.50000000546236834, 0.000000000000000000 ) ) ;
#3103 = CARTESIAN_POINT ( 'NONE',  ( 32.50000000000000000, 61.50000000546239676, -3.980102097228898626E-15 ) ) ;
#3104 = CARTESIAN_POINT ( 'NONE',  ( 4.300734207923757602, 78.27500000273118985, -13.23629886949340673 ) ) ;
#3105 = CARTESIAN_POINT ( 'NONE',  ( 30.02300923189239867, 46.22618083240936215, -0.04044903255044467877 ) ) ;
#3106 = CARTESIAN_POINT ( 'NONE',  ( 20.08610463437158344, 57.20000000546237828, 27.64615127144129403 ) ) ;
#3107 = CARTESIAN_POINT ( 'NONE',  ( -11.25946833292375793, 73.17500000273119554, -8.180482586598733619 ) ) ;
#3108 = DIRECTION ( 'NONE',  ( -0.000000000000000000, -1.000000000000000000, -0.000000000000000000 ) ) ;
#3109 = CARTESIAN_POINT ( 'NONE',  ( 24.20753774853731244, 16.44010416666666430, -13.97622843553632599 ) ) ;
#3110 = CARTESIAN_POINT ( 'NONE',  ( 32.50000000000000000, 71.50000000546235412, -3.980102097228898626E-15 ) ) ;
#3111 = CARTESIAN_POINT ( 'NONE',  ( 26.00068869287340334, 19.87760416666666430, -15.01150461594642316 ) ) ;
#3112 = CARTESIAN_POINT ( 'NONE',  ( 18.94512977948576093, 15.32499999726880091, -13.76444248337722875 ) ) ;
#3113 = ORIENTED_EDGE ( 'NONE', *, *, #27812, .T. ) ;
#3114 = CARTESIAN_POINT ( 'NONE',  ( 28.02196122052045268, 38.64621500092395934, -7.468012846824774620 ) ) ;
#3115 = CARTESIAN_POINT ( 'NONE',  ( -2.092463501923844636E-15, 20.00000000546236834, -34.17252228774368916 ) ) ;
#3116 = CARTESIAN_POINT ( 'NONE',  ( 2.740863092043355209E-13, 48.52343750000000000, 30.02300923189239512 ) ) ;
#3117 = CARTESIAN_POINT ( 'NONE',  ( 5.147494310547434893, 74.55125428154683220, 32.49999999999999289 ) ) ;
#3118 = CARTESIAN_POINT ( 'NONE',  ( 6.486482029760649416E-15, 49.87500000273119838, 35.31076352940723240 ) ) ;
#3119 = CARTESIAN_POINT ( 'NONE',  ( -20.08610463437157989, 56.20000000546239249, -27.64615127144129758 ) ) ;
#3120 = CARTESIAN_POINT ( 'NONE',  ( 2.688165632520823219E-15, 75.87500000273115575, 14.63369212191046387 ) ) ;
#3121 = CARTESIAN_POINT ( 'NONE',  ( -27.16883889988624290, 34.92500000273118843, -19.73931689729374028 ) ) ;
#3122 = CARTESIAN_POINT ( 'NONE',  ( 20.75514604977248467, 62.67500000273117422, -28.56700777964554305 ) ) ;
#3123 = CARTESIAN_POINT ( 'NONE',  ( 0.000000000000000000, 111.9999999999999858, 0.000000000000000000 ) ) ;
#3124 = CARTESIAN_POINT ( 'NONE',  ( -1.778240108872766143E-15, 23.49999999999999645, -32.49999999999999289 ) ) ;
#3125 = CARTESIAN_POINT ( 'NONE',  ( 20.50609665441005092, 17.15624999999999645, 20.50609665440969209 ) ) ;
#3126 = CARTESIAN_POINT ( 'NONE',  ( -20.08610463437157989, 41.69999999999999574, -27.64615127144129758 ) ) ;
#3127 = CARTESIAN_POINT ( 'NONE',  ( 1.507698388325705758E-15, 3.124999997268809615, -24.62258325217400312 ) ) ;
#3128 = CARTESIAN_POINT ( 'NONE',  ( 6.486482029760649416E-15, 5.875000002731167292, 35.31076352940723240 ) ) ;
#3129 = CARTESIAN_POINT ( 'NONE',  ( 32.50000000000000000, 35.60000000546237686, -10.55989012756945833 ) ) ;
#3130 = CARTESIAN_POINT ( 'NONE',  ( 11.25946833292375793, 72.17500000273119554, 8.180482586598731842 ) ) ;
#3131 = CARTESIAN_POINT ( 'NONE',  ( -10.37757302488624411, 72.97500000273119269, -31.93888565452638417 ) ) ;
#3132 = DIRECTION ( 'NONE',  ( 0.000000000000000000, -0.000000000000000000, 1.000000000000000000 ) ) ;
#3133 = CARTESIAN_POINT ( 'NONE',  ( -20.75514604977248112, 71.67500000273116711, 28.56700777964554661 ) ) ;
#3134 = ORIENTED_EDGE ( 'NONE', *, *, #25934, .T. ) ;
#3135 = AXIS2_PLACEMENT_3D ( 'NONE', #6451, #6110, #16590 ) ;
#3136 = DIRECTION ( 'NONE',  ( -0.000000000000000000, -1.000000000000000000, -0.000000000000000000 ) ) ;
#3137 = CARTESIAN_POINT ( 'NONE',  ( 13.97622843553589966, 64.27864583333332860, -24.20753774853756113 ) ) ;
#3138 = CARTESIAN_POINT ( 'NONE',  ( -33.58253175000000113, 51.02500000273119696, -10.91162601494193218 ) ) ;
#3139 = CARTESIAN_POINT ( 'NONE',  ( -27.16883889988623935, 9.575000002731190563, 19.73931689729374739 ) ) ;
#3140 = CARTESIAN_POINT ( 'NONE',  ( -2.162160676586881955E-15, 4.875000002731200155, -35.31076352940723240 ) ) ;
#3141 = CARTESIAN_POINT ( 'NONE',  ( -24.20753774853730889, 42.22135416666666430, 13.97622843553634020 ) ) ;
#3142 = CARTESIAN_POINT ( 'NONE',  ( -7.468012846824771955, 30.91184000092396644, -28.02196122052045624 ) ) ;
#3143 = AXIS2_PLACEMENT_3D ( 'NONE', #16484, #26940, #3440 ) ;
#3144 = CARTESIAN_POINT ( 'NONE',  ( 28.00173670424535644, 18.58295166574268364, -7.543491769121920321 ) ) ;
#3145 = CARTESIAN_POINT ( 'NONE',  ( 26.29305231718578995, 75.70000000546238539, -19.10302069950538240 ) ) ;
#3146 = CARTESIAN_POINT ( 'NONE',  ( -20.08610463437157989, 56.20000000546238539, -27.64615127144129758 ) ) ;
#3147 = CARTESIAN_POINT ( 'NONE',  ( 6.486482029760648627E-15, 41.62500000273116285, 35.31076352940722529 ) ) ;
#3148 = CARTESIAN_POINT ( 'NONE',  ( 13.94119854578893580, 49.09076416574269786, -24.22776226481265383 ) ) ;
#3149 = CARTESIAN_POINT ( 'NONE',  ( -7.236395654485763274, 14.02499999726880553, 22.27133577429736633 ) ) ;
#3150 = DIRECTION ( 'NONE',  ( -1.000000000000000000, -1.416100796715761110E-16, 0.000000000000000000 ) ) ;
#3151 = ORIENTED_EDGE ( 'NONE', *, *, #9021, .F. ) ;
#3152 = ADVANCED_FACE ( 'NONE', ( #24010 ), #5814, .F. ) ;
#3153 = CARTESIAN_POINT ( 'NONE',  ( -10.37757302488624411, 44.97500000273117848, -31.93888565452638417 ) ) ;
#3154 = LINE ( 'NONE', #13784, #21763 ) ;
#3155 = CARTESIAN_POINT ( 'NONE',  ( -26.06988505166735237, 54.40142333425730925, -7.025853678916388567 ) ) ;
#3156 = CARTESIAN_POINT ( 'NONE',  ( -27.16883889988624290, 71.17500000273119554, -19.73931689729374028 ) ) ;
#3157 = EDGE_CURVE ( 'NONE', #9414, #21926, #16291, .T. ) ;
#3158 = ORIENTED_EDGE ( 'NONE', *, *, #25617, .T. ) ;
#3159 = CARTESIAN_POINT ( 'NONE',  ( 33.58253175000000113, 16.22500000273118914, -10.91162601494193751 ) ) ;
#3160 = CARTESIAN_POINT ( 'NONE',  ( 26.00068869287367335, 20.45052083333332504, 15.01150461594596308 ) ) ;
#3161 = ORIENTED_EDGE ( 'NONE', *, *, #22557, .F. ) ;
#3162 = CARTESIAN_POINT ( 'NONE',  ( 32.50000000000000711, 65.40000000546237402, 10.55989012756945122 ) ) ;
#3163 = CARTESIAN_POINT ( 'NONE',  ( -27.16883889988624290, 54.92500000273120264, -19.73931689729374028 ) ) ;
#3164 = CARTESIAN_POINT ( 'NONE',  ( -15.01150461594642138, 49.95572916666665009, -26.00068869287340334 ) ) ;
#3165 = AXIS2_PLACEMENT_3D ( 'NONE', #16128, #3242, #24176 ) ;
#3166 = CARTESIAN_POINT ( 'NONE',  ( 26.29305231718579350, 15.30000000546238859, 19.10302069950537529 ) ) ;
#3167 = CARTESIAN_POINT ( 'NONE',  ( -1.756012107511856980E-14, 2.500000000000005773, -24.50000000000000000 ) ) ;
#3168 = CARTESIAN_POINT ( 'NONE',  ( -14.47279130897151767, 5.824999997268811569, -19.92008829642072598 ) ) ;
#3169 = CARTESIAN_POINT ( 'NONE',  ( -10.37757302488624411, 28.97500000273117848, -31.93888565452638417 ) ) ;
#3170 = CYLINDRICAL_SURFACE ( 'NONE', #1166, 27.00000000000000000 ) ;
#3171 = CARTESIAN_POINT ( 'NONE',  ( 15.04653450569339945, 63.98659749907601935, 25.98046417659831775 ) ) ;
#3172 = CARTESIAN_POINT ( 'NONE',  ( -34.92499999999992610, 0.000000000000000000, 0.000000000000000000 ) ) ;
#3173 = CARTESIAN_POINT ( 'NONE',  ( -26.29305231718578995, 4.199999999999981526, 19.10302069950538595 ) ) ;
#3174 =( BOUNDED_CURVE ( )  B_SPLINE_CURVE ( 2, ( #22328, #20439, #30890, #9436, #3960, #31565, #5153, #25748, #7557, #28486, #10475, #28657, #10310 ),
 .UNSPECIFIED., .F., .F. ) 
 B_SPLINE_CURVE_WITH_KNOTS ( ( 3, 2, 2, 2, 2, 2, 3 ),
 ( 0.4807692307692307820, 0.4820512820512820595, 0.4846153846153846145, 0.4871794871794871695, 0.4897435897435897245, 0.4923076923076923350, 0.4935897435897436125 ),
 .UNSPECIFIED. ) 
 CURVE ( )  GEOMETRIC_REPRESENTATION_ITEM ( )  RATIONAL_B_SPLINE_CURVE ( ( 0.9755282581475768211, 0.9755282581475768211, 1.000000000000000000, 0.9510565162951535312, 1.000000000000000000, 0.9510565162951535312, 1.000000000000000000, 0.9510565162951535312, 1.000000000000000000, 0.9510565162951535312, 1.000000000000000000, 0.9755282581475768211, 0.9755282581475768211 ) ) 
 REPRESENTATION_ITEM ( '' )  );
#3175 = CARTESIAN_POINT ( 'NONE',  ( 32.50000000000000711, 12.90000000000000036, 10.55989012756945122 ) ) ;
#3176 = CARTESIAN_POINT ( 'NONE',  ( -26.07999730980477437, 62.98958333333332149, 6.988114217768305103 ) ) ;
#3177 = CARTESIAN_POINT ( 'NONE',  ( -24.50000000000001066, 16.84999999453763309, 7.960532557706201828 ) ) ;
#3178 = CARTESIAN_POINT ( 'NONE',  ( -13.91746824999999887, 76.87500000273116996, 0.000000000000000000 ) ) ;
#3179 = CARTESIAN_POINT ( 'NONE',  ( 19.09188309203661049, 30.04687500000000000, -19.09188309203694445 ) ) ;
#3180 = CARTESIAN_POINT ( 'NONE',  ( -33.58253175000000113, 23.02500000273117919, -10.91162601494193218 ) ) ;
#3181 = CARTESIAN_POINT ( 'NONE',  ( -33.58253175000000113, 71.12500000273118417, 0.000000000000000000 ) ) ;
#3182 = CARTESIAN_POINT ( 'NONE',  ( -10.37757302488624411, 30.97500000273119269, -31.93888565452638417 ) ) ;
#3183 = CARTESIAN_POINT ( 'NONE',  ( 10.37757302488624767, 17.97500000273119625, 31.93888565452638417 ) ) ;
#3184 = CARTESIAN_POINT ( 'NONE',  ( 24.18731323226247554, 59.70090250092397355, 14.01125832528285997 ) ) ;
#3185 = CARTESIAN_POINT ( 'NONE',  ( 10.37757302488624056, 68.52500000273120406, -31.93888565452638417 ) ) ;
#3186 = CARTESIAN_POINT ( 'NONE',  ( 20.08610463437158344, 59.20000000546237828, 27.64615127144129403 ) ) ;
#3187 = CARTESIAN_POINT ( 'NONE',  ( 32.50000000000000711, 50.89999999999999858, 10.55989012756945122 ) ) ;
#3188 = CARTESIAN_POINT ( 'NONE',  ( 3.445340210940985210E-14, 7.249999994537621895, 24.50000000000000000 ) ) ;
#3189 = CARTESIAN_POINT ( 'NONE',  ( 20.75514604977248467, 58.42500000273119554, -28.56700777964554305 ) ) ;
#3190 = CARTESIAN_POINT ( 'NONE',  ( -18.94512977948575738, 17.92499999726882010, -13.76444248337723231 ) ) ;
#3191 = AXIS2_PLACEMENT_3D ( 'NONE', #22795, #4600, #25545 ) ;
#3192 = EDGE_CURVE ( 'NONE', #24073, #25557, #13036, .T. ) ;
#3193 = VERTEX_POINT ( 'NONE', #10459 ) ;
#3194 = CARTESIAN_POINT ( 'NONE',  ( -20.75514604977248823, 69.07500000273115859, -28.56700777964554305 ) ) ;
#3195 = CARTESIAN_POINT ( 'NONE',  ( -5.147494310547213736, 15.55125428154684641, -32.50000000000007105 ) ) ;
#3196 = CARTESIAN_POINT ( 'NONE',  ( 14.47279130897151767, 8.924999997268800556, -19.92008829642072598 ) ) ;
#3197 = CARTESIAN_POINT ( 'NONE',  ( -27.95245687107223986, 19.88319416759064495, -0.04044903254993292840 ) ) ;
#3198 = ADVANCED_FACE ( 'NONE', ( #31720 ), #15848, .F. ) ;
#3199 = ORIENTED_EDGE ( 'NONE', *, *, #2527, .T. ) ;
#3200 = CARTESIAN_POINT ( 'NONE',  ( -27.16883889988623935, 37.32500000273118701, 19.73931689729374739 ) ) ;
#3201 = FACE_OUTER_BOUND ( 'NONE', #9127, .T. ) ;
#3202 = ORIENTED_EDGE ( 'NONE', *, *, #9641, .T. ) ;
#3203 = CARTESIAN_POINT ( 'NONE',  ( 20.50609665441005092, 48.09375000000000000, 20.50609665440969209 ) ) ;
#3204 = CARTESIAN_POINT ( 'NONE',  ( 5.779280353836490358E-15, 11.00000000546238077, 32.49999999999999289 ) ) ;
#3205 = CARTESIAN_POINT ( 'NONE',  ( 10.04305231718579705, 58.60000000000000142, 30.90933677959248982 ) ) ;
#3206 = CARTESIAN_POINT ( 'NONE',  ( 20.75514604977248467, 74.42500000273119554, -28.56700777964554305 ) ) ;
#3207 = CARTESIAN_POINT ( 'NONE',  ( 26.00068869287367335, 20.45052083333332504, 15.01150461594596308 ) ) ;
#3208 = CARTESIAN_POINT ( 'NONE',  ( -4.732186688966233175E-15, 1.500000000000010880, 25.76082449383753925 ) ) ;
#3209 = CARTESIAN_POINT ( 'NONE',  ( 20.75514604977248467, 8.675000002731195536, -28.56700777964554305 ) ) ;
#3210 = CARTESIAN_POINT ( 'NONE',  ( -33.58253175000000113, 21.02500000273117919, -10.91162601494193218 ) ) ;
#3211 = CARTESIAN_POINT ( 'NONE',  ( 2.688165632520823219E-15, 79.37500000273119838, 14.63369212191046209 ) ) ;
#3212 = DIRECTION ( 'NONE',  ( -0.000000000000000000, 1.000000000000000000, -0.000000000000000000 ) ) ;
#3213 = CARTESIAN_POINT ( 'NONE',  ( 20.53372385742108008, 32.90586833240934794, 20.47846945139866648 ) ) ;
#3214 = CARTESIAN_POINT ( 'NONE',  ( 2.688165632520823219E-15, 73.87500000273119838, 14.63369212191046387 ) ) ;
#3215 = CARTESIAN_POINT ( 'NONE',  ( 20.50609665440969565, 47.23437499999999289, -20.50609665441004736 ) ) ;
#3216 = CYLINDRICAL_SURFACE ( 'NONE', #32141, 15.00000000000000000 ) ;
#3217 = CARTESIAN_POINT ( 'NONE',  ( -32.50000000000000000, 54.60000000546237686, 10.55989012756946366 ) ) ;
#3218 = CARTESIAN_POINT ( 'NONE',  ( 13.94119854578893580, 59.40326416574269075, -24.22776226481265383 ) ) ;
#3219 = CARTESIAN_POINT ( 'NONE',  ( -10.37757302488623701, 41.52500000273118275, 31.93888565452638417 ) ) ;
#3220 = CARTESIAN_POINT ( 'NONE',  ( -9.270509831248421762, 72.55000000546239391, 12.75976212528060039 ) ) ;
#3221 = CARTESIAN_POINT ( 'NONE',  ( 20.75514604977249178, 54.07500000273118701, 28.56700777964553950 ) ) ;
#3222 = CARTESIAN_POINT ( 'NONE',  ( -10.37757302488623701, 35.77500000273120406, 31.93888565452638417 ) ) ;
#3223 = CARTESIAN_POINT ( 'NONE',  ( 0.000000000000000000, 96.00000000000002842, 0.000000000000000000 ) ) ;
#3224 = CARTESIAN_POINT ( 'NONE',  ( -6.988114217767819270, 21.16666666666666430, 26.07999730980490583 ) ) ;
#3225 = DIRECTION ( 'NONE',  ( 0.000000000000000000, 1.000000000000000000, 0.000000000000000000 ) ) ;
#3226 = CARTESIAN_POINT ( 'NONE',  ( -1.778240108872766143E-15, 47.49999999999999289, -32.49999999999999289 ) ) ;
#3227 = CARTESIAN_POINT ( 'NONE',  ( 20.08610463437158344, 72.70000000000001705, 27.64615127144129403 ) ) ;
#3228 = CARTESIAN_POINT ( 'NONE',  ( -20.75514604977248823, 10.82500000273118701, -28.56700777964554305 ) ) ;
#3229 = CARTESIAN_POINT ( 'NONE',  ( 7.236395654485760609, 5.024999997268825069, -22.27133577429736633 ) ) ;
#3230 = CYLINDRICAL_SURFACE ( 'NONE', #6705, 32.50000000000000000 ) ;
#3231 = CARTESIAN_POINT ( 'NONE',  ( 19.11951029504797006, 26.03086833240935860, 19.06425588902558133 ) ) ;
#3232 = CARTESIAN_POINT ( 'NONE',  ( -24.50000000000000000, 12.90000000000000036, -7.960532557706207157 ) ) ;
#3233 = CARTESIAN_POINT ( 'NONE',  ( -10.37757302488624411, 16.72500000273119269, -31.93888565452638417 ) ) ;
#3234 = CARTESIAN_POINT ( 'NONE',  ( -26.07999730980477437, 52.67708333333333570, 6.988114217768305103 ) ) ;
#3235 = ORIENTED_EDGE ( 'NONE', *, *, #181, .T. ) ;
#3236 = CARTESIAN_POINT ( 'NONE',  ( -33.58253175000000113, 55.12500000273119838, 0.000000000000000000 ) ) ;
#3237 = ORIENTED_EDGE ( 'NONE', *, *, #17210, .F. ) ;
#3238 = CARTESIAN_POINT ( 'NONE',  ( 15.01150461594643204, 27.61197916666666430, 26.00068869287340334 ) ) ;
#3239 = CARTESIAN_POINT ( 'NONE',  ( 28.02196122052045268, 28.33371500092397355, -7.468012846824774620 ) ) ;
#3240 = CARTESIAN_POINT ( 'NONE',  ( -10.37757302488624411, 6.725000002731185589, -31.93888565452638417 ) ) ;
#3241 = ORIENTED_EDGE ( 'NONE', *, *, #32764, .T. ) ;
#3242 = DIRECTION ( 'NONE',  ( -1.224646799147353454E-16, 1.000000000000000000, -0.000000000000000000 ) ) ;
#3243 = CARTESIAN_POINT ( 'NONE',  ( -33.58253175000000113, 27.47500000273118204, 10.91162601494193929 ) ) ;
#3244 = CARTESIAN_POINT ( 'NONE',  ( -10.04305231718579172, 34.10000000546236976, -30.90933677959248982 ) ) ;
#3245 = CARTESIAN_POINT ( 'NONE',  ( -9.270509831248421762, 72.29999999999999716, 12.75976212528060039 ) ) ;
#3246 = CARTESIAN_POINT ( 'NONE',  ( -32.50000000000000000, 54.60000000546237686, 10.55989012756946366 ) ) ;
#3247 = CARTESIAN_POINT ( 'NONE',  ( 0.000000000000000000, 80.00000000000001421, -32.50000000000000000 ) ) ;
#3248 = CARTESIAN_POINT ( 'NONE',  ( -33.58253175000000113, 45.27500000273116854, -10.91162601494193218 ) ) ;
#3249 = CARTESIAN_POINT ( 'NONE',  ( 6.277390505771533514E-15, 24.50000000000001421, 34.17252228774368916 ) ) ;
#3250 = CARTESIAN_POINT ( 'NONE',  ( -20.08610463437156923, 22.29999999999999716, 27.64615127144130113 ) ) ;
#3251 = CARTESIAN_POINT ( 'NONE',  ( -19.82091636218621389, 11.19999999999998863, 14.40073868116558842 ) ) ;
#3252 = CARTESIAN_POINT ( 'NONE',  ( 20.75514604977248467, 60.42500000273118133, -28.56700777964554305 ) ) ;
#3253 = CARTESIAN_POINT ( 'NONE',  ( -7.570916362186210335, 4.349999994537640191, -23.30088464923126779 ) ) ;
#3254 = CARTESIAN_POINT ( 'NONE',  ( 6.486482029760648627E-15, 55.87500000273118417, 35.31076352940722529 ) ) ;
#3255 = CARTESIAN_POINT ( 'NONE',  ( 1.507698388325705758E-15, 1.124999997268814722, -24.62258325217400312 ) ) ;
#3256 = CARTESIAN_POINT ( 'NONE',  ( -4.223320258572819786E-15, 9.499999999999992895, 24.50000000000000000 ) ) ;
#3257 = CARTESIAN_POINT ( 'NONE',  ( -33.58253175000000113, 7.025000002731188964, -10.91162601494193218 ) ) ;
#3258 = CARTESIAN_POINT ( 'NONE',  ( 26.09010956794232428, 42.08371500092398065, -6.950374756619718042 ) ) ;
#3259 = CARTESIAN_POINT ( 'NONE',  ( 23.11635443782376242, 16.99999999999997868, -3.820720850812610259 ) ) ;
#3260 = CARTESIAN_POINT ( 'NONE',  ( -30.22248186753587973, 52.00000000000002842, 12.55019540181404736 ) ) ;
#3261 = CARTESIAN_POINT ( 'NONE',  ( -27.16883889988623935, 27.32500000273117990, 19.73931689729374739 ) ) ;
#3262 = CARTESIAN_POINT ( 'NONE',  ( 10.04305231718579705, 64.60000000000000853, 30.90933677959248982 ) ) ;
#3263 = CARTESIAN_POINT ( 'NONE',  ( 11.54700538379251107, 96.00000000000002842, -19.99999999999999645 ) ) ;
#3264 = CARTESIAN_POINT ( 'NONE',  ( 3.880418787951140036, 14.44874571845315536, -24.49999999999999645 ) ) ;
#3265 = CARTESIAN_POINT ( 'NONE',  ( -15.04653450569338524, 55.39284749907604066, -25.98046417659831775 ) ) ;
#3266 = CARTESIAN_POINT ( 'NONE',  ( -26.29305231718578995, 50.70000000546236407, 19.10302069950538595 ) ) ;
#3267 = CARTESIAN_POINT ( 'NONE',  ( 10.04305231718579705, 48.60000000000000142, 30.90933677959248982 ) ) ;
#3268 = SHAPE_REPRESENTATION ( 'top barb fitting', ( #1376 ), #19430 ) ;
#3269 = CARTESIAN_POINT ( 'NONE',  ( 24.20753774853731244, 26.75260416666666430, -13.97622843553632599 ) ) ;
#3270 = ORIENTED_EDGE ( 'NONE', *, *, #13968, .F. ) ;
#3271 = CARTESIAN_POINT ( 'NONE',  ( 20.08610463437157279, 67.80000000546236549, -27.64615127144129758 ) ) ;
#3272 = CARTESIAN_POINT ( 'NONE',  ( 15.01150461594643204, 34.48697916666667140, 26.00068869287340334 ) ) ;
#3273 = CARTESIAN_POINT ( 'NONE',  ( 20.58269335310955839, 16.96161537386475260, 11.51052958701926698 ) ) ;
#3274 = ORIENTED_EDGE ( 'NONE', *, *, #19531, .T. ) ;
#3275 = CARTESIAN_POINT ( 'NONE',  ( 7.543491769121427382, 38.07329833425730925, -28.00173670424548433 ) ) ;
#3276 = CARTESIAN_POINT ( 'NONE',  ( -20.08610463437157989, 20.20000000546239249, -27.64615127144129758 ) ) ;
#3277 = EDGE_CURVE ( 'NONE', #5214, #19151, #20139, .T. ) ;
#3278 = CARTESIAN_POINT ( 'NONE',  ( -15.01150461594595775, 55.68489583333332860, 26.00068869287368756 ) ) ;
#3279 = CARTESIAN_POINT ( 'NONE',  ( -7.505752307972844761, 65.85416666666665719, 28.01184896238304134 ) ) ;
#3280 = CARTESIAN_POINT ( 'NONE',  ( 27.16883889988623935, 48.57500000273118701, -19.73931689729374384 ) ) ;
#3281 = CARTESIAN_POINT ( 'NONE',  ( 32.50000000000000000, 51.60000000546239107, -10.55989012756945833 ) ) ;
#3282 = CARTESIAN_POINT ( 'NONE',  ( 8.601468415847520532, 80.07500000273120122, 11.83890561707634781 ) ) ;
#3283 = CARTESIAN_POINT ( 'NONE',  ( -10.37757302488624411, 32.72500000273117848, -31.93888565452638417 ) ) ;
#3284 = CARTESIAN_POINT ( 'NONE',  ( 20.08610463437157279, 77.80000000546237970, -27.64615127144129758 ) ) ;
#3285 = CARTESIAN_POINT ( 'NONE',  ( 20.75514604977249178, 62.07500000273118701, 28.56700777964553950 ) ) ;
#3286 = CARTESIAN_POINT ( 'NONE',  ( 11.07021743829117710, 74.00000000000002842, 8.483650685288816717 ) ) ;
#3287 = EDGE_CURVE ( 'NONE', #11786, #24787, #21809, .T. ) ;
#3288 = CARTESIAN_POINT ( 'NONE',  ( -33.58253175000000113, 53.02500000273118985, -10.91162601494193041 ) ) ;
#3289 = EDGE_CURVE ( 'NONE', #15868, #29257, #7629, .T. ) ;
#3290 = CARTESIAN_POINT ( 'NONE',  ( 32.50000000000000000, 41.10000000000001563, -10.55989012756945833 ) ) ;
#3291 = CARTESIAN_POINT ( 'NONE',  ( 18.94512977948576093, 4.824999997268819563, -13.76444248337722875 ) ) ;
#3292 = CARTESIAN_POINT ( 'NONE',  ( -10.37757302488624411, 6.975000002731185589, -31.93888565452638417 ) ) ;
#3293 = CARTESIAN_POINT ( 'NONE',  ( 26.29305231718578995, 35.70000000546236407, -19.10302069950538240 ) ) ;
#3294 = CARTESIAN_POINT ( 'NONE',  ( -13.91746824999999532, 75.27500000273121827, -4.522059556121115875 ) ) ;
#3295 = CARTESIAN_POINT ( 'NONE',  ( 10.37757302488624767, 71.97500000273119269, 31.93888565452638417 ) ) ;
#3296 = CARTESIAN_POINT ( 'NONE',  ( 7.570916362186207671, 3.349999994537639303, 23.30088464923126779 ) ) ;
#3297 = EDGE_CURVE ( 'NONE', #33362, #1345, #15710, .T. ) ;
#3298 = CARTESIAN_POINT ( 'NONE',  ( 20.75514604977249178, 70.07500000273120122, 28.56700777964553950 ) ) ;
#3299 = ORIENTED_EDGE ( 'NONE', *, *, #21276, .F. ) ;
#3300 = CARTESIAN_POINT ( 'NONE',  ( 14.47279130897151589, 18.82499999726881157, 19.92008829642072953 ) ) ;
#3301 = CARTESIAN_POINT ( 'NONE',  ( -24.18731323226248264, 13.29465250092397532, -14.01125832528284931 ) ) ;
#3302 = CARTESIAN_POINT ( 'NONE',  ( -7.579748464070167083E-14, 10.49999999999999112, -24.50000000000000000 ) ) ;
#3303 = CARTESIAN_POINT ( 'NONE',  ( -10.37757302488624411, 44.72500000273120691, -31.93888565452638417 ) ) ;
#3304 = CARTESIAN_POINT ( 'NONE',  ( -33.58253175000000113, 13.47500000273118914, 10.91162601494193929 ) ) ;
#3305 = CARTESIAN_POINT ( 'NONE',  ( -27.16883889988623935, 61.57500000273117990, 19.73931689729374739 ) ) ;
#3306 = CARTESIAN_POINT ( 'NONE',  ( 2.584737979205442066E-13, 48.52343749999999289, 27.95245687107223276 ) ) ;
#3307 = PRODUCT_DEFINITION_FORMATION_WITH_SPECIFIED_SOURCE ( 'ANY', '', #9557, .NOT_KNOWN. ) ;
#3308 = CARTESIAN_POINT ( 'NONE',  ( -15.04653450569291984, 26.18527750092397710, 25.98046417659859486 ) ) ;
#3309 = CARTESIAN_POINT ( 'NONE',  ( -26.02091320914878025, 31.04388916574268364, -14.97647472619899389 ) ) ;
#3310 = CARTESIAN_POINT ( 'NONE',  ( 32.50000000000000000, 71.60000000546240528, -10.55989012756945833 ) ) ;
#3311 = CARTESIAN_POINT ( 'NONE',  ( 13.91746824999999887, 75.87500000273116996, -1.704398294459741270E-15 ) ) ;
#3312 = CARTESIAN_POINT ( 'NONE',  ( -20.75514604977248823, 36.82500000273117990, -28.56700777964554305 ) ) ;
#3313 = CARTESIAN_POINT ( 'NONE',  ( 7.025853678916867295, 43.50482666574268364, 26.06988505166722803 ) ) ;
#3314 = CARTESIAN_POINT ( 'NONE',  ( -14.47279130897152122, 17.92499999726880588, 19.92008829642072243 ) ) ;
#3315 = CARTESIAN_POINT ( 'NONE',  ( -1.778240108872766143E-15, 59.50000000000000711, -32.49999999999999289 ) ) ;
#3316 = EDGE_LOOP ( 'NONE', ( #474, #19189, #20666, #19232 ) ) ;
#3317 = CARTESIAN_POINT ( 'NONE',  ( -27.16883889988624290, 47.17500000273118843, -19.73931689729374028 ) ) ;
#3318 = CARTESIAN_POINT ( 'NONE',  ( 1.555960095263670572E-15, 12.50000000000000355, -24.50000000000000000 ) ) ;
#3319 = CARTESIAN_POINT ( 'NONE',  ( -7.025853678916393008, 50.10454833425731636, 26.06988505166735592 ) ) ;
#3320 = CARTESIAN_POINT ( 'NONE',  ( -33.58253175000000113, 67.47500000273117848, 10.91162601494193929 ) ) ;
#3321 = ORIENTED_EDGE ( 'NONE', *, *, #2853, .F. ) ;
#3322 = CARTESIAN_POINT ( 'NONE',  ( -10.37757302488624411, 16.72500000273117848, -31.93888565452638417 ) ) ;
#3323 = CARTESIAN_POINT ( 'NONE',  ( -20.50609665440969209, 21.45312499999999645, 20.50609665441005092 ) ) ;
#3324 = ORIENTED_EDGE ( 'NONE', *, *, #2535, .F. ) ;
#3325 = CARTESIAN_POINT ( 'NONE',  ( -5.147494310547423346, 48.94874572391553613, 32.50000000000000000 ) ) ;
#3326 = CARTESIAN_POINT ( 'NONE',  ( -20.75514604977248112, 57.42500000273118843, 28.56700777964554661 ) ) ;
#3327 = CARTESIAN_POINT ( 'NONE',  ( -28.01184896238290278, 56.11458333333332860, 7.505752307973363457 ) ) ;
#3328 = CARTESIAN_POINT ( 'NONE',  ( -2.092463501923844636E-15, 18.00000000546237189, -34.17252228774368916 ) ) ;
#3329 = CARTESIAN_POINT ( 'NONE',  ( 4.445600272181915325E-13, 14.00000000546237544, -32.50000000000000000 ) ) ;
#3330 = CARTESIAN_POINT ( 'NONE',  ( 23.41746824999999887, 11.02499999726882152, 7.608796670333735079 ) ) ;
#3331 = CARTESIAN_POINT ( 'NONE',  ( -27.16883889988624290, 23.17500000273120619, -19.73931689729374028 ) ) ;
#3332 = CARTESIAN_POINT ( 'NONE',  ( -27.95245687107223986, 17.00743083240935860, 0.04044903255043252877 ) ) ;
#3333 = DIRECTION ( 'NONE',  ( 0.000000000000000000, 0.000000000000000000, 1.000000000000000000 ) ) ;
#3334 = CARTESIAN_POINT ( 'NONE',  ( -5.147494310547430452, 28.05125428700921475, -32.49999999999999289 ) ) ;
#3335 = CARTESIAN_POINT ( 'NONE',  ( 32.50000000000000000, 8.999999999999994671, -3.980102097228898626E-15 ) ) ;
#3336 = ORIENTED_EDGE ( 'NONE', *, *, #20704, .F. ) ;
#3337 = CARTESIAN_POINT ( 'NONE',  ( 14.47279130897151589, 2.824999997268819119, 19.92008829642072953 ) ) ;
#3338 = CARTESIAN_POINT ( 'NONE',  ( -11.25946833292375793, 77.07500000273121543, 8.180482586598737171 ) ) ;
#3339 = CARTESIAN_POINT ( 'NONE',  ( -6.988114217768288228, 29.47395833333332860, -26.07999730980477437 ) ) ;
#3340 = ADVANCED_FACE ( 'NONE', ( #23256 ), #2485, .T. ) ;
#3341 = CARTESIAN_POINT ( 'NONE',  ( -33.58253175000000113, 23.22500000273117138, 10.91162601494193929 ) ) ;
#3342 = PRODUCT_DEFINITION_SHAPE ( 'NONE', 'NONE',  #16263 ) ;
#3343 = CARTESIAN_POINT ( 'NONE',  ( -10.37757302488624411, 70.72500000273117848, -31.93888565452638417 ) ) ;
#3344 = CARTESIAN_POINT ( 'NONE',  ( -2.162160676586881955E-15, 28.87500000273119838, -35.31076352940723240 ) ) ;
#3345 = CARTESIAN_POINT ( 'NONE',  ( -33.58253175000000113, 19.47500000273117493, 10.91162601494193929 ) ) ;
#3346 = CARTESIAN_POINT ( 'NONE',  ( 10.37757302488624767, 13.97500000273119092, 31.93888565452638417 ) ) ;
#3347 = CARTESIAN_POINT ( 'NONE',  ( 19.11951029504763611, 55.54725666759064495, -19.06425588902591173 ) ) ;
#3348 = CARTESIAN_POINT ( 'NONE',  ( 27.16883889988623935, 72.32500000273117280, -19.73931689729374384 ) ) ;
#3349 = CARTESIAN_POINT ( 'NONE',  ( 0.000000000000000000, -22.99999999999999289, 0.000000000000000000 ) ) ;
#3350 = CARTESIAN_POINT ( 'NONE',  ( -13.91746824999999532, 77.27500000273118985, -4.522059556121115875 ) ) ;
#3351 = CARTESIAN_POINT ( 'NONE',  ( 26.29305231718578995, 53.20000000000000995, -19.10302069950538240 ) ) ;
#3352 = CARTESIAN_POINT ( 'NONE',  ( 0.000000000000000000, -22.99999999999999289, 0.000000000000000000 ) ) ;
#3353 = CARTESIAN_POINT ( 'NONE',  ( 10.37757302488624767, 55.72500000273117138, 31.93888565452638417 ) ) ;
#3354 = CARTESIAN_POINT ( 'NONE',  ( -23.41746824999999887, 14.12499999726882294, -2.867812753649727150E-15 ) ) ;
#3355 = ORIENTED_EDGE ( 'NONE', *, *, #12398, .F. ) ;
#3356 = CARTESIAN_POINT ( 'NONE',  ( 10.37757302488624767, 69.97500000273119269, 31.93888565452638417 ) ) ;
#3357 = CARTESIAN_POINT ( 'NONE',  ( 5.779280353836490358E-15, 16.50000000000000000, 32.49999999999999289 ) ) ;
#3358 = CARTESIAN_POINT ( 'NONE',  ( -14.47279130897151589, 9.324999997268816898, -19.92008829642072598 ) ) ;
#3359 = CARTESIAN_POINT ( 'NONE',  ( -26.09010956794232428, 19.73996500092397355, 6.950374756619732253 ) ) ;
#3360 = ORIENTED_EDGE ( 'NONE', *, *, #16600, .F. ) ;
#3361 = CARTESIAN_POINT ( 'NONE',  ( 33.58253175000000113, 36.12500000273118417, -4.112674001490185761E-15 ) ) ;
#3362 = DIRECTION ( 'NONE',  ( -0.000000000000000000, -1.000000000000000000, -0.000000000000000000 ) ) ;
#3363 = ORIENTED_EDGE ( 'NONE', *, *, #7756, .F. ) ;
#3364 = CARTESIAN_POINT ( 'NONE',  ( -7.505752307972844761, 52.10416666666666430, 28.01184896238304134 ) ) ;
#3365 = CARTESIAN_POINT ( 'NONE',  ( 5.147494310547426899, 5.448745718453162468, -32.50000000000000000 ) ) ;
#3366 = CARTESIAN_POINT ( 'NONE',  ( 0.000000000000000000, 82.00000000000001421, 0.000000000000000000 ) ) ;
#3367 = CARTESIAN_POINT ( 'NONE',  ( 10.37757302488624767, 75.72500000273119269, 31.93888565452638417 ) ) ;
#3368 = CARTESIAN_POINT ( 'NONE',  ( -28.01184896238304134, 22.02604166666666430, -7.505752307972844761 ) ) ;
#3369 = CARTESIAN_POINT ( 'NONE',  ( 24.50000000000000355, 8.100000000000006750, -7.960532557706203605 ) ) ;
#3370 = CARTESIAN_POINT ( 'NONE',  ( -27.16883889988623935, 11.57500000273120655, 19.73931689729374739 ) ) ;
#3371 = CARTESIAN_POINT ( 'NONE',  ( -20.75514604977248112, 13.42500000273119198, 28.56700777964554661 ) ) ;
#3372 = CARTESIAN_POINT ( 'NONE',  ( -13.91746824999999532, 80.77500000273118985, -4.522059556121115875 ) ) ;
#3373 = CARTESIAN_POINT ( 'NONE',  ( 15.00000000000000000, 77.25000000546239676, -1.836970198721029589E-15 ) ) ;
#3374 = CARTESIAN_POINT ( 'NONE',  ( -20.47846945139866648, 47.51524333240936215, 20.53372385742108008 ) ) ;
#3375 = VECTOR ( 'NONE', #16248, 1000.000000000000114 ) ;
#3376 = CARTESIAN_POINT ( 'NONE',  ( 13.91746825000000065, 72.27500000273118985, 4.522059556121114987 ) ) ;
#3377 = CARTESIAN_POINT ( 'NONE',  ( -26.00068869287340334, 45.65885416666666430, 15.01150461594643559 ) ) ;
#3378 = CARTESIAN_POINT ( 'NONE',  ( -19.82091636218621389, 16.94999999453764161, 14.40073868116558842 ) ) ;
#3379 = CARTESIAN_POINT ( 'NONE',  ( 32.50000000000000000, 71.09999999999999432, -10.55989012756945833 ) ) ;
#3380 = CARTESIAN_POINT ( 'NONE',  ( 0.04044903255044120238, 57.39805583240935505, 27.95245687107223276 ) ) ;
#3381 = ADVANCED_FACE ( 'NONE', ( #15366 ), #7797, .T. ) ;
#3382 = CARTESIAN_POINT ( 'NONE',  ( 10.37757302488624056, 44.52500000273118275, -31.93888565452638417 ) ) ;
#3383 = CARTESIAN_POINT ( 'NONE',  ( -4.300734207923759378, 78.47500000273116427, -13.23629886949340495 ) ) ;
#3384 = CARTESIAN_POINT ( 'NONE',  ( -20.75514604977248823, 47.07500000273117990, -28.56700777964554305 ) ) ;
#3385 = CARTESIAN_POINT ( 'NONE',  ( 33.58253175000000113, 32.37500000273119127, -4.112674001490185761E-15 ) ) ;
#3386 = CARTESIAN_POINT ( 'NONE',  ( 15.62859546567362656, 16.99999999999999645, 17.78191404720239888 ) ) ;
#3387 = EDGE_CURVE ( 'NONE', #15614, #12770, #32314, .T. ) ;
#3388 = CARTESIAN_POINT ( 'NONE',  ( 13.97622843553633842, 24.17447916666666075, 24.20753774853730889 ) ) ;
#3389 = CARTESIAN_POINT ( 'NONE',  ( 5.779280353836490358E-15, 18.50000000000000000, 32.49999999999999289 ) ) ;
#3390 = CARTESIAN_POINT ( 'NONE',  ( 0.000000000000000000, 70.00000000000000000, -15.00000000000000000 ) ) ;
#3391 = CARTESIAN_POINT ( 'NONE',  ( -20.08610463437156923, 76.30000000000001137, 27.64615127144130113 ) ) ;
#3392 = CARTESIAN_POINT ( 'NONE',  ( 33.58253175000000113, 10.22500000273118914, -10.91162601494193751 ) ) ;
#3393 = CARTESIAN_POINT ( 'NONE',  ( 18.94512977948575738, 4.424999997268807661, 13.76444248337723408 ) ) ;
#3394 = DIRECTION ( 'NONE',  ( -0.000000000000000000, 1.000000000000000000, -0.000000000000000000 ) ) ;
#3395 = CARTESIAN_POINT ( 'NONE',  ( -19.11951029504797006, 24.31211833240934794, -19.06425588902558133 ) ) ;
#3396 = CARTESIAN_POINT ( 'NONE',  ( -2.375766604868045029, 75.80125428700921475, -14.99999999999999822 ) ) ;
#3397 = CARTESIAN_POINT ( 'NONE',  ( 33.58253175000000113, 20.22500000273117848, -10.91162601494193574 ) ) ;
#3398 = CARTESIAN_POINT ( 'NONE',  ( 7.236395654485755280, 8.724999997268806595, 22.27133577429736988 ) ) ;
#3399 = CARTESIAN_POINT ( 'NONE',  ( 6.988114217767829928, 57.26041666666666430, -26.07999730980489872 ) ) ;
#3400 = ORIENTED_EDGE ( 'NONE', *, *, #24650, .F. ) ;
#3401 = CARTESIAN_POINT ( 'NONE',  ( 33.58253175000000823, 56.02500000273117564, 10.91162601494192863 ) ) ;
#3402 = ORIENTED_EDGE ( 'NONE', *, *, #17508, .F. ) ;
#3403 = CARTESIAN_POINT ( 'NONE',  ( 15.01150461594596308, 23.02864583333332149, -26.00068869287367335 ) ) ;
#3404 = CARTESIAN_POINT ( 'NONE',  ( -28.02196122052045268, 19.73996500092397355, 7.468012846824790607 ) ) ;
#3405 = CARTESIAN_POINT ( 'NONE',  ( 0.000000000000000000, 52.00000000000000711, 0.000000000000000000 ) ) ;
#3406 = CARTESIAN_POINT ( 'NONE',  ( 14.47279130897151589, 6.324999997268824892, 19.92008829642072953 ) ) ;
#3407 = CARTESIAN_POINT ( 'NONE',  ( 33.58253175000000113, 28.37500000273118772, -4.112674001490185761E-15 ) ) ;
#3408 = CARTESIAN_POINT ( 'NONE',  ( -32.50000000000000000, 28.50000000546237899, 0.000000000000000000 ) ) ;
#3409 = CARTESIAN_POINT ( 'NONE',  ( -26.29305231718579350, 77.80000000000001137, -19.10302069950537884 ) ) ;
#3410 = CARTESIAN_POINT ( 'NONE',  ( 5.147494310547426899, 33.94874572391552192, -32.50000000000000000 ) ) ;
#3411 = CYLINDRICAL_SURFACE ( 'NONE', #33493, 32.50000000000000000 ) ;
#3412 = CARTESIAN_POINT ( 'NONE',  ( -10.37757302488624411, 40.97500000273118559, -31.93888565452638417 ) ) ;
#3413 = CARTESIAN_POINT ( 'NONE',  ( -2.092463501923844636E-15, 21.49999999999998934, -34.17252228774368916 ) ) ;
#3414 = CARTESIAN_POINT ( 'NONE',  ( -26.29305231718579350, 23.79999999999998650, -19.10302069950537884 ) ) ;
#3415 = CARTESIAN_POINT ( 'NONE',  ( 7.570916362186207671, 9.599999999999997868, 23.30088464923126779 ) ) ;
#3416 = CARTESIAN_POINT ( 'NONE',  ( 33.58253175000000113, 62.22500000273119269, -10.91162601494193751 ) ) ;
#3417 = CARTESIAN_POINT ( 'NONE',  ( -20.75514604977248823, 57.07500000273117990, -28.56700777964554305 ) ) ;
#3418 = CARTESIAN_POINT ( 'NONE',  ( 18.94512977948575738, 10.42499999726881299, 13.76444248337723408 ) ) ;
#3419 = CARTESIAN_POINT ( 'NONE',  ( 24.50000000000000000, 4.099999999999986322, -7.960532557706203605 ) ) ;
#3420 = CARTESIAN_POINT ( 'NONE',  ( -10.37757302488624411, 8.725000002731187365, -31.93888565452638417 ) ) ;
#3421 = ADVANCED_FACE ( 'NONE', ( #16873 ), #22191, .F. ) ;
#3422 = EDGE_CURVE ( 'NONE', #4339, #20029, #29557, .T. ) ;
#3423 = CARTESIAN_POINT ( 'NONE',  ( -26.09010956794232428, 43.80246500092398776, 6.950374756619732253 ) ) ;
#3424 = CARTESIAN_POINT ( 'NONE',  ( 31.32135535759086054, 66.99999999999997158, -9.352374566761925578 ) ) ;
#3425 = CARTESIAN_POINT ( 'NONE',  ( -1.778240108872766143E-15, 19.50000000000000000, -32.49999999999999289 ) ) ;
#3426 = CARTESIAN_POINT ( 'NONE',  ( 27.16883889988623935, 30.32500000273117990, -19.73931689729374384 ) ) ;
#3427 = CARTESIAN_POINT ( 'NONE',  ( 10.04305231718579705, 56.59999999999999432, 30.90933677959248982 ) ) ;
#3428 = CARTESIAN_POINT ( 'NONE',  ( 26.29305231718579350, 61.30000000546238681, 19.10302069950537529 ) ) ;
#3429 = CARTESIAN_POINT ( 'NONE',  ( -5.147494310547430452, 30.05125428700921475, -32.49999999999999289 ) ) ;
#3430 = CARTESIAN_POINT ( 'NONE',  ( 30.02300923189239867, 59.97618083240934794, -0.04044903255044467877 ) ) ;
#3431 = CARTESIAN_POINT ( 'NONE',  ( -32.50000000000000000, 50.50000000546238255, 0.000000000000000000 ) ) ;
#3432 = FACE_OUTER_BOUND ( 'NONE', #27371, .T. ) ;
#3433 = CARTESIAN_POINT ( 'NONE',  ( -3.880418787951174675, 16.55125428154684997, -24.49999999999998579 ) ) ;
#3434 = AXIS2_PLACEMENT_3D ( 'NONE', #11819, #22295, #32740 ) ;
#3435 = CARTESIAN_POINT ( 'NONE',  ( 24.20753774853731244, 23.31510416666666430, -13.97622843553632599 ) ) ;
#3436 = ORIENTED_EDGE ( 'NONE', *, *, #13366, .T. ) ;
#3437 = AXIS2_PLACEMENT_3D ( 'NONE', #6769, #30611, #7107 ) ;
#3438 = CARTESIAN_POINT ( 'NONE',  ( 10.37757302488624056, 74.52500000273120406, -31.93888565452638417 ) ) ;
#3439 = CARTESIAN_POINT ( 'NONE',  ( 15.01150461594643204, 27.61197916666666430, 26.00068869287340334 ) ) ;
#3440 = DIRECTION ( 'NONE',  ( 1.000000000000000000, 0.000000000000000000, 1.224646799147352714E-16 ) ) ;
#3441 = ORIENTED_EDGE ( 'NONE', *, *, #3192, .T. ) ;
#3442 = CARTESIAN_POINT ( 'NONE',  ( -30.02300923189239867, 47.38319416759065206, -0.04044903254991731589 ) ) ;
#3443 = CARTESIAN_POINT ( 'NONE',  ( -32.50000000000000000, 14.50000000546237899, 0.000000000000000000 ) ) ;
#3444 = CARTESIAN_POINT ( 'NONE',  ( 26.00068869287340334, 54.25260416666666430, -15.01150461594642316 ) ) ;
#3445 = CARTESIAN_POINT ( 'NONE',  ( -20.08610463437156923, 36.29999999999998295, 27.64615127144130113 ) ) ;
#3446 = CARTESIAN_POINT ( 'NONE',  ( 20.75514604977248467, 48.67500000273117422, -28.56700777964554305 ) ) ;
#3447 = CARTESIAN_POINT ( 'NONE',  ( -10.04305231718579172, 52.10000000546239107, -30.90933677959248982 ) ) ;
#3448 = DIRECTION ( 'NONE',  ( 1.000000000000000000, 0.000000000000000000, 0.000000000000000000 ) ) ;
#3449 = CARTESIAN_POINT ( 'NONE',  ( -27.16883889988623935, 37.32500000273120122, 19.73931689729374739 ) ) ;
#3450 = DIRECTION ( 'NONE',  ( 1.224646799147353454E-16, -1.000000000000000000, 0.000000000000000000 ) ) ;
#3451 = CARTESIAN_POINT ( 'NONE',  ( -2.162160676586881955E-15, 62.87500000273120548, -35.31076352940723240 ) ) ;
#3452 = CARTESIAN_POINT ( 'NONE',  ( -20.08610463437156923, 42.30000000000000426, 27.64615127144130113 ) ) ;
#3453 = CARTESIAN_POINT ( 'NONE',  ( -18.94512977948575738, 9.424999997268812990, -13.76444248337723231 ) ) ;
#3454 = CARTESIAN_POINT ( 'NONE',  ( 27.16883889988623935, 6.575000002731201221, -19.73931689729374384 ) ) ;
#3455 = AXIS2_PLACEMENT_3D ( 'NONE', #29112, #7846, #8183 ) ;
#3456 = CYLINDRICAL_SURFACE ( 'NONE', #17855, 32.50000000000000000 ) ;
#3457 = CARTESIAN_POINT ( 'NONE',  ( 2.688165632520823219E-15, 71.87500000273121259, 14.63369212191046387 ) ) ;
#3458 = CARTESIAN_POINT ( 'NONE',  ( -20.75514604977248112, 75.67500000273119554, 28.56700777964554661 ) ) ;
#3459 = DIRECTION ( 'NONE',  ( 0.000000000000000000, 0.000000000000000000, -1.000000000000000000 ) ) ;
#3460 = AXIS2_PLACEMENT_3D ( 'NONE', #4843, #28357, #7418 ) ;
#3461 = CARTESIAN_POINT ( 'NONE',  ( -10.37757302488623701, 67.77500000273118985, 31.93888565452638417 ) ) ;
#3462 = VERTEX_POINT ( 'NONE', #16708 ) ;
#3463 = CARTESIAN_POINT ( 'NONE',  ( -24.50000000000000355, 4.649999994537640902, -7.960532557706207157 ) ) ;
#3464 = CARTESIAN_POINT ( 'NONE',  ( 6.950374756619721595, 15.44309000092397355, 26.09010956794232428 ) ) ;
#3465 = DIRECTION ( 'NONE',  ( -1.000000000000000000, 0.000000000000000000, 0.000000000000000000 ) ) ;
#3466 = CARTESIAN_POINT ( 'NONE',  ( 20.75514604977249178, 49.82500000273117990, 28.56700777964553950 ) ) ;
#3467 = CARTESIAN_POINT ( 'NONE',  ( -10.37757302488623701, 11.77500000273117031, 31.93888565452638417 ) ) ;
#3468 = CARTESIAN_POINT ( 'NONE',  ( 27.16883889988623935, 62.57500000273117990, -19.73931689729374384 ) ) ;
#3469 = CARTESIAN_POINT ( 'NONE',  ( -24.20753774853730889, 49.09635416666666430, 13.97622843553634020 ) ) ;
#3470 = CARTESIAN_POINT ( 'NONE',  ( -20.53372385742071771, 40.07850666759064495, 20.47846945139902530 ) ) ;
#3471 = CARTESIAN_POINT ( 'NONE',  ( 7.468012846824281681, 31.76003499907602290, -28.02196122052058058 ) ) ;
#3472 = CARTESIAN_POINT ( 'NONE',  ( 20.08610463437157279, 67.80000000546236549, -27.64615127144129758 ) ) ;
#3473 = CARTESIAN_POINT ( 'NONE',  ( -13.91746824999999887, 76.87500000273116996, 0.000000000000000000 ) ) ;
#3474 = CARTESIAN_POINT ( 'NONE',  ( 14.01125832528330051, 57.11159749907603356, 24.18731323226221974 ) ) ;
#3475 = CARTESIAN_POINT ( 'NONE',  ( 18.94512977948575738, 16.42499999726882010, 13.76444248337723408 ) ) ;
#3476 = CARTESIAN_POINT ( 'NONE',  ( 0.000000000000000000, -10.99999999999999645, 0.000000000000000000 ) ) ;
#3477 = ORIENTED_EDGE ( 'NONE', *, *, #17444, .F. ) ;
#3478 = CARTESIAN_POINT ( 'NONE',  ( 20.75514604977248467, 50.67500000273117422, -28.56700777964554305 ) ) ;
#3479 = DIRECTION ( 'NONE',  ( 0.000000000000000000, -1.000000000000000000, 0.000000000000000000 ) ) ;
#3480 = CARTESIAN_POINT ( 'NONE',  ( 19.11951029504763611, 55.54725666759064495, -19.06425588902591173 ) ) ;
#3481 = CARTESIAN_POINT ( 'NONE',  ( 27.16883889988623935, 68.57500000273120122, -19.73931689729374384 ) ) ;
#3482 = ORIENTED_EDGE ( 'NONE', *, *, #21089, .T. ) ;
#3483 = CARTESIAN_POINT ( 'NONE',  ( 20.75514604977249178, 17.82500000273120122, 28.56700777964553950 ) ) ;
#3484 = AXIS2_PLACEMENT_3D ( 'NONE', #33078, #25029, #2030 ) ;
#3485 = ADVANCED_FACE ( 'NONE', ( #18956 ), #29724, .T. ) ;
#3486 = CARTESIAN_POINT ( 'NONE',  ( 26.00068869287340334, 26.75260416666666430, -15.01150461594642316 ) ) ;
#3487 = ORIENTED_EDGE ( 'NONE', *, *, #23060, .T. ) ;
#3488 = CARTESIAN_POINT ( 'NONE',  ( -19.82091636218621389, 2.949999994537627401, 14.40073868116558842 ) ) ;
#3489 = CARTESIAN_POINT ( 'NONE',  ( 6.486482029760649416E-15, 53.62500000273119838, 35.31076352940723240 ) ) ;
#3490 = CARTESIAN_POINT ( 'NONE',  ( 30.02300923189239512, 54.53906249999998579, -2.619432448724977703E-13 ) ) ;
#3491 = CARTESIAN_POINT ( 'NONE',  ( -32.50000000000000000, 14.40000000546236691, -10.55989012756945478 ) ) ;
#3492 = CARTESIAN_POINT ( 'NONE',  ( 0.000000000000000000, 52.00000000000000711, 0.000000000000000000 ) ) ;
#3493 = CARTESIAN_POINT ( 'NONE',  ( -23.41746824999999887, 16.02499999726881086, -7.608796670333730638 ) ) ;
#3494 = CARTESIAN_POINT ( 'NONE',  ( -10.37757302488624411, 20.97500000273119625, -31.93888565452638417 ) ) ;
#3495 =( NAMED_UNIT ( * ) PLANE_ANGLE_UNIT ( ) SI_UNIT ( $, .RADIAN. ) );
#3496 = CARTESIAN_POINT ( 'NONE',  ( 19.11951029504797006, 15.71836833240935327, 19.06425588902558133 ) ) ;
#3497 = CARTESIAN_POINT ( 'NONE',  ( 26.29305231718579350, 65.30000000546236549, 19.10302069950537529 ) ) ;
#3498 = CARTESIAN_POINT ( 'NONE',  ( -20.08610463437157989, 33.70000000000001705, -27.64615127144129758 ) ) ;
#3499 = CARTESIAN_POINT ( 'NONE',  ( 20.08610463437158344, 12.70000000000000639, 27.64615127144129403 ) ) ;
#3500 = ORIENTED_EDGE ( 'NONE', *, *, #3387, .F. ) ;
#3501 = CARTESIAN_POINT ( 'NONE',  ( -14.47279130897151589, 3.824999997268816454, -19.92008829642072598 ) ) ;
#3502 = CARTESIAN_POINT ( 'NONE',  ( -4.300734207923759378, 76.47500000273119269, -13.23629886949340495 ) ) ;
#3503 = CARTESIAN_POINT ( 'NONE',  ( -24.20753774853730889, 45.65885416666666430, 13.97622843553633842 ) ) ;
#3504 = CARTESIAN_POINT ( 'NONE',  ( -33.58253175000000113, 27.02500000273119696, -10.91162601494193218 ) ) ;
#3505 = CARTESIAN_POINT ( 'NONE',  ( -10.37757302488623701, 67.52500000273118985, 31.93888565452638417 ) ) ;
#3506 = CARTESIAN_POINT ( 'NONE',  ( 33.58253175000000113, 30.37500000273117706, -4.112674001490185761E-15 ) ) ;
#3507 = CARTESIAN_POINT ( 'NONE',  ( -2.162160676586881955E-15, 18.87500000273119483, -35.31076352940723240 ) ) ;
#3508 = CARTESIAN_POINT ( 'NONE',  ( -2.162160676586882350E-15, 6.875000002731194826, -35.31076352940722529 ) ) ;
#3509 = CARTESIAN_POINT ( 'NONE',  ( 30.02300923189239867, 11.28944416759064140, 0.04044903254992252006 ) ) ;
#3510 = CARTESIAN_POINT ( 'NONE',  ( 20.75514604977249178, 69.82500000273118701, 28.56700777964553950 ) ) ;
#3511 = CARTESIAN_POINT ( 'NONE',  ( -26.00068869287368756, 56.54427083333332149, -15.01150461594595775 ) ) ;
#3512 = DIRECTION ( 'NONE',  ( -0.000000000000000000, -1.000000000000000000, -0.000000000000000000 ) ) ;
#3513 = CARTESIAN_POINT ( 'NONE',  ( 13.91746824999999887, 78.37500000273116996, -1.704398294459741270E-15 ) ) ;
#3514 = CARTESIAN_POINT ( 'NONE',  ( -32.50000000000000000, 50.00000000000000000, 0.000000000000000000 ) ) ;
#3515 = CARTESIAN_POINT ( 'NONE',  ( -12.13525491562420910, 72.45000000546237118, 8.816778784387098611 ) ) ;
#3516 = CARTESIAN_POINT ( 'NONE',  ( 10.37757302488624056, 58.52500000273119696, -31.93888565452638417 ) ) ;
#3517 = CARTESIAN_POINT ( 'NONE',  ( 18.94512977948575738, 16.92499999726882010, 13.76444248337723408 ) ) ;
#3518 = VERTEX_POINT ( 'NONE', #1229 ) ;
#3519 = CARTESIAN_POINT ( 'NONE',  ( 20.75514604977249178, 70.07500000273120122, 28.56700777964553950 ) ) ;
#3520 = CARTESIAN_POINT ( 'NONE',  ( -32.50000000000000000, 16.00000000000001421, 0.000000000000000000 ) ) ;
#3521 = CARTESIAN_POINT ( 'NONE',  ( 18.94512977948576093, 4.824999997268819563, -13.76444248337722875 ) ) ;
#3522 = CARTESIAN_POINT ( 'NONE',  ( 27.95245687107223986, 21.60194416759064495, 0.04044903254993640479 ) ) ;
#3523 = ORIENTED_EDGE ( 'NONE', *, *, #21121, .F. ) ;
#3524 = CARTESIAN_POINT ( 'NONE',  ( 10.37757302488624767, 35.72500000273119980, 31.93888565452638417 ) ) ;
#3525 = CARTESIAN_POINT ( 'NONE',  ( 0.000000000000000000, 52.00000000000000711, 0.000000000000000000 ) ) ;
#3526 = ORIENTED_EDGE ( 'NONE', *, *, #33800, .F. ) ;
#3527 = CARTESIAN_POINT ( 'NONE',  ( -15.01150461594642138, 53.39322916666665009, -26.00068869287340334 ) ) ;
#3528 = CARTESIAN_POINT ( 'NONE',  ( 27.16883889988624290, 62.17500000273118133, 19.73931689729373673 ) ) ;
#3529 = CARTESIAN_POINT ( 'NONE',  ( 32.50000000000000711, 58.90000000000000568, 10.55989012756945122 ) ) ;
#3530 = CARTESIAN_POINT ( 'NONE',  ( -33.58253175000000113, 77.12500000273119838, 0.000000000000000000 ) ) ;
#3531 = CARTESIAN_POINT ( 'NONE',  ( -30.02300923189239512, 32.19531250000000000, 2.654126918244515359E-13 ) ) ;
#3532 = CARTESIAN_POINT ( 'NONE',  ( -15.14183272437241889, 4.699999999999995737, -20.84094480462497856 ) ) ;
#3533 = CARTESIAN_POINT ( 'NONE',  ( -33.58253175000000113, 7.375000002731169069, 0.000000000000000000 ) ) ;
#3534 = CARTESIAN_POINT ( 'NONE',  ( 20.75514604977249178, 15.82500000273117102, 28.56700777964553950 ) ) ;
#3535 = CARTESIAN_POINT ( 'NONE',  ( 13.91746824999999887, 73.87500000273116996, -1.704398294459741270E-15 ) ) ;
#3536 = CARTESIAN_POINT ( 'NONE',  ( 0.000000000000000000, 0.000000000000000000, 24.50000000000000000 ) ) ;
#3537 = CARTESIAN_POINT ( 'NONE',  ( -25.98046417659831420, 44.22097249907603356, 15.04653450569339945 ) ) ;
#3538 = CARTESIAN_POINT ( 'NONE',  ( 15.00000000000000000, 79.10000000000000853, -4.873795443493596835 ) ) ;
#3539 = CARTESIAN_POINT ( 'NONE',  ( -15.01150461594595775, 52.24739583333332860, 26.00068869287368756 ) ) ;
#3540 = CARTESIAN_POINT ( 'NONE',  ( 26.29305231718579350, 53.30000000546237970, 19.10302069950537529 ) ) ;
#3541 = CARTESIAN_POINT ( 'NONE',  ( -1.778240108872766143E-15, 38.00000000546237544, -32.49999999999999289 ) ) ;
#3542 = CARTESIAN_POINT ( 'NONE',  ( 26.09010956794244507, 66.99440999907601224, 6.950374756619249084 ) ) ;
#3543 = CARTESIAN_POINT ( 'NONE',  ( 20.75514604977248467, 46.42500000273119554, -28.56700777964554305 ) ) ;
#3544 = CARTESIAN_POINT ( 'NONE',  ( -4.300734207923759378, 76.47500000273116427, -13.23629886949340495 ) ) ;
#3545 = CARTESIAN_POINT ( 'NONE',  ( -33.58253175000000113, 49.37500000273119127, 0.000000000000000000 ) ) ;
#3546 = CARTESIAN_POINT ( 'NONE',  ( -33.58253175000000113, 29.37500000273118772, 0.000000000000000000 ) ) ;
#3547 = CARTESIAN_POINT ( 'NONE',  ( 17.67679332509665713, 16.99999999999998224, 15.66627074469097458 ) ) ;
#3548 = CARTESIAN_POINT ( 'NONE',  ( -19.09188309203694445, 18.87499999999999645, -19.09188309203661049 ) ) ;
#3549 = DIRECTION ( 'NONE',  ( 0.000000000000000000, 0.000000000000000000, -1.000000000000000000 ) ) ;
#3550 = CARTESIAN_POINT ( 'NONE',  ( -15.00000000000000000, 80.10000000000003695, 4.873795443493597723 ) ) ;
#3551 = CARTESIAN_POINT ( 'NONE',  ( 6.277390505771533514E-15, 70.50000000000001421, 34.17252228774368916 ) ) ;
#3552 = CARTESIAN_POINT ( 'NONE',  ( -27.16883889988623935, 7.325000002731188786, 19.73931689729374739 ) ) ;
#3553 = CARTESIAN_POINT ( 'NONE',  ( 23.41746824999999887, 6.624999997268815832, 0.000000000000000000 ) ) ;
#3554 = LINE ( 'NONE', #11609, #25895 ) ;
#3555 = CARTESIAN_POINT ( 'NONE',  ( 14.01125832528330051, 29.61159749907602290, 24.18731323226221974 ) ) ;
#3556 =( BOUNDED_CURVE ( )  B_SPLINE_CURVE ( 2, ( #18342, #31195, #7685, #462, #2885, #5455, #10944, #29122, #5625, #28614, #3056, #28787, #5113 ),
 .UNSPECIFIED., .F., .F. ) 
 B_SPLINE_CURVE_WITH_KNOTS ( ( 3, 2, 2, 2, 2, 2, 3 ),
 ( 0.6987179487179486781, 0.6999999999999999556, 0.7025641025641025106, 0.7051282051282051766, 0.7076923076923077316, 0.7102564102564102866, 0.7115384615384615641 ),
 .UNSPECIFIED. ) 
 CURVE ( )  GEOMETRIC_REPRESENTATION_ITEM ( )  RATIONAL_B_SPLINE_CURVE ( ( 0.9755282581475768211, 0.9755282581475768211, 1.000000000000000000, 0.9510565162951535312, 1.000000000000000000, 0.9510565162951535312, 1.000000000000000000, 0.9510565162951535312, 1.000000000000000000, 0.9510565162951535312, 1.000000000000000000, 0.9755282581475768211, 0.9755282581475768211 ) ) 
 REPRESENTATION_ITEM ( '' )  );
#3557 = CARTESIAN_POINT ( 'NONE',  ( -7.570916362186215665, 13.39999999999999503, 23.30088464923126423 ) ) ;
#3558 = CARTESIAN_POINT ( 'NONE',  ( 6.486482029760648627E-15, 17.62500000273117351, 35.31076352940722529 ) ) ;
#3559 = CARTESIAN_POINT ( 'NONE',  ( 23.41746824999999887, 5.124999997268814056, 0.000000000000000000 ) ) ;
#3560 = CARTESIAN_POINT ( 'NONE',  ( -2.428612866367529427E-13, 53.67968750000000000, -27.95245687107222921 ) ) ;
#3561 = ORIENTED_EDGE ( 'NONE', *, *, #25807, .F. ) ;
#3562 = CARTESIAN_POINT ( 'NONE',  ( -27.16883889988623935, 57.32500000273120833, 19.73931689729374739 ) ) ;
#3563 = CARTESIAN_POINT ( 'NONE',  ( -27.16883889988623935, 29.57500000273117990, 19.73931689729374739 ) ) ;
#3564 = ADVANCED_FACE ( 'NONE', ( #26994 ), #8798, .F. ) ;
#3565 = ORIENTED_EDGE ( 'NONE', *, *, #25296, .F. ) ;
#3566 = CARTESIAN_POINT ( 'NONE',  ( 2.740863092043355209E-13, 24.46093749999999645, 30.02300923189239512 ) ) ;
#3567 = CARTESIAN_POINT ( 'NONE',  ( -25.98046417659859486, 20.16965250092397355, -15.04653450569291628 ) ) ;
#3568 = CARTESIAN_POINT ( 'NONE',  ( 5.147494310547434893, 38.55125428154683220, 32.49999999999999289 ) ) ;
#3569 = CARTESIAN_POINT ( 'NONE',  ( 1.577395562988744260E-15, 16.24999999453762456, -25.76082449383753925 ) ) ;
#3570 = EDGE_CURVE ( 'NONE', #30585, #14202, #13435, .T. ) ;
#3571 = CARTESIAN_POINT ( 'NONE',  ( -23.41746825000000598, 3.724999997268819918, 7.608796670333726198 ) ) ;
#3572 = CARTESIAN_POINT ( 'NONE',  ( 10.37757302488624056, 28.77500000273120051, -31.93888565452638417 ) ) ;
#3573 = CARTESIAN_POINT ( 'NONE',  ( -20.08610463437157989, 34.20000000546238539, -27.64615127144129758 ) ) ;
#3574 = CARTESIAN_POINT ( 'NONE',  ( 26.29305231718579350, 72.79999999999999716, 19.10302069950537529 ) ) ;
#3575 = LINE ( 'NONE', #24508, #31320 ) ;
#3576 = CARTESIAN_POINT ( 'NONE',  ( 15.00000000000000000, 73.09999999999996589, -4.873795443493596835 ) ) ;
#3577 = CARTESIAN_POINT ( 'NONE',  ( 26.02091320914851025, 59.12798583425730925, -14.97647472619946463 ) ) ;
#3578 = CARTESIAN_POINT ( 'NONE',  ( -10.37757302488624411, 42.97500000273119269, -31.93888565452638417 ) ) ;
#3579 = FILL_AREA_STYLE_COLOUR ( '', #8470 ) ;
#3580 = CARTESIAN_POINT ( 'NONE',  ( -23.41746825000000243, 12.02499999726881974, -7.608796670333730638 ) ) ;
#3581 = CARTESIAN_POINT ( 'NONE',  ( 10.04305231718578817, 21.40000000000000213, -30.90933677959249337 ) ) ;
#3582 = CARTESIAN_POINT ( 'NONE',  ( -19.82091636218621389, 9.200000000000013500, 14.40073868116558842 ) ) ;
#3583 = CARTESIAN_POINT ( 'NONE',  ( -24.18731323226221974, 33.90847249907601935, 14.01125832528330406 ) ) ;
#3584 = CARTESIAN_POINT ( 'NONE',  ( -20.75514604977248823, 62.82500000273119412, -28.56700777964554305 ) ) ;
#3585 = CARTESIAN_POINT ( 'NONE',  ( -20.75514604977248823, 51.07500000273116569, -28.56700777964554305 ) ) ;
#3586 = CARTESIAN_POINT ( 'NONE',  ( 23.41746824999999887, 8.624999997268817609, 0.000000000000000000 ) ) ;
#3587 = CARTESIAN_POINT ( 'NONE',  ( -20.75514604977248112, 3.425000002731186655, 28.56700777964554661 ) ) ;
#3588 = CARTESIAN_POINT ( 'NONE',  ( 26.09010956794232428, 38.64621500092395934, -6.950374756619718042 ) ) ;
#3589 = CARTESIAN_POINT ( 'NONE',  ( 20.08610463437158344, 25.20000000546237473, 27.64615127144129403 ) ) ;
#3590 = CARTESIAN_POINT ( 'NONE',  ( 15.14183272437242422, 2.049999994537635484, -20.84094480462497856 ) ) ;
#3591 = CARTESIAN_POINT ( 'NONE',  ( 20.75514604977249178, 29.82500000273119767, 28.56700777964553950 ) ) ;
#3592 = CARTESIAN_POINT ( 'NONE',  ( 0.000000000000000000, 80.00000000000001421, -32.50000000000000000 ) ) ;
#3593 = CARTESIAN_POINT ( 'NONE',  ( 20.08610463437158344, 61.20000000546237118, 27.64615127144129403 ) ) ;
#3594 = CARTESIAN_POINT ( 'NONE',  ( 10.04305231718578817, 61.39999999999999858, -30.90933677959249337 ) ) ;
#3595 = CARTESIAN_POINT ( 'NONE',  ( 20.53372385742108008, 56.96836833240936215, 20.47846945139866648 ) ) ;
#3596 = CARTESIAN_POINT ( 'NONE',  ( -10.04305231718579172, 50.10000000546236976, -30.90933677959248982 ) ) ;
#3597 = MECHANICAL_DESIGN_GEOMETRIC_PRESENTATION_REPRESENTATION (  '', ( #10711 ), #7987 ) ;
#3598 = CARTESIAN_POINT ( 'NONE',  ( -13.91746824999999887, 71.37500000273116996, 0.000000000000000000 ) ) ;
#3599 = CARTESIAN_POINT ( 'NONE',  ( -32.50000000000000000, 58.50000000546238965, 0.000000000000000000 ) ) ;
#3600 = CARTESIAN_POINT ( 'NONE',  ( 26.07999730980490227, 23.74479166666666430, 6.988114217767821046 ) ) ;
#3601 = ORIENTED_EDGE ( 'NONE', *, *, #9641, .F. ) ;
#3602 = CARTESIAN_POINT ( 'NONE',  ( 10.37757302488624767, 75.72500000273117848, 31.93888565452638417 ) ) ;
#3603 = CARTESIAN_POINT ( 'NONE',  ( 26.00068869287367335, 30.76302083333332504, 15.01150461594596308 ) ) ;
#3604 = EDGE_CURVE ( 'NONE', #22688, #2905, #9132, .T. ) ;
#3605 = CYLINDRICAL_SURFACE ( 'NONE', #16298, 32.50000000000000000 ) ;
#3606 = ORIENTED_EDGE ( 'NONE', *, *, #14450, .F. ) ;
#3607 = CARTESIAN_POINT ( 'NONE',  ( 7.543491769121427382, 51.82329833425730925, -28.00173670424548433 ) ) ;
#3608 = AXIS2_PLACEMENT_3D ( 'NONE', #1026, #24229, #21987 ) ;
#3609 = CARTESIAN_POINT ( 'NONE',  ( 10.04305231718579705, 11.10000000546239285, 30.90933677959248982 ) ) ;
#3610 = CARTESIAN_POINT ( 'NONE',  ( -30.02300923189239512, 59.69531250000000711, 2.654126918244515359E-13 ) ) ;
#3611 = CARTESIAN_POINT ( 'NONE',  ( -8.761981113183991350E-16, -15.84529946162075298, 0.000000000000000000 ) ) ;
#3612 = CARTESIAN_POINT ( 'NONE',  ( -10.37757302488623701, 45.77500000273118985, 31.93888565452638417 ) ) ;
#3613 = CARTESIAN_POINT ( 'NONE',  ( -2.092463501923844636E-15, 50.00000000546237544, -34.17252228774368916 ) ) ;
#3614 = CARTESIAN_POINT ( 'NONE',  ( 15.00000000000000000, 81.00000000000001421, -1.836970198721029589E-15 ) ) ;
#3615 = CARTESIAN_POINT ( 'NONE',  ( 27.16883889988623935, 36.32500000273120122, -19.73931689729374384 ) ) ;
#3616 = CARTESIAN_POINT ( 'NONE',  ( -32.50000000000000000, 62.60000000546238397, 10.55989012756946366 ) ) ;
#3617 = CARTESIAN_POINT ( 'NONE',  ( 20.75514604977249178, 60.07500000273119412, 28.56700777964553950 ) ) ;
#3618 = CARTESIAN_POINT ( 'NONE',  ( 0.000000000000000000, 0.000000000000000000, 0.000000000000000000 ) ) ;
#3619 = CARTESIAN_POINT ( 'NONE',  ( 32.50000000000000711, 32.89999999999997726, 10.55989012756945122 ) ) ;
#3620 = CARTESIAN_POINT ( 'NONE',  ( -2.092463501923844636E-15, 37.50000000000000711, -34.17252228774368916 ) ) ;
#3621 = CARTESIAN_POINT ( 'NONE',  ( 14.47279130897151767, 8.924999997268800556, -19.92008829642072598 ) ) ;
#3622 = CARTESIAN_POINT ( 'NONE',  ( 33.58253175000000823, 4.275000002731189852, 10.91162601494192863 ) ) ;
#3623 = CARTESIAN_POINT ( 'NONE',  ( -5.147494310547450880, 70.94874572391553613, 32.49999999999999289 ) ) ;
#3624 = CARTESIAN_POINT ( 'NONE',  ( -11.25946833292375793, 81.17500000273119554, -8.180482586598733619 ) ) ;
#3625 = CARTESIAN_POINT ( 'NONE',  ( 6.486482029760648627E-15, 71.87500000273116996, 35.31076352940722529 ) ) ;
#3626 = CARTESIAN_POINT ( 'NONE',  ( -7.570916362186210335, 4.599999999999992539, -23.30088464923126779 ) ) ;
#3627 = CARTESIAN_POINT ( 'NONE',  ( -2.162160676586881955E-15, 66.87500000273119838, -35.31076352940723240 ) ) ;
#3628 = ORIENTED_EDGE ( 'NONE', *, *, #1325, .T. ) ;
#3629 = CARTESIAN_POINT ( 'NONE',  ( 24.50000000000000355, 5.849999994537631309, -7.960532557706203605 ) ) ;
#3630 = CARTESIAN_POINT ( 'NONE',  ( 0.04044903254993986036, 10.43006916759064495, -27.95245687107223986 ) ) ;
#3631 = CARTESIAN_POINT ( 'NONE',  ( -4.000000000000003553, 2.020667218593133100E-15, -16.50000000000000000 ) ) ;
#3632 = CARTESIAN_POINT ( 'NONE',  ( -33.58253175000000113, 49.22500000273119269, 10.91162601494193929 ) ) ;
#3633 = CARTESIAN_POINT ( 'NONE',  ( 20.75514604977249178, 8.075000002731185234, 28.56700777964553950 ) ) ;
#3634 = CARTESIAN_POINT ( 'NONE',  ( -10.37757302488623701, 63.77500000273118985, 31.93888565452638417 ) ) ;
#3635 = CARTESIAN_POINT ( 'NONE',  ( -19.09188309203660694, 45.51562500000000000, 19.09188309203694800 ) ) ;
#3636 = CARTESIAN_POINT ( 'NONE',  ( -7.543491769121417612, 39.79204833425731636, 28.00173670424549499 ) ) ;
#3637 = CARTESIAN_POINT ( 'NONE',  ( 7.543491769121922985, 29.75482666574269075, 28.00173670424535644 ) ) ;
#3638 = CARTESIAN_POINT ( 'NONE',  ( -20.08610463437156923, 66.80000000546236549, 27.64615127144130113 ) ) ;
#3639 = DIRECTION ( 'NONE',  ( -0.000000000000000000, -1.000000000000000000, -0.000000000000000000 ) ) ;
#3640 = CARTESIAN_POINT ( 'NONE',  ( 13.94119854578893580, 55.96576416574269786, -24.22776226481265383 ) ) ;
#3641 = CARTESIAN_POINT ( 'NONE',  ( -18.94512977948575738, 17.42499999726882010, -13.76444248337723231 ) ) ;
#3642 = CARTESIAN_POINT ( 'NONE',  ( -19.82091636218621389, 17.19999999999999218, 14.40073868116558842 ) ) ;
#3643 = ORIENTED_EDGE ( 'NONE', *, *, #13848, .F. ) ;
#3644 = CARTESIAN_POINT ( 'NONE',  ( 33.58253175000000113, 44.37500000273119127, -4.112674001490185761E-15 ) ) ;
#3645 = CARTESIAN_POINT ( 'NONE',  ( 14.01125832528286352, 55.40402750092397355, -24.18731323226246843 ) ) ;
#3646 = CARTESIAN_POINT ( 'NONE',  ( 32.50000000000000000, 27.50000000546236478, -3.980102097228898626E-15 ) ) ;
#3647 = VERTEX_POINT ( 'NONE', #32467 ) ;
#3648 = CARTESIAN_POINT ( 'NONE',  ( 33.58253175000000823, 18.02500000273118630, 10.91162601494192863 ) ) ;
#3649 = CARTESIAN_POINT ( 'NONE',  ( 7.505752307972854531, 29.76041666666666430, -28.01184896238303423 ) ) ;
#3650 = ORIENTED_EDGE ( 'NONE', *, *, #20550, .F. ) ;
#3651 = FACE_OUTER_BOUND ( 'NONE', #29908, .T. ) ;
#3652 = CARTESIAN_POINT ( 'NONE',  ( -27.16883889988624290, 52.92500000273120264, -19.73931689729374028 ) ) ;
#3653 = CARTESIAN_POINT ( 'NONE',  ( 15.01150461594643204, 58.54947916666665009, 26.00068869287340334 ) ) ;
#3654 = CARTESIAN_POINT ( 'NONE',  ( -20.08610463437156923, 12.80000000546236016, 27.64615127144130113 ) ) ;
#3655 = CARTESIAN_POINT ( 'NONE',  ( 1.555960095263670572E-15, 16.24999999453762101, -24.50000000000000000 ) ) ;
#3656 = VECTOR ( 'NONE', #10313, 1000.000000000000000 ) ;
#3657 = CARTESIAN_POINT ( 'NONE',  ( -4.523095164977117273E-15, 12.62499999726879807, 24.62258325217400312 ) ) ;
#3658 = CARTESIAN_POINT ( 'NONE',  ( -26.29305231718578995, 60.20000000000000284, 19.10302069950538595 ) ) ;
#3659 = CARTESIAN_POINT ( 'NONE',  ( 20.75514604977248467, 22.67500000273119198, -28.56700777964554305 ) ) ;
#3660 = CARTESIAN_POINT ( 'NONE',  ( 9.270509831248425314, 76.69999999999998863, 12.75976212528059683 ) ) ;
#3661 = CARTESIAN_POINT ( 'NONE',  ( -25.98046417659831420, 68.28347249907602645, 15.04653450569339945 ) ) ;
#3662 = CARTESIAN_POINT ( 'NONE',  ( 8.601468415847516980, 74.17500000273119554, -11.83890561707634781 ) ) ;
#3663 = CARTESIAN_POINT ( 'NONE',  ( 24.50000000000000000, 15.89999999999998970, 7.960532557706212486 ) ) ;
#3664 = DIRECTION ( 'NONE',  ( 1.000000000000000000, 0.000000000000000000, 1.224646799147353947E-16 ) ) ;
#3665 = CIRCLE ( 'NONE', #23090, 14.00000000000000178 ) ;
#3666 = CARTESIAN_POINT ( 'NONE',  ( -2.092463501923844636E-15, 9.499999999999991118, -34.17252228774368916 ) ) ;
#3667 = ORIENTED_EDGE ( 'NONE', *, *, #14686, .T. ) ;
#3668 = CARTESIAN_POINT ( 'NONE',  ( 18.94512977948576093, 9.324999997268824004, -13.76444248337722875 ) ) ;
#3669 = CARTESIAN_POINT ( 'NONE',  ( -13.91746824999999532, 76.77500000273117564, -4.522059556121115875 ) ) ;
#3670 = CARTESIAN_POINT ( 'NONE',  ( -27.95245687107222921, 45.94531249999997868, 2.498001805406602216E-13 ) ) ;
#3671 = CARTESIAN_POINT ( 'NONE',  ( -33.58253175000000113, 19.22500000273118204, 10.91162601494193929 ) ) ;
#3672 = CARTESIAN_POINT ( 'NONE',  ( 20.75514604977249178, 65.82500000273115859, 28.56700777964553950 ) ) ;
#3673 = CARTESIAN_POINT ( 'NONE',  ( 33.58253175000000113, 28.47500000273118204, -10.91162601494193751 ) ) ;
#3674 = CARTESIAN_POINT ( 'NONE',  ( 27.16883889988624290, 18.17500000273118843, 19.73931689729373673 ) ) ;
#3675 = CARTESIAN_POINT ( 'NONE',  ( 27.16883889988624290, 6.175000002731190207, 19.73931689729373673 ) ) ;
#3676 = CARTESIAN_POINT ( 'NONE',  ( 24.22776226481241224, 62.56548583425730925, -13.94119854578936923 ) ) ;
#3677 = CARTESIAN_POINT ( 'NONE',  ( -7.505752307972844761, 52.10416666666666430, 28.01184896238304134 ) ) ;
#3678 = DIRECTION ( 'NONE',  ( -0.000000000000000000, -1.000000000000000000, -0.000000000000000000 ) ) ;
#3679 = CARTESIAN_POINT ( 'NONE',  ( 13.91746824999999887, 80.37500000273118417, -1.704398294459741270E-15 ) ) ;
#3680 = CARTESIAN_POINT ( 'NONE',  ( -10.04305231718578462, 46.39999999999998437, 30.90933677959249337 ) ) ;
#3681 = CARTESIAN_POINT ( 'NONE',  ( 5.147494310547434893, 57.05125428700922185, 32.49999999999999289 ) ) ;
#3682 = CARTESIAN_POINT ( 'NONE',  ( 10.37757302488624767, 49.72500000273119269, 31.93888565452638417 ) ) ;
#3683 = CARTESIAN_POINT ( 'NONE',  ( 7.236395654485755280, 12.72499999726881015, 22.27133577429736988 ) ) ;
#3684 = ORIENTED_EDGE ( 'NONE', *, *, #5519, .T. ) ;
#3685 = CARTESIAN_POINT ( 'NONE',  ( -10.37757302488623701, 65.77500000273118985, 31.93888565452638417 ) ) ;
#3686 = CARTESIAN_POINT ( 'NONE',  ( 5.779280353836490358E-15, 59.00000000546238255, 32.49999999999999289 ) ) ;
#3687 = CARTESIAN_POINT ( 'NONE',  ( 14.47279130897151767, 4.924999997268811214, -19.92008829642072598 ) ) ;
#3688 = CARTESIAN_POINT ( 'NONE',  ( 0.04044903254993986036, 27.61756916759064140, -27.95245687107223986 ) ) ;
#3689 = VERTEX_POINT ( 'NONE', #26833 ) ;
#3690 = VECTOR ( 'NONE', #31924, 1000.000000000000000 ) ;
#3691 = CARTESIAN_POINT ( 'NONE',  ( 20.75514604977249178, 33.82500000273117990, 28.56700777964553950 ) ) ;
#3692 = DIRECTION ( 'NONE',  ( 0.000000000000000000, -0.000000000000000000, 1.000000000000000000 ) ) ;
#3693 = EDGE_LOOP ( 'NONE', ( #11136, #25558, #33859, #1240 ) ) ;
#3694 = CARTESIAN_POINT ( 'NONE',  ( -7.505752307972844761, 55.54166666666667140, 28.01184896238304134 ) ) ;
#3695 = CARTESIAN_POINT ( 'NONE',  ( 33.58253175000000823, 58.27500000273116854, 10.91162601494192863 ) ) ;
#3696 = CARTESIAN_POINT ( 'NONE',  ( 2.375766604868043252, 75.69874572391552192, -14.99999999999999822 ) ) ;
#3697 = CARTESIAN_POINT ( 'NONE',  ( -33.58253175000000113, 77.22500000273117848, 10.91162601494193929 ) ) ;
#3698 = CARTESIAN_POINT ( 'NONE',  ( -7.505752307972844761, 31.47916666666666075, 28.01184896238304134 ) ) ;
#3699 = EDGE_CURVE ( 'NONE', #12256, #17243, #8968, .T. ) ;
#3700 = CARTESIAN_POINT ( 'NONE',  ( 7.570916362186207671, 3.599999999999992095, 23.30088464923126779 ) ) ;
#3701 = CARTESIAN_POINT ( 'NONE',  ( 2.205017735002230837E-13, 57.49999999999999289, -32.50000000000000000 ) ) ;
#3702 = CARTESIAN_POINT ( 'NONE',  ( -27.16883889988623935, 19.32500000273118701, 19.73931689729374739 ) ) ;
#3703 = CARTESIAN_POINT ( 'NONE',  ( -8.601468415847518756, 72.57500000273117280, -11.83890561707634603 ) ) ;
#3704 = CARTESIAN_POINT ( 'NONE',  ( -26.02091320914878025, 48.23138916574269786, -14.97647472619899389 ) ) ;
#3705 = CARTESIAN_POINT ( 'NONE',  ( 12.13525491562420910, 81.19999999999998863, -8.816778784387098611 ) ) ;
#3706 = CARTESIAN_POINT ( 'NONE',  ( -28.01184896238304134, 52.96354166666666430, -7.505752307972844761 ) ) ;
#3707 = EDGE_CURVE ( 'NONE', #11212, #14916, #27280, .T. ) ;
#3708 = EDGE_CURVE ( 'NONE', #13932, #6218, #14295, .T. ) ;
#3709 = CARTESIAN_POINT ( 'NONE',  ( -18.67342709957029001, 16.97452379773154973, 15.98012215616494913 ) ) ;
#3710 = CARTESIAN_POINT ( 'NONE',  ( 5.779280353836490358E-15, 49.00000000546238255, 32.49999999999999289 ) ) ;
#3711 = CARTESIAN_POINT ( 'NONE',  ( -19.09188309203660694, 14.57812499999999645, 19.09188309203694800 ) ) ;
#3712 = CARTESIAN_POINT ( 'NONE',  ( -27.16883889988623935, 39.32500000273120122, 19.73931689729374739 ) ) ;
#3713 = CARTESIAN_POINT ( 'NONE',  ( -8.960552108402742093E-16, 76.37500000273114154, -14.63369212191046387 ) ) ;
#3714 = CARTESIAN_POINT ( 'NONE',  ( -27.16883889988623935, 51.57500000273117280, 19.73931689729374739 ) ) ;
#3715 = CARTESIAN_POINT ( 'NONE',  ( 10.37757302488624056, 26.77500000273119696, -31.93888565452638417 ) ) ;
#3716 = CARTESIAN_POINT ( 'NONE',  ( 24.50000000000000000, 17.89999999999998437, 7.960532557706212486 ) ) ;
#3717 = CARTESIAN_POINT ( 'NONE',  ( 13.97622843553633842, 34.48697916666666430, 24.20753774853730889 ) ) ;
#3718 = CARTESIAN_POINT ( 'NONE',  ( 7.570916362186207671, 11.34999999453761887, 23.30088464923126779 ) ) ;
#3719 = VECTOR ( 'NONE', #3822, 1000.000000000000000 ) ;
#3720 = CARTESIAN_POINT ( 'NONE',  ( 5.147494310547434893, 30.55125428154684997, 32.49999999999999289 ) ) ;
#3721 = CARTESIAN_POINT ( 'NONE',  ( -20.08610463437156923, 64.29999999999996874, 27.64615127144130113 ) ) ;
#3722 = CARTESIAN_POINT ( 'NONE',  ( -2.162160676586881955E-15, 6.625000002731173510, -35.31076352940723240 ) ) ;
#3723 = CARTESIAN_POINT ( 'NONE',  ( -7.236395654485763274, 2.024999997268822405, 22.27133577429736633 ) ) ;
#3724 = CARTESIAN_POINT ( 'NONE',  ( 20.53372385742108008, 26.03086833240935860, 20.47846945139866648 ) ) ;
#3725 = FACE_OUTER_BOUND ( 'NONE', #17369, .T. ) ;
#3726 = CARTESIAN_POINT ( 'NONE',  ( -13.94119854578892514, 30.18451416574268720, 24.22776226481266448 ) ) ;
#3727 = DIRECTION ( 'NONE',  ( 0.000000000000000000, -1.000000000000000000, 0.000000000000000000 ) ) ;
#3728 = CARTESIAN_POINT ( 'NONE',  ( -10.37757302488624411, 22.72500000273119980, -31.93888565452638417 ) ) ;
#3729 = CARTESIAN_POINT ( 'NONE',  ( -18.94512977948575738, 5.924999997268809437, -13.76444248337723231 ) ) ;
#3730 = CARTESIAN_POINT ( 'NONE',  ( 26.07999730980477437, 50.95833333333332860, -6.988114217768290004 ) ) ;
#3731 = VERTEX_POINT ( 'NONE', #3167 ) ;
#3732 = CARTESIAN_POINT ( 'NONE',  ( -20.75514604977248823, 58.82500000273117990, -28.56700777964554305 ) ) ;
#3733 = CARTESIAN_POINT ( 'NONE',  ( 20.75514604977249178, 28.07500000273119412, 28.56700777964553950 ) ) ;
#3734 = VERTEX_POINT ( 'NONE', #3329 ) ;
#3735 = CARTESIAN_POINT ( 'NONE',  ( 20.50609665441005092, 27.46875000000000000, 20.50609665440969209 ) ) ;
#3736 = CARTESIAN_POINT ( 'NONE',  ( -28.00173670424549499, 26.90142333425731280, -7.543491769121417612 ) ) ;
#3737 = CARTESIAN_POINT ( 'NONE',  ( 26.29305231718579350, 38.80000000000000426, 19.10302069950537529 ) ) ;
#3738 = CARTESIAN_POINT ( 'NONE',  ( -24.50000000000001066, 16.84999999453763309, 7.960532557706201828 ) ) ;
#3739 = CARTESIAN_POINT ( 'NONE',  ( 18.94512977948576093, 2.824999997268817786, -13.76444248337722875 ) ) ;
#3740 = CARTESIAN_POINT ( 'NONE',  ( -2.162160676586881955E-15, 18.87500000273119483, -35.31076352940723240 ) ) ;
#3741 = CARTESIAN_POINT ( 'NONE',  ( 26.29305231718578995, 31.70000000546238539, -19.10302069950538240 ) ) ;
#3742 = CARTESIAN_POINT ( 'NONE',  ( -20.08610463437157989, 71.69999999999997442, -27.64615127144129758 ) ) ;
#3743 = DIRECTION ( 'NONE',  ( 0.000000000000000000, 1.000000000000000000, 0.000000000000000000 ) ) ;
#3744 = CARTESIAN_POINT ( 'NONE',  ( 0.04044903254992426173, 55.11756916759064495, -30.02300923189239867 ) ) ;
#3745 = CARTESIAN_POINT ( 'NONE',  ( -10.37757302488623701, 37.77500000273118275, 31.93888565452638417 ) ) ;
#3746 = CARTESIAN_POINT ( 'NONE',  ( -28.01184896238290278, 25.17708333333332860, 7.505752307973363457 ) ) ;
#3747 = CARTESIAN_POINT ( 'NONE',  ( 23.41746825000000243, 11.22499999726881548, -7.608796670333727974 ) ) ;
#3748 = CARTESIAN_POINT ( 'NONE',  ( -32.50000000000000000, 12.00000000000001066, 0.000000000000000000 ) ) ;
#3749 = CARTESIAN_POINT ( 'NONE',  ( 19.82091636218621034, 13.80000000000000604, 14.40073868116559730 ) ) ;
#3750 = CARTESIAN_POINT ( 'NONE',  ( -6.950374756619247307, 47.22878499907602645, 26.09010956794245217 ) ) ;
#3751 = CARTESIAN_POINT ( 'NONE',  ( -27.16883889988623935, 61.32500000273119412, 19.73931689729374739 ) ) ;
#3752 = CARTESIAN_POINT ( 'NONE',  ( 20.75514604977249178, 46.07500000273117280, 28.56700777964553950 ) ) ;
#3753 = CARTESIAN_POINT ( 'NONE',  ( 23.41746824999999887, 10.72499999726880127, -7.608796670333727974 ) ) ;
#3754 = CARTESIAN_POINT ( 'NONE',  ( 24.50000000000000000, 3.749999994537622783, 0.000000000000000000 ) ) ;
#3755 = CARTESIAN_POINT ( 'NONE',  ( 10.37757302488624767, 7.725000002731185589, 31.93888565452638417 ) ) ;
#3756 = CARTESIAN_POINT ( 'NONE',  ( -13.94119854578936923, 37.64361083425730925, -24.22776226481241224 ) ) ;
#3757 = EDGE_CURVE ( 'NONE', #16950, #4399, #21280, .T. ) ;
#3758 =( BOUNDED_CURVE ( )  B_SPLINE_CURVE ( 2, ( #13535, #15776, #26232, #2721, #23998, #10106, #20585, #26399, #10615, #28457, #2892, #13020, #18180 ),
 .UNSPECIFIED., .F., .T. ) 
 B_SPLINE_CURVE_WITH_KNOTS ( ( 3, 2, 2, 2, 2, 2, 3 ),
 ( 0.4166666666666666852, 0.4222222222222222210, 0.4333333333333333481, 0.4444444444444444198, 0.4555555555555555469, 0.4666666666666666741, 0.4722222222222222099 ),
 .UNSPECIFIED. ) 
 CURVE ( )  GEOMETRIC_REPRESENTATION_ITEM ( )  RATIONAL_B_SPLINE_CURVE ( ( 0.9755282581475767101, 0.9755282581475768211, 1.000000000000000000, 0.9510565162951535312, 1.000000000000000000, 0.9510565162951535312, 1.000000000000000000, 0.9510565162951535312, 1.000000000000000000, 0.9510565162951535312, 1.000000000000000000, 0.9755282581475768211, 0.9755282581475765991 ) ) 
 REPRESENTATION_ITEM ( '' )  );
#3759 = CARTESIAN_POINT ( 'NONE',  ( 3.445340210940985210E-14, 9.249999994537636994, 24.50000000000000000 ) ) ;
#3760 = CARTESIAN_POINT ( 'NONE',  ( -20.08610463437157989, 41.69999999999999574, -27.64615127144129758 ) ) ;
#3761 = UNCERTAINTY_MEASURE_WITH_UNIT (LENGTH_MEASURE( 1.000000000000000082E-05 ), #29170, 'distance_accuracy_value', 'NONE');
#3762 = CARTESIAN_POINT ( 'NONE',  ( -33.58253175000000113, 27.12500000273120193, 0.000000000000000000 ) ) ;
#3763 = CARTESIAN_POINT ( 'NONE',  ( 0.000000000000000000, 0.000000000000000000, 0.000000000000000000 ) ) ;
#3764 = DIRECTION ( 'NONE',  ( 0.000000000000000000, 0.000000000000000000, -1.000000000000000000 ) ) ;
#3765 = CARTESIAN_POINT ( 'NONE',  ( -1.778240108872766143E-15, 30.00000000546237189, -32.49999999999999289 ) ) ;
#3766 = CARTESIAN_POINT ( 'NONE',  ( -28.00173670424535644, 54.67670166574269075, 7.543491769121936308 ) ) ;
#3767 = CARTESIAN_POINT ( 'NONE',  ( 32.50000000000000000, 47.50000000546238255, -3.980102097228898626E-15 ) ) ;
#3768 = DIRECTION ( 'NONE',  ( -0.2588190451025255689, -0.9659258262890669799, 3.169619151431825338E-17 ) ) ;
#3769 = CARTESIAN_POINT ( 'NONE',  ( 26.07999730980477437, 23.45833333333333215, -6.988114217768290004 ) ) ;
#3770 = ORIENTED_EDGE ( 'NONE', *, *, #15128, .F. ) ;
#3771 = CARTESIAN_POINT ( 'NONE',  ( -10.37757302488623701, 77.52500000273120406, 31.93888565452638417 ) ) ;
#3772 = CARTESIAN_POINT ( 'NONE',  ( -2.584737979205441561E-13, 29.61718749999999645, -30.02300923189239512 ) ) ;
#3773 = CARTESIAN_POINT ( 'NONE',  ( 3.469446951953614189E-15, -45.00000000000000000, 0.000000000000000000 ) ) ;
#3774 = VERTEX_POINT ( 'NONE', #11060 ) ;
#3775 = CARTESIAN_POINT ( 'NONE',  ( -15.04653450569291984, 50.24777750092398065, 25.98046417659859486 ) ) ;
#3776 = CARTESIAN_POINT ( 'NONE',  ( 26.29305231718579350, 9.300000005462369046, 19.10302069950537529 ) ) ;
#3777 = CARTESIAN_POINT ( 'NONE',  ( -7.505752307972844761, 62.41666666666666430, 28.01184896238304134 ) ) ;
#3778 = CARTESIAN_POINT ( 'NONE',  ( 5.779280353836490358E-15, 47.00000000546238255, 32.49999999999999289 ) ) ;
#3779 = CARTESIAN_POINT ( 'NONE',  ( 33.58253175000000823, 46.27500000273120406, 10.91162601494192863 ) ) ;
#3780 = CARTESIAN_POINT ( 'NONE',  ( -26.29305231718579350, 52.30000000546236549, -19.10302069950537884 ) ) ;
#3781 = CARTESIAN_POINT ( 'NONE',  ( 4.300734207923757602, 74.77500000273118985, -13.23629886949340673 ) ) ;
#3782 = CARTESIAN_POINT ( 'NONE',  ( -10.37757302488624411, 30.72500000273117848, -31.93888565452638417 ) ) ;
#3783 = CARTESIAN_POINT ( 'NONE',  ( 15.14183272437242067, 11.70000000000000817, 20.84094480462498211 ) ) ;
#3784 = CARTESIAN_POINT ( 'NONE',  ( -27.16883889988623935, 59.57500000273119412, 19.73931689729374739 ) ) ;
#3785 =( NAMED_UNIT ( * ) PLANE_ANGLE_UNIT ( ) SI_UNIT ( $, .RADIAN. ) );
#3786 = CARTESIAN_POINT ( 'NONE',  ( -26.29305231718578995, 36.19999999999999574, 19.10302069950538595 ) ) ;
#3787 = CARTESIAN_POINT ( 'NONE',  ( 10.04305231718578817, 35.39999999999998437, -30.90933677959249337 ) ) ;
#3788 = CARTESIAN_POINT ( 'NONE',  ( -23.41746825000000243, 9.524999997268810858, -7.608796670333730638 ) ) ;
#3789 = CARTESIAN_POINT ( 'NONE',  ( 20.75514604977249178, 4.075000002731195892, 28.56700777964553950 ) ) ;
#3790 = CARTESIAN_POINT ( 'NONE',  ( 10.04305231718579705, 12.59999999999999964, 30.90933677959248982 ) ) ;
#3791 = CARTESIAN_POINT ( 'NONE',  ( -8.601468415847515203, 79.67500000273115290, 11.83890561707634959 ) ) ;
#3792 = CARTESIAN_POINT ( 'NONE',  ( 10.37757302488624056, 64.77500000273117564, -31.93888565452638417 ) ) ;
#3793 = CARTESIAN_POINT ( 'NONE',  ( 33.58253175000000823, 60.27500000273116143, 10.91162601494192863 ) ) ;
#3794 = ORIENTED_EDGE ( 'NONE', *, *, #7358, .F. ) ;
#3795 = CARTESIAN_POINT ( 'NONE',  ( 7.570916362186207671, 7.349999994537615322, 23.30088464923126779 ) ) ;
#3796 = CARTESIAN_POINT ( 'NONE',  ( -26.07999730980490583, 66.71354166666665719, -6.988114217767815717 ) ) ;
#3797 = ADVANCED_FACE ( 'NONE', ( #8468 ), #735, .F. ) ;
#3798 = DIRECTION ( 'NONE',  ( 0.000000000000000000, 0.000000000000000000, 1.000000000000000000 ) ) ;
#3799 = CARTESIAN_POINT ( 'NONE',  ( 27.16883889988623935, 50.32500000273120122, -19.73931689729374384 ) ) ;
#3800 = CARTESIAN_POINT ( 'NONE',  ( -20.75514604977248823, 13.07500000273118879, -28.56700777964554305 ) ) ;
#3801 = CARTESIAN_POINT ( 'NONE',  ( 27.16883889988623935, 60.57500000273117990, -19.73931689729374384 ) ) ;
#3802 = CARTESIAN_POINT ( 'NONE',  ( 6.988114217767829928, 50.38541666666666430, -26.07999730980489872 ) ) ;
#3803 = CARTESIAN_POINT ( 'NONE',  ( -7.468012846824771955, 37.78684000092396644, -28.02196122052045624 ) ) ;
#3804 = EDGE_CURVE ( 'NONE', #2692, #30646, #17443, .T. ) ;
#3805 = CARTESIAN_POINT ( 'NONE',  ( 14.97647472619900455, 28.46576416574268720, -26.02091320914876960 ) ) ;
#3806 = CARTESIAN_POINT ( 'NONE',  ( 26.29305231718578995, 65.70000000546237118, -19.10302069950538240 ) ) ;
#3807 = CARTESIAN_POINT ( 'NONE',  ( -4.300734207923755825, 77.27500000273118985, 13.23629886949340673 ) ) ;
#3808 = CARTESIAN_POINT ( 'NONE',  ( 24.18731323226221974, 52.81472249907603356, -14.01125832528328985 ) ) ;
#3809 = DIRECTION ( 'NONE',  ( -0.000000000000000000, -1.000000000000000000, -0.000000000000000000 ) ) ;
#3810 = DIRECTION ( 'NONE',  ( 0.000000000000000000, -1.000000000000000000, 0.000000000000000000 ) ) ;
#3811 = VERTEX_POINT ( 'NONE', #20298 ) ;
#3812 = CARTESIAN_POINT ( 'NONE',  ( 10.37757302488624767, 39.97500000273117138, 31.93888565452638417 ) ) ;
#3813 = CARTESIAN_POINT ( 'NONE',  ( -4.523095164977117273E-15, 4.624999997268820273, 24.62258325217400312 ) ) ;
#3814 = CARTESIAN_POINT ( 'NONE',  ( -2.092463501923844636E-15, 32.00000000546236834, -34.17252228774368916 ) ) ;
#3815 = VERTEX_POINT ( 'NONE', #30748 ) ;
#3816 = CARTESIAN_POINT ( 'NONE',  ( 7.505752307972854531, 33.19791666666665719, -28.01184896238303423 ) ) ;
#3817 = EDGE_LOOP ( 'NONE', ( #32106, #15090, #16719, #14877 ) ) ;
#3818 = CARTESIAN_POINT ( 'NONE',  ( -32.50000000000000000, 74.40000000546234560, -10.55989012756945300 ) ) ;
#3819 = CARTESIAN_POINT ( 'NONE',  ( -10.37757302488624411, 56.72500000273117138, -31.93888565452638417 ) ) ;
#3820 = CARTESIAN_POINT ( 'NONE',  ( -20.50609665440969209, 59.26562500000000000, 20.50609665441005092 ) ) ;
#3821 = CARTESIAN_POINT ( 'NONE',  ( -10.04305231718579172, 12.10000000546238041, -30.90933677959248982 ) ) ;
#3822 = DIRECTION ( 'NONE',  ( -0.000000000000000000, -1.000000000000000000, -0.000000000000000000 ) ) ;
#3823 = CARTESIAN_POINT ( 'NONE',  ( 18.94512977948576093, 15.32499999726882933, -13.76444248337722875 ) ) ;
#3824 = CARTESIAN_POINT ( 'NONE',  ( -32.50000000000000000, 53.99999999999999289, 0.000000000000000000 ) ) ;
#3825 = CARTESIAN_POINT ( 'NONE',  ( 10.37757302488624056, 26.77500000273119696, -31.93888565452638417 ) ) ;
#3826 = DIRECTION ( 'NONE',  ( 0.000000000000000000, 0.000000000000000000, -1.000000000000000000 ) ) ;
#3827 = CARTESIAN_POINT ( 'NONE',  ( -19.11951029504797006, 17.43711833240935505, -19.06425588902558133 ) ) ;
#3828 = CARTESIAN_POINT ( 'NONE',  ( -13.91746824999999532, 72.97500000273117848, 4.522059556121122093 ) ) ;
#3829 = CARTESIAN_POINT ( 'NONE',  ( -8.891200544363830713E-16, 75.75000000546236834, -15.00000000000000000 ) ) ;
#3830 = CARTESIAN_POINT ( 'NONE',  ( -5.147494310547423346, 34.44874571845313938, 32.50000000000000000 ) ) ;
#3831 = CARTESIAN_POINT ( 'NONE',  ( -32.50000000000000000, 8.099999999999990763, 10.55989012756946366 ) ) ;
#3832 = ORIENTED_EDGE ( 'NONE', *, *, #7432, .T. ) ;
#3833 = CARTESIAN_POINT ( 'NONE',  ( 18.94512977948575738, 4.924999997268808549, 13.76444248337723408 ) ) ;
#3834 = CARTESIAN_POINT ( 'NONE',  ( 32.50000000000000000, 71.60000000546240528, -10.55989012756945833 ) ) ;
#3835 = CARTESIAN_POINT ( 'NONE',  ( 24.20753774853731244, 37.06510416666666430, -13.97622843553632599 ) ) ;
#3836 = CARTESIAN_POINT ( 'NONE',  ( -27.16883889988623935, 65.32500000273118701, 19.73931689729374739 ) ) ;
#3837 = CARTESIAN_POINT ( 'NONE',  ( 33.58253175000000113, 28.37500000273117351, -4.112674001490185761E-15 ) ) ;
#3838 = CARTESIAN_POINT ( 'NONE',  ( 6.486482029760649416E-15, 15.87500000273120015, 35.31076352940723240 ) ) ;
#3839 = CARTESIAN_POINT ( 'NONE',  ( -20.75514604977248112, 11.67500000273118843, 28.56700777964554661 ) ) ;
#3840 = CARTESIAN_POINT ( 'NONE',  ( 26.06988505166735592, 62.99517333425730214, 7.025853678916393896 ) ) ;
#3841 = CARTESIAN_POINT ( 'NONE',  ( -28.01184896238304134, 52.96354166666666430, -7.505752307972844761 ) ) ;
#3842 = CARTESIAN_POINT ( 'NONE',  ( 24.50000000000000000, 5.899999999999987921, 7.960532557706212486 ) ) ;
#3843 = CARTESIAN_POINT ( 'NONE',  ( 13.91746825000000065, 74.27500000273118985, 4.522059556121115875 ) ) ;
#3844 = CARTESIAN_POINT ( 'NONE',  ( 26.29305231718578995, 49.20000000000000995, -19.10302069950538240 ) ) ;
#3845 = CARTESIAN_POINT ( 'NONE',  ( 1.555960095263670572E-15, 8.249999994537619230, -24.50000000000000000 ) ) ;
#3846 = CARTESIAN_POINT ( 'NONE',  ( 20.75514604977248467, 52.42500000273118133, -28.56700777964554305 ) ) ;
#3847 = CARTESIAN_POINT ( 'NONE',  ( -4.523095164977116484E-15, 2.124999997268812280, 24.62258325217400312 ) ) ;
#3848 = ORIENTED_EDGE ( 'NONE', *, *, #23533, .F. ) ;
#3849 = CARTESIAN_POINT ( 'NONE',  ( 6.486482029760649416E-15, 59.87500000273117706, 35.31076352940723240 ) ) ;
#3850 = DIRECTION ( 'NONE',  ( 0.000000000000000000, -1.000000000000000000, 0.000000000000000000 ) ) ;
#3851 = CARTESIAN_POINT ( 'NONE',  ( -14.47279130897151589, 7.324999997268822227, -19.92008829642072598 ) ) ;
#3852 = CARTESIAN_POINT ( 'NONE',  ( 26.06988505166735592, 35.49517333425730214, 7.025853678916393896 ) ) ;
#3853 =( BOUNDED_CURVE ( )  B_SPLINE_CURVE ( 2, ( #30289, #17442, #6791, #29957, #16935, #33204, #9355, #17268, #15038, #20188, #27731, #27393, #4559 ),
 .UNSPECIFIED., .F., .T. ) 
 B_SPLINE_CURVE_WITH_KNOTS ( ( 3, 2, 2, 2, 2, 2, 3 ),
 ( 0.08333333333333334259, 0.08888888888888889228, 0.1000000000000000056, 0.1111111111111111049, 0.1222222222222222321, 0.1333333333333333315, 0.1388888888888888951 ),
 .UNSPECIFIED. ) 
 CURVE ( )  GEOMETRIC_REPRESENTATION_ITEM ( )  RATIONAL_B_SPLINE_CURVE ( ( 0.9755282581475768211, 0.9755282581475768211, 1.000000000000000000, 0.9510565162951535312, 1.000000000000000000, 0.9510565162951535312, 1.000000000000000000, 0.9510565162951535312, 1.000000000000000000, 0.9510565162951535312, 1.000000000000000000, 0.9755282581475767101, 0.9755282581475768211 ) ) 
 REPRESENTATION_ITEM ( '' )  );
#3854 = ORIENTED_EDGE ( 'NONE', *, *, #15671, .T. ) ;
#3855 = CARTESIAN_POINT ( 'NONE',  ( -33.58253175000000113, 35.22500000273119980, 10.91162601494193929 ) ) ;
#3856 = CYLINDRICAL_SURFACE ( 'NONE', #19802, 32.50000000000000000 ) ;
#3857 = EDGE_CURVE ( 'NONE', #6723, #33526, #1843, .T. ) ;
#3858 = ORIENTED_EDGE ( 'NONE', *, *, #31876, .F. ) ;
#3860 = CARTESIAN_POINT ( 'NONE',  ( 7.505752307973351023, 48.38020833333332860, 28.01184896238290278 ) ) ;
#3859 =( BOUNDED_CURVE ( )  B_SPLINE_CURVE ( 2, ( #1413, #3830, #8805, #9140, #5909, #32313, #1238, #3998, #14471, #3498, #8641, #8976, #24760 ),
 .UNSPECIFIED., .F., .T. ) 
 B_SPLINE_CURVE_WITH_KNOTS ( ( 3, 2, 2, 2, 2, 2, 3 ),
 ( 0.5833333333333333703, 0.5846153846153846478, 0.5871794871794872028, 0.5897435897435897578, 0.5923076923076923128, 0.5948717948717948678, 0.5961538461538461453 ),
 .UNSPECIFIED. ) 
 CURVE ( )  GEOMETRIC_REPRESENTATION_ITEM ( )  RATIONAL_B_SPLINE_CURVE ( ( 0.9755282581475768211, 0.9755282581475768211, 1.000000000000000000, 0.9510565162951535312, 1.000000000000000000, 0.9510565162951535312, 1.000000000000000000, 0.9510565162951535312, 1.000000000000000000, 0.9510565162951535312, 1.000000000000000000, 0.9755282581475768211, 0.9755282581475768211 ) ) 
 REPRESENTATION_ITEM ( '' )  );
#3861 = CARTESIAN_POINT ( 'NONE',  ( -2.162160676586881955E-15, 58.87500000273117706, -35.31076352940723240 ) ) ;
#3862 = CARTESIAN_POINT ( 'NONE',  ( -20.08610463437157989, 36.20000000546237828, -27.64615127144129758 ) ) ;
#3863 = CARTESIAN_POINT ( 'NONE',  ( 33.58253175000000823, 74.02500000273120406, 10.91162601494192863 ) ) ;
#3864 = CARTESIAN_POINT ( 'NONE',  ( 26.00068869287367335, 30.76302083333332504, 15.01150461594596308 ) ) ;
#3865 = CARTESIAN_POINT ( 'NONE',  ( -7.570916362186215665, 5.399999999999987921, 23.30088464923126423 ) ) ;
#3866 = CARTESIAN_POINT ( 'NONE',  ( 0.000000000000000000, 0.000000000000000000, 24.50000000000000000 ) ) ;
#3867 = CARTESIAN_POINT ( 'NONE',  ( -27.16883889988623935, 15.32500000273118168, 19.73931689729374739 ) ) ;
#3868 = CARTESIAN_POINT ( 'NONE',  ( -4.300734207923755825, 73.27500000273118985, 13.23629886949340673 ) ) ;
#3869 = CARTESIAN_POINT ( 'NONE',  ( 0.04044903255045854962, 43.64805583240936215, 30.02300923189239867 ) ) ;
#3870 = CARTESIAN_POINT ( 'NONE',  ( -4.635254915624208216, 80.40000000000000568, 14.26584774442730463 ) ) ;
#3871 = CARTESIAN_POINT ( 'NONE',  ( -2.584737979205442066E-13, 53.67968750000000000, -30.02300923189239867 ) ) ;
#3872 = CARTESIAN_POINT ( 'NONE',  ( 5.779280353836490358E-15, 53.00000000546238255, 32.49999999999999289 ) ) ;
#3873 = CARTESIAN_POINT ( 'NONE',  ( 24.50000000000000000, 7.749999994537626336, 0.000000000000000000 ) ) ;
#3874 = CARTESIAN_POINT ( 'NONE',  ( -20.08610463437156923, 54.80000000546236549, 27.64615127144130113 ) ) ;
#3875 = CARTESIAN_POINT ( 'NONE',  ( 2.584737979205441561E-13, 14.14843749999999289, 27.95245687107222921 ) ) ;
#3876 = CARTESIAN_POINT ( 'NONE',  ( 10.37757302488624056, 36.52500000273117564, -31.93888565452638417 ) ) ;
#3877 = CARTESIAN_POINT ( 'NONE',  ( -13.91746824999999532, 76.77500000273118985, -4.522059556121115875 ) ) ;
#3878 = CARTESIAN_POINT ( 'NONE',  ( -10.37757302488624411, 50.97500000273118559, -31.93888565452638417 ) ) ;
#3879 = CARTESIAN_POINT ( 'NONE',  ( -27.16883889988624290, 31.17500000273118488, -19.73931689729374028 ) ) ;
#3880 = CARTESIAN_POINT ( 'NONE',  ( -16.57479016809132588, 16.99999999999998579, 18.03908112418252685 ) ) ;
#3881 = CARTESIAN_POINT ( 'NONE',  ( -26.07999730980477437, 35.48958333333332860, 6.988114217768305103 ) ) ;
#3882 = CARTESIAN_POINT ( 'NONE',  ( -20.08610463437157989, 17.69999999999999218, -27.64615127144129758 ) ) ;
#3883 = LINE ( 'NONE', #17103, #23419 ) ;
#3884 = CARTESIAN_POINT ( 'NONE',  ( -32.50000000000000000, 65.89999999999997726, -10.55989012756945478 ) ) ;
#3885 = CARTESIAN_POINT ( 'NONE',  ( 23.41746824999999887, 12.72499999726882791, -7.608796670333727974 ) ) ;
#3886 = CARTESIAN_POINT ( 'NONE',  ( -0.04044903255044120238, 21.30430583240935860, -30.02300923189239867 ) ) ;
#3887 = EDGE_CURVE ( 'NONE', #438, #26701, #7237, .T. ) ;
#3888 = CARTESIAN_POINT ( 'NONE',  ( -7.570916362186210335, 10.34999999453761710, -23.30088464923126779 ) ) ;
#3889 = CARTESIAN_POINT ( 'NONE',  ( -24.22776226481266448, 41.35638916574269075, -13.94119854578892514 ) ) ;
#3890 = FILL_AREA_STYLE_COLOUR ( '', #2480 ) ;
#3891 = CARTESIAN_POINT ( 'NONE',  ( 10.37757302488624056, 10.52500000273118275, -31.93888565452638417 ) ) ;
#3892 = CARTESIAN_POINT ( 'NONE',  ( -14.47279130897151589, 7.824999997268807128, -19.92008829642072598 ) ) ;
#3893 = CARTESIAN_POINT ( 'NONE',  ( 24.20753774853731244, 57.69010416666667140, -13.97622843553632599 ) ) ;
#3894 = EDGE_CURVE ( 'NONE', #24457, #29888, #5374, .T. ) ;
#3895 = ORIENTED_EDGE ( 'NONE', *, *, #24650, .T. ) ;
#3896 = CARTESIAN_POINT ( 'NONE',  ( -2.162160676586881955E-15, 56.62500000273116996, -35.31076352940723240 ) ) ;
#3897 = CARTESIAN_POINT ( 'NONE',  ( 33.58253175000000113, 30.37500000273117706, -4.112674001490185761E-15 ) ) ;
#3898 = ORIENTED_EDGE ( 'NONE', *, *, #10326, .T. ) ;
#3899 = CARTESIAN_POINT ( 'NONE',  ( 15.01150461594643204, 20.73697916666666075, 26.00068869287340334 ) ) ;
#3900 = CARTESIAN_POINT ( 'NONE',  ( -28.00173670424549499, 20.02642333425731280, -7.543491769121417612 ) ) ;
#3901 = CARTESIAN_POINT ( 'NONE',  ( 1.555960095263670572E-15, 16.24999999453762101, -24.50000000000000000 ) ) ;
#3902 = CARTESIAN_POINT ( 'NONE',  ( 7.570916362186207671, 17.34999999453762243, 23.30088464923126779 ) ) ;
#3903 = EDGE_CURVE ( 'NONE', #17565, #30177, #21758, .T. ) ;
#3904 = CARTESIAN_POINT ( 'NONE',  ( -18.94512977948575738, 3.424999997268807217, -13.76444248337723231 ) ) ;
#3905 = CARTESIAN_POINT ( 'NONE',  ( 20.75514604977248467, 24.67500000273118843, -28.56700777964554305 ) ) ;
#3906 = CARTESIAN_POINT ( 'NONE',  ( 20.08610463437157279, 29.80000000546237970, -27.64615127144129758 ) ) ;
#3907 = CARTESIAN_POINT ( 'NONE',  ( 32.50000000000000711, 74.90000000000000568, 10.55989012756945122 ) ) ;
#3908 = CARTESIAN_POINT ( 'NONE',  ( -1.778240108872766143E-15, 58.00000000546237544, -32.49999999999999289 ) ) ;
#3909 = CARTESIAN_POINT ( 'NONE',  ( -29.16592172374821601, 67.00000000000004263, -16.79171150063893236 ) ) ;
#3910 = CARTESIAN_POINT ( 'NONE',  ( -25.98046417659859486, 57.98215250092397355, -15.04653450569291628 ) ) ;
#3911 = CARTESIAN_POINT ( 'NONE',  ( 10.37757302488624056, 38.77500000273118275, -31.93888565452638417 ) ) ;
#3912 = CARTESIAN_POINT ( 'NONE',  ( 27.16883889988624290, 57.92500000273119554, 19.73931689729373673 ) ) ;
#3913 = CARTESIAN_POINT ( 'NONE',  ( 28.01184896238304134, 30.61979166666666075, 7.505752307972846538 ) ) ;
#3914 = CARTESIAN_POINT ( 'NONE',  ( 23.41746825000000243, 11.02499999726882152, 7.608796670333735079 ) ) ;
#3915 = CARTESIAN_POINT ( 'NONE',  ( 10.04305231718578817, 15.39999999999999680, -30.90933677959249337 ) ) ;
#3916 = CARTESIAN_POINT ( 'NONE',  ( 15.14183272437242245, 10.29999999999999361, -20.84094480462497856 ) ) ;
#3917 = CARTESIAN_POINT ( 'NONE',  ( -14.01125832528328985, 45.08034749907603356, -24.18731323226223040 ) ) ;
#3918 = CARTESIAN_POINT ( 'NONE',  ( 6.486482029760649416E-15, 53.62500000273119838, 35.31076352940723240 ) ) ;
#3919 = CARTESIAN_POINT ( 'NONE',  ( 20.75514604977248467, 46.67500000273118133, -28.56700777964554305 ) ) ;
#3920 = CARTESIAN_POINT ( 'NONE',  ( 1.507698388325705758E-15, 13.12499999726881228, -24.62258325217400312 ) ) ;
#3921 = CARTESIAN_POINT ( 'NONE',  ( 24.50000000000000000, 10.00000000000000888, 0.000000000000000000 ) ) ;
#3922 = FACE_OUTER_BOUND ( 'NONE', #810, .T. ) ;
#3923 = CARTESIAN_POINT ( 'NONE',  ( 24.22776226481241224, 35.06548583425731636, -13.94119854578936923 ) ) ;
#3924 = CARTESIAN_POINT ( 'NONE',  ( -9.163862182818718338, 16.99999999999998224, -22.02512863723370629 ) ) ;
#3925 = CARTESIAN_POINT ( 'NONE',  ( -5.147494310547423346, 42.44874571845314648, 32.50000000000000000 ) ) ;
#3926 = CARTESIAN_POINT ( 'NONE',  ( 33.58253175000000113, 30.12500000273120193, -4.112674001490185761E-15 ) ) ;
#3928 = AXIS2_PLACEMENT_3D ( 'NONE', #4887, #4714, #2313 ) ;
#3927 = CARTESIAN_POINT ( 'NONE',  ( 0.000000000000000000, 80.00000000000001421, -32.50000000000000000 ) ) ;
#3929 = CARTESIAN_POINT ( 'NONE',  ( 20.08610463437158344, 52.69999999999998863, 27.64615127144129403 ) ) ;
#3930 = CARTESIAN_POINT ( 'NONE',  ( 5.147494310547426899, 1.948745723915527472, -32.50000000000000000 ) ) ;
#3931 = CARTESIAN_POINT ( 'NONE',  ( -25.98046417659831420, 54.53347249907601935, 15.04653450569339945 ) ) ;
#3932 = CARTESIAN_POINT ( 'NONE',  ( -26.29305231718578995, 48.70000000546238539, 19.10302069950538595 ) ) ;
#3933 = CARTESIAN_POINT ( 'NONE',  ( -32.50000000000000000, 58.40000000546237402, -10.55989012756945300 ) ) ;
#3934 = CARTESIAN_POINT ( 'NONE',  ( -33.58253175000000113, 31.12500000273119127, 0.000000000000000000 ) ) ;
#3935 = CARTESIAN_POINT ( 'NONE',  ( 24.20753774853731244, 30.19010416666665719, -13.97622843553632599 ) ) ;
#3936 = VERTEX_POINT ( 'NONE', #3124 ) ;
#3937 = CARTESIAN_POINT ( 'NONE',  ( -10.37757302488623701, 73.52500000273120406, 31.93888565452638417 ) ) ;
#3938 = CARTESIAN_POINT ( 'NONE',  ( -20.50609665441004736, 32.62500000000000000, -20.50609665440969565 ) ) ;
#3939 = CARTESIAN_POINT ( 'NONE',  ( -34.92499999999992610, 0.000000000000000000, 0.000000000000000000 ) ) ;
#3940 = ORIENTED_EDGE ( 'NONE', *, *, #25677, .T. ) ;
#3941 = CARTESIAN_POINT ( 'NONE',  ( -28.00173670424549499, 54.40142333425730925, -7.543491769121417612 ) ) ;
#3942 = CARTESIAN_POINT ( 'NONE',  ( 20.08610463437157279, 9.800000005462381480, -27.64615127144129758 ) ) ;
#3943 = CARTESIAN_POINT ( 'NONE',  ( 30.02300923189239512, 64.85156249999998579, -2.619432448724977703E-13 ) ) ;
#3944 = CARTESIAN_POINT ( 'NONE',  ( 26.29305231718578995, 57.20000000000000284, -19.10302069950538240 ) ) ;
#3945 = CARTESIAN_POINT ( 'NONE',  ( 6.486482029760649416E-15, 41.87500000273119127, 35.31076352940723240 ) ) ;
#3946 = CARTESIAN_POINT ( 'NONE',  ( -32.50000000000000000, 52.40000000546239534, -10.55989012756945478 ) ) ;
#3947 = CARTESIAN_POINT ( 'NONE',  ( 9.270509831248425314, 80.70000000000000284, 12.75976212528059683 ) ) ;
#3948 = CARTESIAN_POINT ( 'NONE',  ( -27.16883889988624290, 28.92500000273118133, -19.73931689729374028 ) ) ;
#3949 = CARTESIAN_POINT ( 'NONE',  ( -26.29305231718578995, 62.70000000546237118, 19.10302069950538595 ) ) ;
#3950 = CARTESIAN_POINT ( 'NONE',  ( -20.75514604977248823, 57.07500000273117280, -28.56700777964554305 ) ) ;
#3951 = CARTESIAN_POINT ( 'NONE',  ( -10.04305231718578462, 38.40000000000000568, 30.90933677959249337 ) ) ;
#3952 = CARTESIAN_POINT ( 'NONE',  ( 6.277390505771533514E-15, 36.49999999999997868, 34.17252228774368916 ) ) ;
#3953 = CARTESIAN_POINT ( 'NONE',  ( 23.41746825000000243, 10.52499999726880731, 7.608796670333735079 ) ) ;
#3954 =( BOUNDED_CURVE ( )  B_SPLINE_CURVE ( 2, ( #31520, #20899, #103, #31348, #25695, #10594, #2176, #276, #23811, #13338, #8014, #18499, #21241 ),
 .UNSPECIFIED., .F., .T. ) 
 B_SPLINE_CURVE_WITH_KNOTS ( ( 3, 2, 2, 2, 2, 2, 3 ),
 ( 0.05769230769230769551, 0.05897435897435897301, 0.06153846153846154188, 0.06410256410256409687, 0.06666666666666666574, 0.06923076923076923461, 0.07051282051282051211 ),
 .UNSPECIFIED. ) 
 CURVE ( )  GEOMETRIC_REPRESENTATION_ITEM ( )  RATIONAL_B_SPLINE_CURVE ( ( 0.9755282581475768211, 0.9755282581475768211, 1.000000000000000000, 0.9510565162951535312, 1.000000000000000000, 0.9510565162951535312, 1.000000000000000000, 0.9510565162951535312, 1.000000000000000000, 0.9510565162951535312, 1.000000000000000000, 0.9755282581475768211, 0.9755282581475768211 ) ) 
 REPRESENTATION_ITEM ( '' )  );
#3955 = CARTESIAN_POINT ( 'NONE',  ( -27.16883889988623935, 77.32500000273118701, 19.73931689729374739 ) ) ;
#3956 = CARTESIAN_POINT ( 'NONE',  ( 5.147494310547426899, 13.44874571845315536, -32.50000000000000000 ) ) ;
#3957 = CARTESIAN_POINT ( 'NONE',  ( 4.300734207923757602, 80.77500000273118985, -13.23629886949340673 ) ) ;
#3958 = CARTESIAN_POINT ( 'NONE',  ( -33.58253175000000113, 65.37500000273119838, 0.000000000000000000 ) ) ;
#3959 = CARTESIAN_POINT ( 'NONE',  ( -9.270509831248425314, 79.95000000546238539, -12.75976212528059861 ) ) ;
#3960 = CARTESIAN_POINT ( 'NONE',  ( -26.29305231718578995, 40.70000000546236407, 19.10302069950538595 ) ) ;
#3961 = CARTESIAN_POINT ( 'NONE',  ( 19.82091636218621389, 3.949999994537628289, -14.40073868116559197 ) ) ;
#3962 = CARTESIAN_POINT ( 'NONE',  ( 24.22776226481241224, 14.44048583425730925, -13.94119854578936923 ) ) ;
#3963 = CARTESIAN_POINT ( 'NONE',  ( 4.412827539393359662E-15, -59.03347138510255832, 0.000000000000000000 ) ) ;
#3964 = AXIS2_PLACEMENT_3D ( 'NONE', #20628, #30900, #15297 ) ;
#3965 = CARTESIAN_POINT ( 'NONE',  ( -2.162160676586881955E-15, 50.62500000273118417, -35.31076352940723240 ) ) ;
#3966 = CARTESIAN_POINT ( 'NONE',  ( -10.37757302488623701, 1.775000002731188964, 31.93888565452638417 ) ) ;
#3967 = CARTESIAN_POINT ( 'NONE',  ( -27.16883889988624290, 59.17500000273119554, -19.73931689729374028 ) ) ;
#3968 = CARTESIAN_POINT ( 'NONE',  ( 24.20753774853756113, 51.38802083333332860, 13.97622843553589789 ) ) ;
#3969 = CARTESIAN_POINT ( 'NONE',  ( -14.97647472619946285, 37.64361083425730925, -26.02091320914851025 ) ) ;
#3970 = AXIS2_PLACEMENT_3D ( 'NONE', #27710, #1443, #17589 ) ;
#3971 = CARTESIAN_POINT ( 'NONE',  ( -14.97647472619899389, 30.18451416574268720, 26.02091320914878025 ) ) ;
#3972 = CARTESIAN_POINT ( 'NONE',  ( -26.29305231718578995, 64.70000000546237118, 19.10302069950538595 ) ) ;
#3973 = CARTESIAN_POINT ( 'NONE',  ( -11.25946833292375793, 72.67500000273119554, -8.180482586598733619 ) ) ;
#3974 = CARTESIAN_POINT ( 'NONE',  ( -24.22776226481266448, 58.54388916574269075, -13.94119854578892514 ) ) ;
#3975 = CARTESIAN_POINT ( 'NONE',  ( -26.29305231718578995, 54.20000000000000995, 19.10302069950538595 ) ) ;
#3976 = CARTESIAN_POINT ( 'NONE',  ( 10.04305231718579705, 58.59999999999998721, 30.90933677959248982 ) ) ;
#3977 = VERTEX_POINT ( 'NONE', #10259 ) ;
#3978 = CARTESIAN_POINT ( 'NONE',  ( 27.16883889988624290, 44.17500000273118133, 19.73931689729373673 ) ) ;
#3979 = CARTESIAN_POINT ( 'NONE',  ( 18.94512977948575738, 2.924999997268806773, 13.76444248337723408 ) ) ;
#3980 = CARTESIAN_POINT ( 'NONE',  ( 20.08610463437157279, 31.80000000546237260, -27.64615127144129758 ) ) ;
#3981 = ORIENTED_EDGE ( 'NONE', *, *, #24113, .F. ) ;
#3982 = CARTESIAN_POINT ( 'NONE',  ( 20.50609665440969565, 33.48437500000000000, -20.50609665441004736 ) ) ;
#3984 = EDGE_LOOP ( 'NONE', ( #2342, #1598 ) ) ;
#3983 = EDGE_CURVE ( 'NONE', #21770, #2565, #11026, .T. ) ;
#3985 = CARTESIAN_POINT ( 'NONE',  ( -3.880418787951099180, 12.30125427608447097, -24.50000000000001421 ) ) ;
#3986 = CARTESIAN_POINT ( 'NONE',  ( -10.37757302488623701, 51.52500000273118985, 31.93888565452638417 ) ) ;
#3987 = CARTESIAN_POINT ( 'NONE',  ( -2.584737979205441561E-13, 60.55468749999999289, -30.02300923189239512 ) ) ;
#3988 = EDGE_CURVE ( 'NONE', #1219, #27572, #1777, .T. ) ;
#3989 = CARTESIAN_POINT ( 'NONE',  ( 20.08610463437157279, 9.800000005462369046, -27.64615127144129758 ) ) ;
#3990 = CARTESIAN_POINT ( 'NONE',  ( 10.37757302488624767, 65.72500000273119269, 31.93888565452638417 ) ) ;
#3991 = CARTESIAN_POINT ( 'NONE',  ( 23.41746824999999887, 13.12499999726882116, 0.000000000000000000 ) ) ;
#3992 =( BOUNDED_CURVE ( )  B_SPLINE_CURVE ( 2, ( #9251, #9089, #25046, #30019, #3944, #14586, #24872, #32259, #19571, #1527, #4112, #14249, #17333 ),
 .UNSPECIFIED., .F., .F. ) 
 B_SPLINE_CURVE_WITH_KNOTS ( ( 3, 2, 2, 2, 2, 2, 3 ),
 ( 0.2884615384615384914, 0.2897435897435897689, 0.2923076923076923239, 0.2948717948717948789, 0.2974358974358974339, 0.2999999999999999889, 0.3012820512820512664 ),
 .UNSPECIFIED. ) 
 CURVE ( )  GEOMETRIC_REPRESENTATION_ITEM ( )  RATIONAL_B_SPLINE_CURVE ( ( 0.9755282581475768211, 0.9755282581475772652, 1.000000000000000000, 0.9510565162951535312, 1.000000000000000000, 0.9510565162951535312, 1.000000000000000000, 0.9510565162951535312, 1.000000000000000000, 0.9510565162951535312, 1.000000000000000000, 0.9755282581475768211, 0.9755282581475768211 ) ) 
 REPRESENTATION_ITEM ( '' )  );
#3993 = CARTESIAN_POINT ( 'NONE',  ( -2.092463501923844636E-15, 53.50000000000000000, -34.17252228774368916 ) ) ;
#3994 = CARTESIAN_POINT ( 'NONE',  ( -10.37757302488623701, 23.77500000273119340, 31.93888565452638417 ) ) ;
#3995 = CARTESIAN_POINT ( 'NONE',  ( -26.06988505166722803, 16.86420166574268720, 7.025853678916877953 ) ) ;
#3996 = CARTESIAN_POINT ( 'NONE',  ( -8.960552108402742093E-16, 76.37500000273116996, -14.63369212191046387 ) ) ;
#3997 = CARTESIAN_POINT ( 'NONE',  ( 7.570916362186207671, 7.599999999999996092, 23.30088464923126779 ) ) ;
#3998 = CARTESIAN_POINT ( 'NONE',  ( -32.50000000000000000, 33.90000000000000568, -10.55989012756945300 ) ) ;
#3999 = CARTESIAN_POINT ( 'NONE',  ( 32.50000000000000711, 4.900000000000005684, 10.55989012756945122 ) ) ;
#4000 = ORIENTED_EDGE ( 'NONE', *, *, #12601, .T. ) ;
#4001 = CARTESIAN_POINT ( 'NONE',  ( -4.523095164977116484E-15, 6.624999997268815832, 24.62258325217400312 ) ) ;
#4002 = CARTESIAN_POINT ( 'NONE',  ( 5.779280353836490358E-15, 58.49999999999999289, 32.49999999999999289 ) ) ;
#4003 = CARTESIAN_POINT ( 'NONE',  ( -24.20753774853756823, 42.79427083333331439, -13.97622843553588723 ) ) ;
#4004 = CARTESIAN_POINT ( 'NONE',  ( -20.75514604977248823, 68.82500000273118701, -28.56700777964554305 ) ) ;
#4005 = CARTESIAN_POINT ( 'NONE',  ( 10.37757302488624056, 26.77500000273118275, -31.93888565452638417 ) ) ;
#4006 = CARTESIAN_POINT ( 'NONE',  ( 33.58253175000000823, 16.27500000273118630, 10.91162601494192863 ) ) ;
#4007 = CARTESIAN_POINT ( 'NONE',  ( 6.486482029760648627E-15, 11.87500000273118062, 35.31076352940722529 ) ) ;
#4008 = CARTESIAN_POINT ( 'NONE',  ( -28.02196122052045268, 12.86496500092397710, 7.468012846824790607 ) ) ;
#4009 = CARTESIAN_POINT ( 'NONE',  ( -26.00068869287340334, 55.97135416666665719, 15.01150461594643382 ) ) ;
#4010 = CARTESIAN_POINT ( 'NONE',  ( 11.25946833292375793, 76.57500000273120122, -8.180482586598735395 ) ) ;
#4011 = CARTESIAN_POINT ( 'NONE',  ( -26.29305231718578995, 48.20000000000000995, 19.10302069950538595 ) ) ;
#4012 = CARTESIAN_POINT ( 'NONE',  ( 15.14183272437242067, 7.449999994537640724, 20.84094480462498211 ) ) ;
#4013 = CARTESIAN_POINT ( 'NONE',  ( 27.16883889988624290, 51.92500000273120264, 19.73931689729373673 ) ) ;
#4014 = AXIS2_PLACEMENT_3D ( 'NONE', #3352, #26856, #13822 ) ;
#4015 = CARTESIAN_POINT ( 'NONE',  ( 18.94512977948575738, 18.92499999726882010, 13.76444248337723408 ) ) ;
#4016 = VERTEX_POINT ( 'NONE', #20387 ) ;
#4017 = CARTESIAN_POINT ( 'NONE',  ( -33.58253175000000113, 63.47500000273117138, 10.91162601494193929 ) ) ;
#4018 = CARTESIAN_POINT ( 'NONE',  ( -34.92499999999992610, 0.000000000000000000, 16.50000000000002842 ) ) ;
#4019 = CARTESIAN_POINT ( 'NONE',  ( -7.236395654485763274, 10.02499999726880198, 22.27133577429736633 ) ) ;
#4020 = CARTESIAN_POINT ( 'NONE',  ( 0.04044903254993986036, 31.05506916759064495, -27.95245687107223986 ) ) ;
#4021 = ORIENTED_EDGE ( 'NONE', *, *, #28655, .T. ) ;
#4022 = CARTESIAN_POINT ( 'NONE',  ( 20.75514604977249178, 31.82500000273119056, 28.56700777964553950 ) ) ;
#4023 = CARTESIAN_POINT ( 'NONE',  ( 0.000000000000000000, 11.99999999999999645, 0.000000000000000000 ) ) ;
#4024 = ORIENTED_EDGE ( 'NONE', *, *, #25175, .F. ) ;
#4025 = CARTESIAN_POINT ( 'NONE',  ( 15.01150461594643204, 58.54947916666665009, 26.00068869287340334 ) ) ;
#4026 = CARTESIAN_POINT ( 'NONE',  ( -27.16883889988623935, 61.57500000273119412, 19.73931689729374739 ) ) ;
#4027 = CARTESIAN_POINT ( 'NONE',  ( -10.04305231718579172, 36.10000000546237686, -30.90933677959248982 ) ) ;
#4028 = CARTESIAN_POINT ( 'NONE',  ( -2.162160676586881955E-15, 64.62500000273121259, -35.31076352940723240 ) ) ;
#4029 = CARTESIAN_POINT ( 'NONE',  ( 15.01150461594596308, 33.34114583333332860, -26.00068869287367335 ) ) ;
#4030 = CARTESIAN_POINT ( 'NONE',  ( -15.14183272437242600, 5.300000000000006928, 20.84094480462497856 ) ) ;
#4031 = CARTESIAN_POINT ( 'NONE',  ( -33.58253175000000113, 3.375000002731193049, 0.000000000000000000 ) ) ;
#4032 = CARTESIAN_POINT ( 'NONE',  ( 10.37757302488624767, 13.72500000273119092, 31.93888565452638417 ) ) ;
#4033 = CARTESIAN_POINT ( 'NONE',  ( -13.91746824999999887, 72.87500000273119838, 0.000000000000000000 ) ) ;
#4034 = CARTESIAN_POINT ( 'NONE',  ( -28.02196122052058413, 41.21315999907602645, -7.468012846824272799 ) ) ;
#4035 = CARTESIAN_POINT ( 'NONE',  ( 4.635254915624212657, 78.60000000000000853, 14.26584774442730286 ) ) ;
#4036 = CARTESIAN_POINT ( 'NONE',  ( 7.505752307973351023, 55.25520833333333570, 28.01184896238290278 ) ) ;
#4037 = CIRCLE ( 'NONE', #16120, 33.00000000000000000 ) ;
#4038 = CARTESIAN_POINT ( 'NONE',  ( -8.891200544363830713E-16, 73.75000000546239676, -15.00000000000000000 ) ) ;
#4039 = CARTESIAN_POINT ( 'NONE',  ( -24.50000000000000355, 6.649999994537636461, -7.960532557706207157 ) ) ;
#4040 = CARTESIAN_POINT ( 'NONE',  ( -12.13525491562421088, 76.05000000546239391, -8.816778784387096835 ) ) ;
#4041 = CARTESIAN_POINT ( 'NONE',  ( -13.97622843553632421, 15.58072916666666607, -24.20753774853731599 ) ) ;
#4042 = CARTESIAN_POINT ( 'NONE',  ( 33.58253175000000113, 38.12500000273119838, -4.112674001490185761E-15 ) ) ;
#4043 = CARTESIAN_POINT ( 'NONE',  ( 4.300734207923757602, 78.27500000273118985, -13.23629886949340673 ) ) ;
#4044 = CARTESIAN_POINT ( 'NONE',  ( -33.58253175000000113, 51.27500000273118275, -10.91162601494193218 ) ) ;
#4045 = CARTESIAN_POINT ( 'NONE',  ( -20.75514604977248823, 27.07500000273119412, -28.56700777964554305 ) ) ;
#4046 = CARTESIAN_POINT ( 'NONE',  ( 5.779280353836490358E-15, 13.00000000546238077, 32.49999999999999289 ) ) ;
#4047 = CARTESIAN_POINT ( 'NONE',  ( -20.08610463437156923, 8.800000005462370822, 27.64615127144130113 ) ) ;
#4048 = CARTESIAN_POINT ( 'NONE',  ( 4.635254915624209993, 81.40000000000000568, -14.26584774442730463 ) ) ;
#4049 = CARTESIAN_POINT ( 'NONE',  ( -32.50000000000000000, 66.10000000000000853, 10.55989012756946366 ) ) ;
#4050 = CARTESIAN_POINT ( 'NONE',  ( 1.507698388325705758E-15, 11.12499999726881761, -24.62258325217400312 ) ) ;
#4051 = CARTESIAN_POINT ( 'NONE',  ( -0.04044903255044120238, 24.74180583240935505, -30.02300923189239867 ) ) ;
#4052 =( BOUNDED_CURVE ( )  B_SPLINE_CURVE ( 2, ( #15406, #31347, #30656, #25862, #2529, #7326, #33231, #26035, #28097, #12997, #4585, #17810, #33765 ),
 .UNSPECIFIED., .F., .F. ) 
 B_SPLINE_CURVE_WITH_KNOTS ( ( 3, 2, 2, 2, 2, 2, 3 ),
 ( 0.2500000000000000000, 0.2555555555555555358, 0.2666666666666666630, 0.2777777777777777901, 0.2888888888888888618, 0.2999999999999999889, 0.3055555555555555802 ),
 .UNSPECIFIED. ) 
 CURVE ( )  GEOMETRIC_REPRESENTATION_ITEM ( )  RATIONAL_B_SPLINE_CURVE ( ( 0.9755282581475768211, 0.9755282581475768211, 1.000000000000000000, 0.9510565162951535312, 1.000000000000000000, 0.9510565162951535312, 1.000000000000000000, 0.9510565162951535312, 1.000000000000000000, 0.9510565162951535312, 1.000000000000000000, 0.9755282581475765991, 0.9755282581475767101 ) ) 
 REPRESENTATION_ITEM ( '' )  );
#4053 = CARTESIAN_POINT ( 'NONE',  ( -7.236395654485763274, 4.524999997268825069, 22.27133577429736633 ) ) ;
#4054 = CARTESIAN_POINT ( 'NONE',  ( 7.025853678916867295, 36.62982666574267654, 26.06988505166722803 ) ) ;
#4055 = DIRECTION ( 'NONE',  ( 0.000000000000000000, -1.000000000000000000, 0.000000000000000000 ) ) ;
#4056 =( BOUNDED_CURVE ( )  B_SPLINE_CURVE ( 2, ( #17762, #28392, #2482, #18283, #15363, #13117, #18451, #31473, #13285, #33716, #15536, #20693, #21192 ),
 .UNSPECIFIED., .F., .T. ) 
 B_SPLINE_CURVE_WITH_KNOTS ( ( 3, 2, 2, 2, 2, 2, 3 ),
 ( 0.2756410256410256610, 0.2769230769230769384, 0.2794871794871794934, 0.2820512820512820484, 0.2846153846153846034, 0.2871794871794871584, 0.2884615384615384914 ),
 .UNSPECIFIED. ) 
 CURVE ( )  GEOMETRIC_REPRESENTATION_ITEM ( )  RATIONAL_B_SPLINE_CURVE ( ( 0.9755282581475768211, 0.9755282581475768211, 1.000000000000000000, 0.9510565162951535312, 1.000000000000000000, 0.9510565162951535312, 1.000000000000000000, 0.9510565162951535312, 1.000000000000000000, 0.9510565162951535312, 1.000000000000000000, 0.9755282581475762660, 0.9755282581475768211 ) ) 
 REPRESENTATION_ITEM ( '' )  );
#4057 = CARTESIAN_POINT ( 'NONE',  ( -27.16883889988623935, 13.32500000273117990, 19.73931689729374739 ) ) ;
#4058 = CARTESIAN_POINT ( 'NONE',  ( -7.236395654485763274, 14.52499999726880553, 22.27133577429736633 ) ) ;
#4059 = AXIS2_PLACEMENT_3D ( 'NONE', #26318, #5213, #24087 ) ;
#4060 = CARTESIAN_POINT ( 'NONE',  ( 6.988114217768294445, 62.13020833333334281, 26.07999730980477437 ) ) ;
#4061 = EDGE_LOOP ( 'NONE', ( #30369, #639, #13546, #15509 ) ) ;
#4062 = CARTESIAN_POINT ( 'NONE',  ( -33.58253175000000113, 51.02500000273119696, -10.91162601494193218 ) ) ;
#4063 = CARTESIAN_POINT ( 'NONE',  ( -33.58253175000000113, 21.27500000273117209, -10.91162601494193218 ) ) ;
#4064 = VERTEX_POINT ( 'NONE', #31183 ) ;
#4065 = CARTESIAN_POINT ( 'NONE',  ( 26.00068869287367335, 37.63802083333331439, 15.01150461594596308 ) ) ;
#4066 = CARTESIAN_POINT ( 'NONE',  ( 25.98046417659858420, 35.63840250092398065, 15.04653450569292872 ) ) ;
#4067 = CARTESIAN_POINT ( 'NONE',  ( -5.147494310547430452, 9.551254281546839309, -32.49999999999999289 ) ) ;
#4068 = CARTESIAN_POINT ( 'NONE',  ( -7.570916362186215665, 19.14999999453761959, 23.30088464923126423 ) ) ;
#4069 = CARTESIAN_POINT ( 'NONE',  ( 18.94512977948575738, 6.424999997268809437, 13.76444248337723408 ) ) ;
#4070 = CARTESIAN_POINT ( 'NONE',  ( -27.16883889988624290, 21.17500000273120264, -19.73931689729374028 ) ) ;
#4071 = CARTESIAN_POINT ( 'NONE',  ( -26.29305231718578995, 24.70000000546238184, 19.10302069950538595 ) ) ;
#4072 = CARTESIAN_POINT ( 'NONE',  ( -32.50000000000000000, 71.89999999999999147, -10.55989012756945478 ) ) ;
#4073 = CARTESIAN_POINT ( 'NONE',  ( 0.000000000000000000, 80.00000000000001421, -32.50000000000000000 ) ) ;
#4074 = CARTESIAN_POINT ( 'NONE',  ( -2.762933978968158399, 73.99999999999998579, 13.97530310184241031 ) ) ;
#4075 = CARTESIAN_POINT ( 'NONE',  ( -28.02196122052045268, 57.55246500092398065, 7.468012846824790607 ) ) ;
#4076 = CARTESIAN_POINT ( 'NONE',  ( -33.58253175000000113, 39.37500000273119838, 0.000000000000000000 ) ) ;
#4077 = CARTESIAN_POINT ( 'NONE',  ( -20.75514604977248823, 56.82500000273118701, -28.56700777964554305 ) ) ;
#4078 = CARTESIAN_POINT ( 'NONE',  ( -15.01150461594595775, 35.05989583333332860, 26.00068869287368756 ) ) ;
#4079 = CARTESIAN_POINT ( 'NONE',  ( 0.000000000000000000, 0.000000000000000000, 0.000000000000000000 ) ) ;
#4080 = CARTESIAN_POINT ( 'NONE',  ( -23.41746824999999887, 10.12499999726881938, -2.867812753649727150E-15 ) ) ;
#4081 = CARTESIAN_POINT ( 'NONE',  ( -2.092463501923844636E-15, 17.50000000000000000, -34.17252228774368916 ) ) ;
#4082 = AXIS2_PLACEMENT_3D ( 'NONE', #2181, #7159, #12654 ) ;
#4083 = CARTESIAN_POINT ( 'NONE',  ( 24.50000000000000355, 17.89999999999998437, 7.960532557706212486 ) ) ;
#4084 = CARTESIAN_POINT ( 'NONE',  ( -24.22776226481266448, 41.35638916574269075, -13.94119854578892514 ) ) ;
#4085 = CARTESIAN_POINT ( 'NONE',  ( 10.37757302488624056, 56.52500000273119696, -31.93888565452638417 ) ) ;
#4086 = CARTESIAN_POINT ( 'NONE',  ( 33.58253175000000113, 50.47500000273118559, -10.91162601494193574 ) ) ;
#4087 = CARTESIAN_POINT ( 'NONE',  ( -23.41746824999999887, 13.52499999726880198, -7.608796670333730638 ) ) ;
#4088 = DIRECTION ( 'NONE',  ( 1.000000000000000000, 0.000000000000000000, 0.000000000000000000 ) ) ;
#4089 = CARTESIAN_POINT ( 'NONE',  ( -33.58253175000000113, 1.125000002731191273, 0.000000000000000000 ) ) ;
#4090 = CARTESIAN_POINT ( 'NONE',  ( 24.22776226481241224, 48.81548583425731636, -13.94119854578936923 ) ) ;
#4091 = CARTESIAN_POINT ( 'NONE',  ( -1.756012107511856980E-14, 4.249999994537631665, -24.50000000000000000 ) ) ;
#4092 = CARTESIAN_POINT ( 'NONE',  ( -31.78768264672014610, 52.00000000000002842, 7.374898305514709484 ) ) ;
#4093 = CARTESIAN_POINT ( 'NONE',  ( 6.486482029760649416E-15, 21.62500000273119483, 35.31076352940723240 ) ) ;
#4094 = FACE_BOUND ( 'NONE', #92, .T. ) ;
#4095 = CARTESIAN_POINT ( 'NONE',  ( -15.00000000000000000, 78.15000000546238823, -4.873795443493594171 ) ) ;
#4096 = CARTESIAN_POINT ( 'NONE',  ( -10.04305231718579172, 78.10000000546237686, -30.90933677959248982 ) ) ;
#4097 = CARTESIAN_POINT ( 'NONE',  ( -30.02300923189239867, 65.13243083240935505, 0.04044903255044988294 ) ) ;
#4098 = CARTESIAN_POINT ( 'NONE',  ( 32.50000000000000000, 43.60000000546237686, -10.55989012756945833 ) ) ;
#4099 = CARTESIAN_POINT ( 'NONE',  ( 12.13525491562420910, 71.45000000546237118, -8.816778784387098611 ) ) ;
#4100 = CARTESIAN_POINT ( 'NONE',  ( 27.16883889988623935, 30.32500000273119412, -19.73931689729374384 ) ) ;
#4101 = CARTESIAN_POINT ( 'NONE',  ( -33.58253175000000113, 65.37500000273119838, 0.000000000000000000 ) ) ;
#4102 = CARTESIAN_POINT ( 'NONE',  ( -19.09188309203694445, 32.62500000000000000, -19.09188309203661049 ) ) ;
#4103 = ORIENTED_EDGE ( 'NONE', *, *, #8318, .T. ) ;
#4104 = CARTESIAN_POINT ( 'NONE',  ( 33.58253175000000113, 66.22500000273120691, -10.91162601494193751 ) ) ;
#4105 = CARTESIAN_POINT ( 'NONE',  ( -2.584737979205441561E-13, 43.36718749999999289, -30.02300923189239512 ) ) ;
#4106 = CIRCLE ( 'NONE', #23308, 24.50000000000000000 ) ;
#4107 = CARTESIAN_POINT ( 'NONE',  ( 0.000000000000000000, 80.00000000000001421, -30.50000000000000000 ) ) ;
#4108 = ORIENTED_EDGE ( 'NONE', *, *, #9396, .T. ) ;
#4109 = CARTESIAN_POINT ( 'NONE',  ( 20.53372385742072481, 48.67225666759065206, -20.47846945139902175 ) ) ;
#4110 = CARTESIAN_POINT ( 'NONE',  ( -32.50000000000000000, 10.50000000546237544, 0.000000000000000000 ) ) ;
#4111 = CARTESIAN_POINT ( 'NONE',  ( 7.505752307973351023, 65.56770833333332860, 28.01184896238290278 ) ) ;
#4112 = CARTESIAN_POINT ( 'NONE',  ( 10.04305231718579705, 56.59999999999998010, 30.90933677959248982 ) ) ;
#4113 = CARTESIAN_POINT ( 'NONE',  ( 20.75514604977249178, 42.07500000273117990, 28.56700777964553950 ) ) ;
#4114 = CARTESIAN_POINT ( 'NONE',  ( 32.50000000000000000, 45.50000000546239676, -3.980102097228898626E-15 ) ) ;
#4115 = ADVANCED_FACE ( 'NONE', ( #25533 ), #20043, .T. ) ;
#4116 = CARTESIAN_POINT ( 'NONE',  ( 12.13525491562421088, 80.79999999999998295, 8.816778784387095058 ) ) ;
#4117 = CARTESIAN_POINT ( 'NONE',  ( 33.58253175000000113, 28.22500000273119269, -10.91162601494193751 ) ) ;
#4118 = CARTESIAN_POINT ( 'NONE',  ( 32.50000000000000000, 31.50000000546238255, -3.980102097228898626E-15 ) ) ;
#4119 = CARTESIAN_POINT ( 'NONE',  ( -20.75514604977248823, 55.07500000273117990, -28.56700777964554305 ) ) ;
#4120 = SURFACE_SIDE_STYLE ('',( #14092 ) ) ;
#4121 = CARTESIAN_POINT ( 'NONE',  ( 20.08610463437157279, 33.29999999999999716, -27.64615127144129758 ) ) ;
#4122 = CARTESIAN_POINT ( 'NONE',  ( 10.04305231718578817, 33.39999999999998437, -30.90933677959249337 ) ) ;
#4123 = CARTESIAN_POINT ( 'NONE',  ( 24.50000000000000000, 0.000000000000000000, 0.000000000000000000 ) ) ;
#4124 = CARTESIAN_POINT ( 'NONE',  ( -33.58253175000000113, 77.12500000273119838, 0.000000000000000000 ) ) ;
#4125 = CARTESIAN_POINT ( 'NONE',  ( -14.41072458151355917, 67.00000000000004263, 29.41684567868815492 ) ) ;
#4126 = DIRECTION ( 'NONE',  ( -0.000000000000000000, 1.000000000000000000, -0.000000000000000000 ) ) ;
#4127 = CARTESIAN_POINT ( 'NONE',  ( 20.75514604977248467, 68.67500000273119554, -28.56700777964554305 ) ) ;
#4128 = CARTESIAN_POINT ( 'NONE',  ( -15.00000000000000000, 74.25000000546239676, 0.000000000000000000 ) ) ;
#4129 = ADVANCED_FACE ( 'NONE', ( #33586 ), #12134, .T. ) ;
#4130 = ORIENTED_EDGE ( 'NONE', *, *, #27703, .T. ) ;
#4131 = CARTESIAN_POINT ( 'NONE',  ( 24.50000000000000000, 3.749999994537622783, 0.000000000000000000 ) ) ;
#4132 = CARTESIAN_POINT ( 'NONE',  ( 0.04044903254993986036, 17.30506916759064140, -27.95245687107223986 ) ) ;
#4133 = CARTESIAN_POINT ( 'NONE',  ( -10.58590195883389207, 74.00000000000001421, -10.62726115788808201 ) ) ;
#4134 = CARTESIAN_POINT ( 'NONE',  ( -27.16883889988623935, 39.32500000273118701, 19.73931689729374739 ) ) ;
#4135 = CARTESIAN_POINT ( 'NONE',  ( -2.162160676586881955E-15, 6.875000002731180615, -35.31076352940723240 ) ) ;
#4136 = CARTESIAN_POINT ( 'NONE',  ( -20.75514604977248112, 55.67500000273119554, 28.56700777964554661 ) ) ;
#4137 = CARTESIAN_POINT ( 'NONE',  ( -6.988114217767819270, 55.54166666666667140, 26.07999730980490583 ) ) ;
#4138 = CARTESIAN_POINT ( 'NONE',  ( 28.02196122052045268, 42.08371500092398065, -7.468012846824774620 ) ) ;
#4139 = CARTESIAN_POINT ( 'NONE',  ( 20.47846945139867003, 38.92149333240934794, -20.53372385742107653 ) ) ;
#4140 = CARTESIAN_POINT ( 'NONE',  ( -20.08610463437157989, 64.20000000546238539, -27.64615127144129758 ) ) ;
#4141 = CARTESIAN_POINT ( 'NONE',  ( -4.300734207923755825, 71.27500000273117564, 13.23629886949340673 ) ) ;
#4142 = AXIS2_PLACEMENT_3D ( 'NONE', #5531, #31269, #10853 ) ;
#4143 = CARTESIAN_POINT ( 'NONE',  ( -14.01125832528328985, 55.39284749907604066, -24.18731323226223040 ) ) ;
#4144 = VECTOR ( 'NONE', #9708, 1000.000000000000114 ) ;
#4145 = DIRECTION ( 'NONE',  ( -0.000000000000000000, 1.000000000000000000, -0.000000000000000000 ) ) ;
#4146 = DIRECTION ( 'NONE',  ( 0.000000000000000000, 0.000000000000000000, -1.000000000000000000 ) ) ;
#4147 = CARTESIAN_POINT ( 'NONE',  ( -27.16883889988624290, 43.17500000273118133, -19.73931689729374028 ) ) ;
#4148 = CARTESIAN_POINT ( 'NONE',  ( 7.236395654485760609, 1.524999997268822183, -22.27133577429736633 ) ) ;
#4149 = ORIENTED_EDGE ( 'NONE', *, *, #20550, .T. ) ;
#4150 = CARTESIAN_POINT ( 'NONE',  ( -20.08610463437156923, 30.80000000546237615, 27.64615127144130113 ) ) ;
#4151 = ORIENTED_EDGE ( 'NONE', *, *, #17536, .T. ) ;
#4152 = CARTESIAN_POINT ( 'NONE',  ( -7.505752307972844761, 31.47916666666666075, 28.01184896238304134 ) ) ;
#4153 = ORIENTED_EDGE ( 'NONE', *, *, #30398, .F. ) ;
#4154 =( BOUNDED_CURVE ( )  B_SPLINE_CURVE ( 2, ( #30771, #32823, #17576, #20322, #17927, #4522, #28035, #14997, #9314, #17232, #4183, #15173, #33347 ),
 .UNSPECIFIED., .F., .T. ) 
 B_SPLINE_CURVE_WITH_KNOTS ( ( 3, 2, 2, 2, 2, 2, 3 ),
 ( 0.9807692307692307265, 0.9820512820512820040, 0.9846153846153846700, 0.9871794871794872250, 0.9897435897435897800, 0.9923076923076923350, 0.9935897435897436125 ),
 .UNSPECIFIED. ) 
 CURVE ( )  GEOMETRIC_REPRESENTATION_ITEM ( )  RATIONAL_B_SPLINE_CURVE ( ( 0.9755282581475768211, 0.9755282581475768211, 1.000000000000000000, 0.9510565162951535312, 1.000000000000000000, 0.9510565162951535312, 1.000000000000000000, 0.9510565162951535312, 1.000000000000000000, 0.9510565162951535312, 1.000000000000000000, 0.9755282581475768211, 0.9755282581475768211 ) ) 
 REPRESENTATION_ITEM ( '' )  );
#4155 = CARTESIAN_POINT ( 'NONE',  ( -20.08610463437157989, 74.20000000546238539, -27.64615127144129758 ) ) ;
#4156 = CARTESIAN_POINT ( 'NONE',  ( -27.16883889988624290, 46.92500000273119554, -19.73931689729374028 ) ) ;
#4157 = FACE_OUTER_BOUND ( 'NONE', #5601, .T. ) ;
#4158 = CARTESIAN_POINT ( 'NONE',  ( -10.04305231718578462, 48.39999999999999858, 30.90933677959249337 ) ) ;
#4159 = CARTESIAN_POINT ( 'NONE',  ( 20.08610463437158344, 11.20000000546238184, 27.64615127144129403 ) ) ;
#4160 = CARTESIAN_POINT ( 'NONE',  ( -26.29305231718579350, 7.800000000000001599, -19.10302069950537884 ) ) ;
#4161 = CARTESIAN_POINT ( 'NONE',  ( 23.41746824999999887, 17.12499999726882649, 0.000000000000000000 ) ) ;
#4162 = CARTESIAN_POINT ( 'NONE',  ( 26.29305231718579350, 50.80000000000001137, 19.10302069950537529 ) ) ;
#4163 = CARTESIAN_POINT ( 'NONE',  ( 6.001560367445586717E-15, 1.500000000000005995, 24.50000000000000000 ) ) ;
#4164 = CARTESIAN_POINT ( 'NONE',  ( 33.58253175000000113, 20.47500000273120335, -10.91162601494193751 ) ) ;
#4165 = CIRCLE ( 'NONE', #8553, 26.50000000000000355 ) ;
#4166 = CARTESIAN_POINT ( 'NONE',  ( 12.13525491562420910, 77.19999999999998863, -8.816778784387098611 ) ) ;
#4167 = CARTESIAN_POINT ( 'NONE',  ( -14.01125832528328985, 24.45534749907602290, -24.18731323226223040 ) ) ;
#4168 = CARTESIAN_POINT ( 'NONE',  ( 13.91746824999999887, 73.87500000273116996, -1.704398294459741270E-15 ) ) ;
#4169 = DIRECTION ( 'NONE',  ( -0.2588190451025238481, -0.9659258262890674240, 3.169619151431803768E-17 ) ) ;
#4170 = DIRECTION ( 'NONE',  ( 0.000000000000000000, 1.000000000000000000, 0.000000000000000000 ) ) ;
#4171 = CARTESIAN_POINT ( 'NONE',  ( -20.08610463437157989, 3.699999999999999289, -27.64615127144129758 ) ) ;
#4172 = VERTEX_POINT ( 'NONE', #17814 ) ;
#4173 = CARTESIAN_POINT ( 'NONE',  ( 18.94512977948576093, 5.324999997268820451, -13.76444248337722875 ) ) ;
#4174 = LINE ( 'NONE', #24764, #12905 ) ;
#4175 = CARTESIAN_POINT ( 'NONE',  ( -26.07999730980490583, 42.65104166666666430, -6.988114217767815717 ) ) ;
#4176 = CARTESIAN_POINT ( 'NONE',  ( 10.37757302488624767, 65.72500000273119269, 31.93888565452638417 ) ) ;
#4177 = CARTESIAN_POINT ( 'NONE',  ( 33.58253175000000113, 24.37500000273119838, -4.112674001490185761E-15 ) ) ;
#4178 = CARTESIAN_POINT ( 'NONE',  ( -27.16883889988624290, 7.175000002731176885, -19.73931689729374028 ) ) ;
#4179 = CARTESIAN_POINT ( 'NONE',  ( -10.37757302488623701, 7.775000002731180970, 31.93888565452638417 ) ) ;
#4180 = CARTESIAN_POINT ( 'NONE',  ( -0.04044903254990864921, 15.58631916759064495, 30.02300923189239867 ) ) ;
#4181 = CARTESIAN_POINT ( 'NONE',  ( 2.740863092043355209E-13, 51.96093750000000000, 30.02300923189239512 ) ) ;
#4182 = ADVANCED_FACE ( 'NONE', ( #10087 ), #21553, .F. ) ;
#4183 = CARTESIAN_POINT ( 'NONE',  ( 10.04305231718579705, 2.599999999999991207, 30.90933677959248982 ) ) ;
#4184 = CARTESIAN_POINT ( 'NONE',  ( -20.08610463437157989, 47.70000000000000995, -27.64615127144129758 ) ) ;
#4185 = CARTESIAN_POINT ( 'NONE',  ( -33.58253175000000113, 53.22500000273118559, 10.91162601494193929 ) ) ;
#4186 = EDGE_CURVE ( 'NONE', #726, #12058, #12315, .T. ) ;
#4187 = CARTESIAN_POINT ( 'NONE',  ( 18.94512977948575738, 2.424999997268806329, 13.76444248337723408 ) ) ;
#4188 = VERTEX_POINT ( 'NONE', #2664 ) ;
#4189 = CARTESIAN_POINT ( 'NONE',  ( 10.37757302488624056, 60.77500000273118275, -31.93888565452638417 ) ) ;
#4190 = CARTESIAN_POINT ( 'NONE',  ( 0.000000000000000000, 80.00000000000001421, -32.50000000000000000 ) ) ;
#4191 = CARTESIAN_POINT ( 'NONE',  ( 23.41746825000000243, 12.52499999726880375, 7.608796670333735079 ) ) ;
#4192 = CARTESIAN_POINT ( 'NONE',  ( 26.06988505166735592, 32.05767333425730214, 7.025853678916393896 ) ) ;
#4193 = ORIENTED_EDGE ( 'NONE', *, *, #24339, .T. ) ;
#4194 = CARTESIAN_POINT ( 'NONE',  ( -33.58253175000000113, 29.02500000273119340, -10.91162601494193218 ) ) ;
#4196 = FACE_OUTER_BOUND ( 'NONE', #4510, .T. ) ;
#4195 = VECTOR ( 'NONE', #28780, 1000.000000000000000 ) ;
#4197 = VERTEX_POINT ( 'NONE', #13474 ) ;
#4198 = CARTESIAN_POINT ( 'NONE',  ( -20.50609665440969209, 62.70312500000000000, 20.50609665441005092 ) ) ;
#4199 = CARTESIAN_POINT ( 'NONE',  ( -27.16883889988623935, 63.57500000273119412, 19.73931689729374739 ) ) ;
#4200 = CARTESIAN_POINT ( 'NONE',  ( 27.16883889988624290, 69.92500000273119554, 19.73931689729373673 ) ) ;
#4201 = CARTESIAN_POINT ( 'NONE',  ( -28.01184896238290278, 28.61458333333333215, 7.505752307973363457 ) ) ;
#4202 = CARTESIAN_POINT ( 'NONE',  ( -24.50000000000001066, 11.09999999999999964, 7.960532557706201828 ) ) ;
#4203 = CARTESIAN_POINT ( 'NONE',  ( 10.37757302488624767, 5.975000002731184701, 31.93888565452638417 ) ) ;
#4204 = CARTESIAN_POINT ( 'NONE',  ( 20.75514604977248467, 12.42500000273119554, -28.56700777964554305 ) ) ;
#4205 = CARTESIAN_POINT ( 'NONE',  ( -8.960552108402744065E-16, 72.37500000273118417, -14.63369212191046209 ) ) ;
#4206 = CARTESIAN_POINT ( 'NONE',  ( -28.00173670424535644, 54.67670166574269075, 7.543491769121936308 ) ) ;
#4207 = CARTESIAN_POINT ( 'NONE',  ( 12.13525491562420910, 73.19999999999998863, -8.816778784387098611 ) ) ;
#4208 = CARTESIAN_POINT ( 'NONE',  ( 28.01184896238304134, 54.68229166666665719, 7.505752307972846538 ) ) ;
#4209 = CARTESIAN_POINT ( 'NONE',  ( 20.08610463437158344, 19.20000000546235697, 27.64615127144129403 ) ) ;
#4210 = CARTESIAN_POINT ( 'NONE',  ( 10.04305231718579705, 22.60000000000000853, 30.90933677959248982 ) ) ;
#4211 = CARTESIAN_POINT ( 'NONE',  ( 19.82091636218621034, 5.549999994537619052, 14.40073868116559730 ) ) ;
#4212 = CARTESIAN_POINT ( 'NONE',  ( 4.635254915624212657, 78.85000000546239107, 14.26584774442730286 ) ) ;
#4213 = CARTESIAN_POINT ( 'NONE',  ( -27.95245687107222921, 15.00781249999999467, 2.498001805406602216E-13 ) ) ;
#4214 = CARTESIAN_POINT ( 'NONE',  ( -10.37757302488624411, 40.72500000273118559, -31.93888565452638417 ) ) ;
#4215 = CARTESIAN_POINT ( 'NONE',  ( -11.25946833292375793, 72.67500000273119554, -8.180482586598733619 ) ) ;
#4216 = CARTESIAN_POINT ( 'NONE',  ( 10.37757302488624056, 40.77500000273119696, -31.93888565452638417 ) ) ;
#4217 = CARTESIAN_POINT ( 'NONE',  ( 10.37757302488624767, 27.97500000273117493, 31.93888565452638417 ) ) ;
#4218 = CARTESIAN_POINT ( 'NONE',  ( -19.82091636218621034, 16.54999999453762882, -14.40073868116559552 ) ) ;
#4219 = CARTESIAN_POINT ( 'NONE',  ( -7.570916362186210335, 14.34999999453762065, -23.30088464923126779 ) ) ;
#4220 = ADVANCED_FACE ( 'NONE', ( #16054 ), #3001, .T. ) ;
#4221 = DIRECTION ( 'NONE',  ( -1.224646799147353454E-16, 1.000000000000000000, -0.000000000000000000 ) ) ;
#4222 = CARTESIAN_POINT ( 'NONE',  ( -32.50000000000000000, 67.89999999999996305, -10.55989012756945478 ) ) ;
#4223 = CARTESIAN_POINT ( 'NONE',  ( 18.94512977948576093, 8.824999997268822227, -13.76444248337722875 ) ) ;
#4224 = CARTESIAN_POINT ( 'NONE',  ( -28.02196122052058413, 24.02565999907602290, -7.468012846824272799 ) ) ;
#4225 = EDGE_CURVE ( 'NONE', #31336, #21272, #22844, .T. ) ;
#4226 = CARTESIAN_POINT ( 'NONE',  ( -4.223320258572819786E-15, 11.24999999453762456, 24.50000000000000000 ) ) ;
#4227 = CARTESIAN_POINT ( 'NONE',  ( 14.01125832528330051, 36.48659749907601935, 24.18731323226221974 ) ) ;
#4228 = CARTESIAN_POINT ( 'NONE',  ( 33.58253175000000823, 12.02500000273117742, 10.91162601494192685 ) ) ;
#4229 = CARTESIAN_POINT ( 'NONE',  ( -18.94512977948575738, 11.92499999726881477, -13.76444248337723231 ) ) ;
#4230 = CARTESIAN_POINT ( 'NONE',  ( -24.20753774853756823, 66.85677083333334281, -13.97622843553588723 ) ) ;
#4231 = VERTEX_POINT ( 'NONE', #21200 ) ;
#4232 = CARTESIAN_POINT ( 'NONE',  ( 6.486482029760649416E-15, 49.62500000273117706, 35.31076352940723240 ) ) ;
#4233 = CARTESIAN_POINT ( 'NONE',  ( 33.58253175000000113, 24.37500000273119838, -4.112674001490185761E-15 ) ) ;
#4234 = VERTEX_POINT ( 'NONE', #13124 ) ;
#4235 = CARTESIAN_POINT ( 'NONE',  ( 30.02300923189239512, 33.91406249999997158, -2.619432448724977703E-13 ) ) ;
#4236 = CARTESIAN_POINT ( 'NONE',  ( -20.53372385742071771, 33.20350666759063074, 20.47846945139902530 ) ) ;
#4237 = CARTESIAN_POINT ( 'NONE',  ( 5.779280353836490358E-15, 60.49999999999998579, 32.49999999999999289 ) ) ;
#4238 = CARTESIAN_POINT ( 'NONE',  ( 24.50000000000000355, 15.64999999453761426, 7.960532557706212486 ) ) ;
#4239 = CARTESIAN_POINT ( 'NONE',  ( -23.41746824999999887, 13.62499999726882116, -2.867812753649727150E-15 ) ) ;
#4240 = CARTESIAN_POINT ( 'NONE',  ( 10.37757302488624767, 19.97500000273119625, 31.93888565452638417 ) ) ;
#4241 = CARTESIAN_POINT ( 'NONE',  ( -32.50000000000000000, 22.40000000546237402, -10.55989012756945478 ) ) ;
#4242 = CARTESIAN_POINT ( 'NONE',  ( -2.092463501923844636E-15, 69.49999999999997158, -34.17252228774368916 ) ) ;
#4243 = DIRECTION ( 'NONE',  ( 0.000000000000000000, 0.000000000000000000, -1.000000000000000000 ) ) ;
#4244 = CARTESIAN_POINT ( 'NONE',  ( 6.054684311146244891E-15, -72.44024934668307480, 0.000000000000000000 ) ) ;
#4245 = CARTESIAN_POINT ( 'NONE',  ( 20.53372385742072481, 52.10975666759065206, -20.47846945139902175 ) ) ;
#4246 = CARTESIAN_POINT ( 'NONE',  ( -20.75514604977248823, 35.07500000273120833, -28.56700777964554305 ) ) ;
#4247 = CARTESIAN_POINT ( 'NONE',  ( 10.37757302488624767, 53.72500000273118559, 31.93888565452638417 ) ) ;
#4248 = CARTESIAN_POINT ( 'NONE',  ( 20.50609665440969565, 33.48437500000000000, -20.50609665441004736 ) ) ;
#4249 = CARTESIAN_POINT ( 'NONE',  ( -7.236395654485763274, 12.52499999726880375, 22.27133577429736633 ) ) ;
#4250 = CARTESIAN_POINT ( 'NONE',  ( 10.04305231718578817, 13.39999999999999503, -30.90933677959249337 ) ) ;
#4251 = CARTESIAN_POINT ( 'NONE',  ( -19.82091636218621389, 17.19999999999999218, 14.40073868116558842 ) ) ;
#4252 = CARTESIAN_POINT ( 'NONE',  ( 19.06425588902558133, 45.79649333240935505, -19.11951029504797006 ) ) ;
#4253 = CARTESIAN_POINT ( 'NONE',  ( -27.16883889988624290, 54.92500000273120264, -19.73931689729374028 ) ) ;
#4254 = CARTESIAN_POINT ( 'NONE',  ( 20.75514604977248467, 48.67500000273118133, -28.56700777964554305 ) ) ;
#4255 =( BOUNDED_CURVE ( )  B_SPLINE_CURVE ( 2, ( #25567, #31216, #7709, #30525, #23160, #7023, #33623, #9771, #22990, #25393, #33449, #10122, #12348 ),
 .UNSPECIFIED., .F., .T. ) 
 B_SPLINE_CURVE_WITH_KNOTS ( ( 3, 2, 2, 2, 2, 2, 3 ),
 ( 0.05000000000000000278, 0.05999999999999999778, 0.08000000000000000167, 0.1000000000000000056, 0.1199999999999999956, 0.1400000000000000133, 0.1500000000000000222 ),
 .UNSPECIFIED. ) 
 CURVE ( )  GEOMETRIC_REPRESENTATION_ITEM ( )  RATIONAL_B_SPLINE_CURVE ( ( 0.9755282581475768211, 0.9755282581475768211, 1.000000000000000000, 0.9510565162951535312, 1.000000000000000000, 0.9510565162951535312, 1.000000000000000000, 0.9510565162951535312, 1.000000000000000000, 0.9510565162951535312, 1.000000000000000000, 0.9755282581475767101, 0.9755282581475768211 ) ) 
 REPRESENTATION_ITEM ( '' )  );
#4256 = CARTESIAN_POINT ( 'NONE',  ( 1.507698388325705758E-15, 15.12499999726880873, -24.62258325217400312 ) ) ;
#4257 = CARTESIAN_POINT ( 'NONE',  ( 3.980102097228898626E-15, 80.00000000000001421, 32.50000000000000000 ) ) ;
#4258 = CARTESIAN_POINT ( 'NONE',  ( -33.58253175000000113, 1.225000002731198467, 10.91162601494193929 ) ) ;
#4259 = CARTESIAN_POINT ( 'NONE',  ( -26.09010956794232428, 47.23996500092398065, 6.950374756619732253 ) ) ;
#4260 = CARTESIAN_POINT ( 'NONE',  ( 23.12028783339972549, 16.99999999999998934, 3.796702233379605662 ) ) ;
#4261 = CARTESIAN_POINT ( 'NONE',  ( -30.93003301939250704, 52.00000000000002842, 10.64619209630807006 ) ) ;
#4262 = CARTESIAN_POINT ( 'NONE',  ( -20.75514604977248112, 23.42500000273119909, 28.56700777964554661 ) ) ;
#4263 = CARTESIAN_POINT ( 'NONE',  ( 26.29305231718578995, 67.19999999999998863, -19.10302069950538240 ) ) ;
#4264 = CARTESIAN_POINT ( 'NONE',  ( 10.04305231718578817, 53.39999999999999147, -30.90933677959249337 ) ) ;
#4265 = DIRECTION ( 'NONE',  ( -0.000000000000000000, -1.000000000000000000, -0.000000000000000000 ) ) ;
#4266 = CARTESIAN_POINT ( 'NONE',  ( 7.468012846824281681, 66.13503499907601224, -28.02196122052058058 ) ) ;
#4267 = CARTESIAN_POINT ( 'NONE',  ( 10.04305231718579705, 43.10000000546236265, 30.90933677959248982 ) ) ;
#4268 = CARTESIAN_POINT ( 'NONE',  ( 32.50000000000000000, 35.10000000000000142, -10.55989012756945833 ) ) ;
#4269 = CARTESIAN_POINT ( 'NONE',  ( 6.486482029760648627E-15, 31.62500000273119838, 35.31076352940722529 ) ) ;
#4270 = CARTESIAN_POINT ( 'NONE',  ( 10.37757302488624767, 63.97500000273120691, 31.93888565452638417 ) ) ;
#4271 = CARTESIAN_POINT ( 'NONE',  ( 13.97622843553633665, 37.92447916666666430, 24.20753774853730889 ) ) ;
#4272 = ORIENTED_EDGE ( 'NONE', *, *, #423, .T. ) ;
#4273 = CARTESIAN_POINT ( 'NONE',  ( -20.75514604977248112, 67.42500000273118133, 28.56700777964554661 ) ) ;
#4274 = CARTESIAN_POINT ( 'NONE',  ( 28.01184896238304134, 44.36979166666666430, 7.505752307972846538 ) ) ;
#4275 = CARTESIAN_POINT ( 'NONE',  ( -2.165007332552593587E-13, 52.50000000000000711, 32.50000000000000000 ) ) ;
#4276 = ORIENTED_EDGE ( 'NONE', *, *, #9547, .F. ) ;
#4277 = CARTESIAN_POINT ( 'NONE',  ( -14.97647472619946285, 58.26861083425732346, -26.02091320914851025 ) ) ;
#4278 = CARTESIAN_POINT ( 'NONE',  ( -26.06988505166735237, 64.71392333425730214, -7.025853678916388567 ) ) ;
#4279 = CARTESIAN_POINT ( 'NONE',  ( 10.37757302488624056, 14.52500000273120051, -31.93888565452638417 ) ) ;
#4280 = CARTESIAN_POINT ( 'NONE',  ( 2.740863092043355209E-13, 62.27343749999999289, 30.02300923189239512 ) ) ;
#4281 = PLANE ( 'NONE',  #6435 ) ;
#4282 = CARTESIAN_POINT ( 'NONE',  ( -20.75514604977248112, 43.67500000273119554, 28.56700777964554661 ) ) ;
#4283 = CARTESIAN_POINT ( 'NONE',  ( 32.50000000000000000, 45.60000000546236265, -10.55989012756945833 ) ) ;
#4284 = CARTESIAN_POINT ( 'NONE',  ( 4.300734207923761154, 73.97500000273122112, 13.23629886949340495 ) ) ;
#4285 = CARTESIAN_POINT ( 'NONE',  ( -33.58253175000000113, 31.22500000273118559, 10.91162601494193929 ) ) ;
#4286 = CARTESIAN_POINT ( 'NONE',  ( 24.50000000000000000, 0.8749999972688105032, 0.000000000000000000 ) ) ;
#4287 = CARTESIAN_POINT ( 'NONE',  ( -33.58253175000000113, 55.37500000273118417, 0.000000000000000000 ) ) ;
#4288 = CARTESIAN_POINT ( 'NONE',  ( -20.08610463437156923, 38.29999999999997584, 27.64615127144130113 ) ) ;
#4289 = CARTESIAN_POINT ( 'NONE',  ( -20.08610463437156923, 32.29999999999999716, 27.64615127144130113 ) ) ;
#4290 = CARTESIAN_POINT ( 'NONE',  ( 19.82091636218621389, 2.200000000000007283, -14.40073868116559197 ) ) ;
#4291 = CARTESIAN_POINT ( 'NONE',  ( -20.75514604977248112, 73.42500000273118133, 28.56700777964554661 ) ) ;
#4292 = CARTESIAN_POINT ( 'NONE',  ( 32.50000000000000711, 62.89999999999998437, 10.55989012756945122 ) ) ;
#4293 = CARTESIAN_POINT ( 'NONE',  ( -4.300734207923755825, 75.77500000273118985, 13.23629886949340673 ) ) ;
#4294 = CARTESIAN_POINT ( 'NONE',  ( -27.16883889988623935, 69.57500000273120122, 19.73931689729374739 ) ) ;
#4295 = CARTESIAN_POINT ( 'NONE',  ( -9.270509831248425314, 75.95000000546238539, -12.75976212528059861 ) ) ;
#4296 = VERTEX_POINT ( 'NONE', #18291 ) ;
#4297 = CARTESIAN_POINT ( 'NONE',  ( -33.58253175000000113, 21.12500000273118062, 0.000000000000000000 ) ) ;
#4298 = CARTESIAN_POINT ( 'NONE',  ( -24.50000000000000355, 12.64999999453762136, -7.960532557706207157 ) ) ;
#4299 = CARTESIAN_POINT ( 'NONE',  ( -26.06988505166735237, 16.58892333425730570, -7.025853678916388567 ) ) ;
#4300 = CARTESIAN_POINT ( 'NONE',  ( 3.980102097228898626E-15, 80.00000000000001421, 32.50000000000000000 ) ) ;
#4301 = CARTESIAN_POINT ( 'NONE',  ( 33.58253175000000113, 42.12500000273118417, -4.112674001490185761E-15 ) ) ;
#4302 = CARTESIAN_POINT ( 'NONE',  ( -2.162160676586881955E-15, 2.875000002731189941, -35.31076352940723240 ) ) ;
#4303 = CARTESIAN_POINT ( 'NONE',  ( 20.75514604977248467, 56.67500000273119554, -28.56700777964554305 ) ) ;
#4304 = CARTESIAN_POINT ( 'NONE',  ( -7.543491769121417612, 46.66704833425730925, 28.00173670424549499 ) ) ;
#4305 = CARTESIAN_POINT ( 'NONE',  ( 30.02300923189239867, 39.35118083240935505, -0.04044903255044467877 ) ) ;
#4306 = CARTESIAN_POINT ( 'NONE',  ( -32.50000000000000000, 60.40000000546236691, -10.55989012756945478 ) ) ;
#4307 = CARTESIAN_POINT ( 'NONE',  ( 13.91746824999999532, 80.47500000273119269, -4.522059556121118540 ) ) ;
#4308 = CARTESIAN_POINT ( 'NONE',  ( -7.025853678916861966, 65.84857666574268364, -26.06988505166722803 ) ) ;
#4309 = CARTESIAN_POINT ( 'NONE',  ( -32.50000000000000000, 54.00000000000000711, 0.000000000000000000 ) ) ;
#4310 = EDGE_CURVE ( 'NONE', #24744, #25078, #23939, .T. ) ;
#4311 = CARTESIAN_POINT ( 'NONE',  ( 6.277390505771533514E-15, 75.00000000546238255, 34.17252228774368916 ) ) ;
#4312 = PLANE ( 'NONE',  #30523 ) ;
#4313 = CARTESIAN_POINT ( 'NONE',  ( 33.58253175000000113, 38.47500000273118559, -10.91162601494193751 ) ) ;
#4314 = CARTESIAN_POINT ( 'NONE',  ( -1.089172066684569321E-14, 78.50000000000000000, 15.00000000000000000 ) ) ;
#4315 = ORIENTED_EDGE ( 'NONE', *, *, #7894, .F. ) ;
#4316 = CARTESIAN_POINT ( 'NONE',  ( -10.37757302488624411, 76.97500000273119269, -31.93888565452638417 ) ) ;
#4317 = CARTESIAN_POINT ( 'NONE',  ( 20.08610463437158344, 29.20000000546237118, 27.64615127144129403 ) ) ;
#4318 = ORIENTED_EDGE ( 'NONE', *, *, #15607, .T. ) ;
#4319 = EDGE_CURVE ( 'NONE', #13996, #23373, #26358, .T. ) ;
#4320 = CARTESIAN_POINT ( 'NONE',  ( 7.505752307973351023, 34.63020833333332860, 28.01184896238290278 ) ) ;
#4321 = CARTESIAN_POINT ( 'NONE',  ( 6.277390505771533514E-15, 63.00000000546238255, 34.17252228774368916 ) ) ;
#4322 = ORIENTED_EDGE ( 'NONE', *, *, #20163, .T. ) ;
#4323 = CARTESIAN_POINT ( 'NONE',  ( -5.147494310547430452, 55.55125428154683220, -32.49999999999999289 ) ) ;
#4324 = CARTESIAN_POINT ( 'NONE',  ( 6.486482029760649416E-15, 51.62500000273120548, 35.31076352940723240 ) ) ;
#4325 = CARTESIAN_POINT ( 'NONE',  ( 14.47279130897151589, 16.32499999726879736, 19.92008829642072953 ) ) ;
#4326 = CARTESIAN_POINT ( 'NONE',  ( -28.01184896238290278, 62.98958333333332149, 7.505752307973363457 ) ) ;
#4327 = CARTESIAN_POINT ( 'NONE',  ( -26.29305231718579350, 4.300000005462378816, -19.10302069950537884 ) ) ;
#4328 = ADVANCED_FACE ( 'NONE', ( #5232 ), #9914, .F. ) ;
#4329 = CARTESIAN_POINT ( 'NONE',  ( -27.16883889988624290, 64.92500000273119554, -19.73931689729374028 ) ) ;
#4330 = CARTESIAN_POINT ( 'NONE',  ( -2.584737979205442066E-13, 12.42968749999999822, -30.02300923189239867 ) ) ;
#4331 = CARTESIAN_POINT ( 'NONE',  ( 10.04305231718578817, 51.39999999999999858, -30.90933677959249337 ) ) ;
#4332 = CARTESIAN_POINT ( 'NONE',  ( 19.82091636218621389, 2.200000000000007283, -14.40073868116559197 ) ) ;
#4333 = CARTESIAN_POINT ( 'NONE',  ( -20.75514604977248112, 15.67500000273117600, 28.56700777964554661 ) ) ;
#4334 = DIRECTION ( 'NONE',  ( -0.000000000000000000, 1.000000000000000000, -0.000000000000000000 ) ) ;
#4335 = CARTESIAN_POINT ( 'NONE',  ( 7.025853678916867295, 22.87982666574268720, 26.06988505166722803 ) ) ;
#4336 = CARTESIAN_POINT ( 'NONE',  ( 11.25946833292375793, 75.67500000273119554, 8.180482586598731842 ) ) ;
#4337 = CARTESIAN_POINT ( 'NONE',  ( 7.313012447739250820E-14, 13.24999999453762456, 24.50000000000000000 ) ) ;
#4338 = CARTESIAN_POINT ( 'NONE',  ( -32.50000000000000000, 3.899999999999992806, -10.55989012756945478 ) ) ;
#4339 = VERTEX_POINT ( 'NONE', #20056 ) ;
#4340 = CARTESIAN_POINT ( 'NONE',  ( 1.507698388325705758E-15, 5.624999997268818497, -24.62258325217400312 ) ) ;
#4341 = CARTESIAN_POINT ( 'NONE',  ( -8.601468415847515203, 71.17500000273115290, 11.83890561707634959 ) ) ;
#4342 = CARTESIAN_POINT ( 'NONE',  ( -26.07999730980490583, 46.08854166666666430, -6.988114217767815717 ) ) ;
#4343 = CARTESIAN_POINT ( 'NONE',  ( -33.58253175000000113, 59.22500000273119269, 10.91162601494193929 ) ) ;
#4344 = CARTESIAN_POINT ( 'NONE',  ( 27.16883889988624290, 24.17500000273119198, 19.73931689729373673 ) ) ;
#4345 = CARTESIAN_POINT ( 'NONE',  ( 33.58253175000000823, 10.27500000273117564, 10.91162601494192863 ) ) ;
#4346 = CARTESIAN_POINT ( 'NONE',  ( -33.58253175000000113, 5.375000002731167292, 0.000000000000000000 ) ) ;
#4347 = CARTESIAN_POINT ( 'NONE',  ( 0.04044903254992426173, 20.74256916759064495, -30.02300923189239867 ) ) ;
#4348 = CARTESIAN_POINT ( 'NONE',  ( -20.50609665440969209, 66.14062500000000000, 20.50609665441005092 ) ) ;
#4349 = CARTESIAN_POINT ( 'NONE',  ( 20.08610463437157279, 77.80000000546237970, -27.64615127144129758 ) ) ;
#4350 = CARTESIAN_POINT ( 'NONE',  ( -4.300734207923759378, 72.97500000273119269, -13.23629886949340495 ) ) ;
#4351 = CARTESIAN_POINT ( 'NONE',  ( 20.08610463437158344, 42.69999999999998863, 27.64615127144129403 ) ) ;
#4352 = CARTESIAN_POINT ( 'NONE',  ( -33.58253175000000113, 43.22500000273118559, 10.91162601494193929 ) ) ;
#4353 = CARTESIAN_POINT ( 'NONE',  ( -14.47279130897151589, 1.324999997268808238, -19.92008829642072598 ) ) ;
#4354 = PRODUCT_DEFINITION_SHAPE ( 'NONE', 'NONE',  #33990 ) ;
#4355 = CARTESIAN_POINT ( 'NONE',  ( -13.97622843553588901, 65.99739583333332860, 24.20753774853756823 ) ) ;
#4356 = ORIENTED_EDGE ( 'NONE', *, *, #7565, .T. ) ;
#4357 = CARTESIAN_POINT ( 'NONE',  ( 6.486482029760649416E-15, 57.87500000273117706, 35.31076352940723240 ) ) ;
#4358 =( BOUNDED_CURVE ( )  B_SPLINE_CURVE ( 2, ( #8438, #27307, #8609, #14105, #9108, #8771, #19254, #24562, #24727, #16850, #27137, #6372, #1035 ),
 .UNSPECIFIED., .F., .T. ) 
 B_SPLINE_CURVE_WITH_KNOTS ( ( 3, 2, 2, 2, 2, 2, 3 ),
 ( 0.6500000000000000222, 0.6600000000000000311, 0.6800000000000000488, 0.6999999999999999556, 0.7199999999999999734, 0.7399999999999999911, 0.7500000000000000000 ),
 .UNSPECIFIED. ) 
 CURVE ( )  GEOMETRIC_REPRESENTATION_ITEM ( )  RATIONAL_B_SPLINE_CURVE ( ( 0.9755282581475768211, 0.9755282581475768211, 1.000000000000000000, 0.9510565162951535312, 1.000000000000000000, 0.9510565162951535312, 1.000000000000000000, 0.9510565162951535312, 1.000000000000000000, 0.9510565162951535312, 1.000000000000000000, 0.9755282581475768211, 0.9755282581475768211 ) ) 
 REPRESENTATION_ITEM ( '' )  );
#4359 = DIRECTION ( 'NONE',  ( -1.000000000000000000, 0.000000000000000000, 0.000000000000000000 ) ) ;
#4360 = CARTESIAN_POINT ( 'NONE',  ( -18.94512977948576093, 11.82499999726882578, 13.76444248337722698 ) ) ;
#4361 = CARTESIAN_POINT ( 'NONE',  ( 26.09010956794232428, 31.77121500092397000, -6.950374756619718042 ) ) ;
#4362 = ORIENTED_EDGE ( 'NONE', *, *, #28129, .F. ) ;
#4363 = CARTESIAN_POINT ( 'NONE',  ( -20.75514604977248112, 29.42500000273118133, 28.56700777964554661 ) ) ;
#4364 = CARTESIAN_POINT ( 'NONE',  ( 2.445080149700053643E-15, 74.49999999999998579, 15.00000000000000000 ) ) ;
#4365 = ORIENTED_EDGE ( 'NONE', *, *, #17881, .F. ) ;
#4366 = CARTESIAN_POINT ( 'NONE',  ( 0.000000000000000000, 80.00000000000001421, 0.000000000000000000 ) ) ;
#4367 = CARTESIAN_POINT ( 'NONE',  ( -27.16883889988623935, 69.32500000273117280, 19.73931689729374739 ) ) ;
#4368 = CARTESIAN_POINT ( 'NONE',  ( -30.02300923189239512, 42.50781249999997868, 2.654126918244515359E-13 ) ) ;
#4369 = CARTESIAN_POINT ( 'NONE',  ( -24.50000000000000000, 11.00000000000001066, -3.000384657911015469E-15 ) ) ;
#4370 = CARTESIAN_POINT ( 'NONE',  ( -20.75514604977248823, 3.075000002731198112, -28.56700777964554305 ) ) ;
#4371 = EDGE_CURVE ( 'NONE', #23252, #29590, #22967, .T. ) ;
#4372 = CARTESIAN_POINT ( 'NONE',  ( 10.37757302488624056, 10.52500000273118275, -31.93888565452638417 ) ) ;
#4373 = DIRECTION ( 'NONE',  ( -1.000000000000000000, 0.000000000000000000, 0.000000000000000000 ) ) ;
#4374 = CARTESIAN_POINT ( 'NONE',  ( -26.02091320914878025, 51.66888916574269075, -14.97647472619899389 ) ) ;
#4375 = CARTESIAN_POINT ( 'NONE',  ( 2.897257156509938333E-15, 74.50000000000000000, 15.77193336357400710 ) ) ;
#4376 = CARTESIAN_POINT ( 'NONE',  ( -2.584737979205442066E-13, 60.55468749999998579, -30.02300923189239867 ) ) ;
#4377 = CARTESIAN_POINT ( 'NONE',  ( -1.778240108872766143E-15, 20.00000000546237544, -32.49999999999999289 ) ) ;
#4378 = CARTESIAN_POINT ( 'NONE',  ( 15.14183272437241889, 3.449999994537620296, 20.84094480462498211 ) ) ;
#4379 = CARTESIAN_POINT ( 'NONE',  ( -9.270509831248425314, 79.95000000546235697, -12.75976212528059861 ) ) ;
#4380 = CARTESIAN_POINT ( 'NONE',  ( 26.07999730980490227, 27.18229166666666430, 6.988114217767821046 ) ) ;
#4381 = CARTESIAN_POINT ( 'NONE',  ( -33.58253175000000113, 37.22500000273119980, 10.91162601494193929 ) ) ;
#4382 = CARTESIAN_POINT ( 'NONE',  ( 33.58253175000000113, 78.22500000273119269, -10.91162601494193751 ) ) ;
#4383 = CARTESIAN_POINT ( 'NONE',  ( -10.37757302488623701, 39.77500000273119696, 31.93888565452638417 ) ) ;
#4384 = CARTESIAN_POINT ( 'NONE',  ( -10.37757302488624411, 24.97500000273117493, -31.93888565452638417 ) ) ;
#4385 = CARTESIAN_POINT ( 'NONE',  ( 20.08610463437158344, 40.69999999999999574, 27.64615127144129403 ) ) ;
#4386 = APPLICATION_CONTEXT ( 'automotive_design' ) ;
#4387 = CARTESIAN_POINT ( 'NONE',  ( -15.14183272437242778, 15.04999999453763238, 20.84094480462497856 ) ) ;
#4388 = CARTESIAN_POINT ( 'NONE',  ( 10.04305231718579705, 32.59999999999998721, 30.90933677959248982 ) ) ;
#4389 = CARTESIAN_POINT ( 'NONE',  ( 6.277390505771533514E-15, 64.50000000000000000, 34.17252228774368916 ) ) ;
#4390 = CARTESIAN_POINT ( 'NONE',  ( -23.41746825000000243, 11.72499999726882969, 7.608796670333725309 ) ) ;
#4391 = CARTESIAN_POINT ( 'NONE',  ( 7.468012846824281681, 28.32253499907601579, -28.02196122052058058 ) ) ;
#4392 = CARTESIAN_POINT ( 'NONE',  ( 6.988114217768294445, 20.88020833333333215, 26.07999730980477437 ) ) ;
#4393 = CARTESIAN_POINT ( 'NONE',  ( 23.41746825000000243, 3.224999997268806151, -7.608796670333727974 ) ) ;
#4394 = CARTESIAN_POINT ( 'NONE',  ( 19.06425588902558133, 35.48399333240935505, -19.11951029504797006 ) ) ;
#4395 = CARTESIAN_POINT ( 'NONE',  ( -33.58253175000000113, 77.37500000273118417, 0.000000000000000000 ) ) ;
#4396 = CARTESIAN_POINT ( 'NONE',  ( 10.37757302488624767, 15.72500000273119269, 31.93888565452638417 ) ) ;
#4397 = CARTESIAN_POINT ( 'NONE',  ( -18.94512977948576093, 10.32499999726882400, 13.76444248337722698 ) ) ;
#4398 = CARTESIAN_POINT ( 'NONE',  ( -13.97622843553632421, 63.70572916666667140, -24.20753774853731599 ) ) ;
#4399 = VERTEX_POINT ( 'NONE', #27772 ) ;
#4400 = CARTESIAN_POINT ( 'NONE',  ( -27.16883889988623935, 51.32500000273120122, 19.73931689729374739 ) ) ;
#4401 = CARTESIAN_POINT ( 'NONE',  ( -10.37757302488623701, 21.77500000273117919, 31.93888565452638417 ) ) ;
#4402 = ORIENTED_EDGE ( 'NONE', *, *, #17994, .F. ) ;
#4403 = CARTESIAN_POINT ( 'NONE',  ( -26.00068869287368756, 29.04427083333332504, -15.01150461594595775 ) ) ;
#4404 = CARTESIAN_POINT ( 'NONE',  ( -15.04653450569291984, 33.06027750092398776, 25.98046417659859486 ) ) ;
#4405 = CARTESIAN_POINT ( 'NONE',  ( -3.880418787951124493, 9.198745712990794132, 24.50000000000000355 ) ) ;
#4406 = CARTESIAN_POINT ( 'NONE',  ( 1.507698388325705758E-15, 1.624999997268798735, -24.62258325217400312 ) ) ;
#4407 = CARTESIAN_POINT ( 'NONE',  ( -4.523095164977116484E-15, 12.12499999726881406, 24.62258325217400312 ) ) ;
#4408 = CARTESIAN_POINT ( 'NONE',  ( 20.75514604977248467, 22.67500000273119198, -28.56700777964554305 ) ) ;
#4409 = CARTESIAN_POINT ( 'NONE',  ( 26.29305231718578995, 27.70000000546238184, -19.10302069950538240 ) ) ;
#4410 = EDGE_CURVE ( 'NONE', #13108, #17050, #12146, .T. ) ;
#4411 = CARTESIAN_POINT ( 'NONE',  ( 32.50000000000000000, 67.10000000000000853, -10.55989012756945833 ) ) ;
#4412 = CARTESIAN_POINT ( 'NONE',  ( 23.41746824999999887, 0.6249999972688102812, 0.000000000000000000 ) ) ;
#4413 = CARTESIAN_POINT ( 'NONE',  ( 26.29305231718579350, 66.80000000000001137, 19.10302069950537529 ) ) ;
#4414 = CARTESIAN_POINT ( 'NONE',  ( 14.97647472619947351, 63.42486083425730925, 26.02091320914850314 ) ) ;
#4415 = CARTESIAN_POINT ( 'NONE',  ( 33.58253175000000113, 34.47500000273119980, -10.91162601494193751 ) ) ;
#4416 = CARTESIAN_POINT ( 'NONE',  ( -4.300734207923755825, 79.77500000273118985, 13.23629886949340673 ) ) ;
#4417 = CARTESIAN_POINT ( 'NONE',  ( 26.00068869287367690, 30.76302083333332860, 15.01150461594596486 ) ) ;
#4418 = EDGE_CURVE ( 'NONE', #7411, #6369, #6462, .T. ) ;
#4419 = CARTESIAN_POINT ( 'NONE',  ( 23.41746825000000243, 19.02499999726880375, 7.608796670333735079 ) ) ;
#4420 = CARTESIAN_POINT ( 'NONE',  ( 10.04305231718578817, 9.399999999999991473, -30.90933677959249337 ) ) ;
#4421 = CARTESIAN_POINT ( 'NONE',  ( -7.570916362186215665, 17.39999999999999858, 23.30088464923126423 ) ) ;
#4422 = CARTESIAN_POINT ( 'NONE',  ( 19.06425588902558133, 52.67149333240935505, -19.11951029504797006 ) ) ;
#4423 = CARTESIAN_POINT ( 'NONE',  ( -20.75514604977248823, 58.82500000273117990, -28.56700777964554305 ) ) ;
#4424 = CARTESIAN_POINT ( 'NONE',  ( 20.75514604977249178, 64.07500000273120122, 28.56700777964553950 ) ) ;
#4425 = CARTESIAN_POINT ( 'NONE',  ( 27.16883889988624290, 42.17500000273119554, 19.73931689729373673 ) ) ;
#4426 = CARTESIAN_POINT ( 'NONE',  ( 18.94512977948576093, 16.82499999726880091, -13.76444248337722875 ) ) ;
#4427 = LINE ( 'NONE', #12145, #21596 ) ;
#4428 = CARTESIAN_POINT ( 'NONE',  ( 33.58253175000000823, 2.025000002731202287, 10.91162601494192863 ) ) ;
#4429 = CARTESIAN_POINT ( 'NONE',  ( -24.22776226481240514, 50.53423583425731636, 13.94119854578937812 ) ) ;
#4430 = LINE ( 'NONE', #17313, #13313 ) ;
#4431 = CARTESIAN_POINT ( 'NONE',  ( -20.75514604977248112, 19.42500000273117777, 28.56700777964554661 ) ) ;
#4432 = CARTESIAN_POINT ( 'NONE',  ( 32.50000000000000711, 66.90000000000001990, 10.55989012756945122 ) ) ;
#4433 = CARTESIAN_POINT ( 'NONE',  ( 32.50000000000000711, 55.40000000546238113, 10.55989012756945122 ) ) ;
#4434 = DIRECTION ( 'NONE',  ( -0.000000000000000000, -1.000000000000000000, -0.000000000000000000 ) ) ;
#4435 = CARTESIAN_POINT ( 'NONE',  ( 28.02196122052058413, 63.55690999907603356, 7.468012846824272799 ) ) ;
#4436 = CARTESIAN_POINT ( 'NONE',  ( -10.04305231718578462, 42.90000000546238823, 30.90933677959249337 ) ) ;
#4437 = CARTESIAN_POINT ( 'NONE',  ( 2.445080149700053643E-15, 70.75000000546236834, 15.00000000000000000 ) ) ;
#4438 = CARTESIAN_POINT ( 'NONE',  ( -33.58253175000000113, 33.02500000273118275, -10.91162601494193041 ) ) ;
#4439 = CARTESIAN_POINT ( 'NONE',  ( -27.95245687107222921, 39.07031249999997868, 2.498001805406602216E-13 ) ) ;
#4440 = VERTEX_POINT ( 'NONE', #14732 ) ;
#4441 = CARTESIAN_POINT ( 'NONE',  ( -10.37757302488624411, 66.72500000273116427, -31.93888565452638417 ) ) ;
#4442 = CARTESIAN_POINT ( 'NONE',  ( -2.584737979205441561E-13, 36.49218750000000000, -30.02300923189239512 ) ) ;
#4443 = DIRECTION ( 'NONE',  ( 0.000000000000000000, 0.000000000000000000, 1.000000000000000000 ) ) ;
#4444 = ORIENTED_EDGE ( 'NONE', *, *, #1940, .T. ) ;
#4445 = CARTESIAN_POINT ( 'NONE',  ( -20.53372385742071771, 60.70350666759063785, 20.47846945139902530 ) ) ;
#4446 = CARTESIAN_POINT ( 'NONE',  ( -14.01125832528285109, 60.56027750092398065, 24.18731323226248264 ) ) ;
#4447 = CARTESIAN_POINT ( 'NONE',  ( 10.37757302488624056, 12.52500000273119873, -31.93888565452638417 ) ) ;
#4448 = CARTESIAN_POINT ( 'NONE',  ( 26.02091320914876960, 15.57513916574268720, 14.97647472619900455 ) ) ;
#4449 = PLANE ( 'NONE',  #17391 ) ;
#4450 = CARTESIAN_POINT ( 'NONE',  ( 33.58253175000000113, 38.37500000273119838, -4.112674001490185761E-15 ) ) ;
#4451 = AXIS2_PLACEMENT_3D ( 'NONE', #8093, #11012, #21482 ) ;
#4452 = CARTESIAN_POINT ( 'NONE',  ( 32.50000000000000000, 43.60000000546237686, -10.55989012756945833 ) ) ;
#4453 = CARTESIAN_POINT ( 'NONE',  ( -12.13525491562420910, 76.19999999999998863, 8.816778784387098611 ) ) ;
#4454 = CARTESIAN_POINT ( 'NONE',  ( -33.58253175000000113, 29.02500000273119340, -10.91162601494193218 ) ) ;
#4455 = CARTESIAN_POINT ( 'NONE',  ( -5.147494310547430452, 23.55125428154684286, -32.49999999999999289 ) ) ;
#4456 = CARTESIAN_POINT ( 'NONE',  ( 27.16883889988623935, 56.57500000273118701, -19.73931689729374384 ) ) ;
#4457 = EDGE_CURVE ( 'NONE', #21929, #17393, #8466, .T. ) ;
#4458 = CARTESIAN_POINT ( 'NONE',  ( 32.50000000000000000, 27.00000000000001066, -3.980102097228898626E-15 ) ) ;
#4459 = ADVANCED_FACE ( 'NONE', ( #3922 ), #12325, .T. ) ;
#4460 = CARTESIAN_POINT ( 'NONE',  ( 20.08610463437157279, 33.29999999999999716, -27.64615127144129758 ) ) ;
#4461 = CARTESIAN_POINT ( 'NONE',  ( 18.94512977948575738, 18.42499999726882010, 13.76444248337723408 ) ) ;
#4462 = CARTESIAN_POINT ( 'NONE',  ( 20.75514604977248467, 74.42500000273119554, -28.56700777964554305 ) ) ;
#4463 = CARTESIAN_POINT ( 'NONE',  ( -19.64450058003837185, 66.99999999999998579, 26.34187928026369718 ) ) ;
#4464 = AXIS2_PLACEMENT_3D ( 'NONE', #29115, #5619, #16103 ) ;
#4465 = VECTOR ( 'NONE', #17075, 1000.000000000000000 ) ;
#4466 = CARTESIAN_POINT ( 'NONE',  ( -13.91746824999999887, 75.37500000273116996, 0.000000000000000000 ) ) ;
#4467 = CARTESIAN_POINT ( 'NONE',  ( -10.37757302488623701, 65.77500000273117564, 31.93888565452638417 ) ) ;
#4468 = CARTESIAN_POINT ( 'NONE',  ( -15.00000000000000000, 76.35000000546239107, 4.873795443493597723 ) ) ;
#4469 = EDGE_LOOP ( 'NONE', ( #23792, #1908 ) ) ;
#4470 = CARTESIAN_POINT ( 'NONE',  ( -2.162160676586881955E-15, 20.62500000273119483, -35.31076352940723240 ) ) ;
#4471 = CARTESIAN_POINT ( 'NONE',  ( -24.50000000000000000, 8.749999994537628112, -3.000384657911015469E-15 ) ) ;
#4472 = CARTESIAN_POINT ( 'NONE',  ( -19.11951029504763611, 19.45350666759063785, 19.06425588902592239 ) ) ;
#4473 = CARTESIAN_POINT ( 'NONE',  ( -5.147494310547430452, 25.55125428154685352, -32.49999999999999289 ) ) ;
#4474 = CARTESIAN_POINT ( 'NONE',  ( 27.16883889988623935, 38.32500000273118701, -19.73931689729374384 ) ) ;
#4475 = CARTESIAN_POINT ( 'NONE',  ( -10.37757302488624411, 4.975000002731183812, -31.93888565452638417 ) ) ;
#4476 = CARTESIAN_POINT ( 'NONE',  ( 33.58253175000000823, 56.27500000273117564, 10.91162601494192685 ) ) ;
#4477 = CARTESIAN_POINT ( 'NONE',  ( -20.53372385742071771, 46.95350666759064495, 20.47846945139902530 ) ) ;
#4478 = CARTESIAN_POINT ( 'NONE',  ( 7.570916362186207671, 15.60000000000000320, 23.30088464923126779 ) ) ;
#4479 = CARTESIAN_POINT ( 'NONE',  ( -20.53372385742107653, 38.06211833240934084, -20.47846945139867003 ) ) ;
#4480 = CARTESIAN_POINT ( 'NONE',  ( 32.50000000000000000, 59.60000000546236976, -10.55989012756945833 ) ) ;
#4481 = CARTESIAN_POINT ( 'NONE',  ( -13.91746824999999532, 72.97500000273120691, 4.522059556121122093 ) ) ;
#4482 = CARTESIAN_POINT ( 'NONE',  ( 19.11951029504797006, 60.40586833240935505, 19.06425588902558133 ) ) ;
#4483 = DIRECTION ( 'NONE',  ( -1.000000000000000000, 0.000000000000000000, 0.000000000000000000 ) ) ;
#4484 = CARTESIAN_POINT ( 'NONE',  ( 32.50000000000000711, 77.40000000546240244, 10.55989012756945122 ) ) ;
#4485 = CARTESIAN_POINT ( 'NONE',  ( -20.50609665441004736, 15.43749999999999645, -20.50609665440969565 ) ) ;
#4486 = CARTESIAN_POINT ( 'NONE',  ( -10.37757302488623701, 35.77500000273118985, 31.93888565452638417 ) ) ;
#4487 = CARTESIAN_POINT ( 'NONE',  ( 18.94512977948576093, 5.324999997268820451, -13.76444248337722875 ) ) ;
#4488 = ORIENTED_EDGE ( 'NONE', *, *, #25226, .T. ) ;
#4489 = CARTESIAN_POINT ( 'NONE',  ( 20.75514604977248467, 74.67500000273118133, -28.56700777964554305 ) ) ;
#4490 = CARTESIAN_POINT ( 'NONE',  ( -32.50000000000000000, 24.60000000546236620, 10.55989012756946366 ) ) ;
#4491 = CARTESIAN_POINT ( 'NONE',  ( -26.00068869287340334, 42.22135416666666430, 15.01150461594643382 ) ) ;
#4492 = CARTESIAN_POINT ( 'NONE',  ( -20.08610463437156923, 62.80000000546237970, 27.64615127144130113 ) ) ;
#4493 = VERTEX_POINT ( 'NONE', #11814 ) ;
#4494 = CARTESIAN_POINT ( 'NONE',  ( -32.50000000000000000, 56.10000000000000142, 10.55989012756946366 ) ) ;
#4495 = CARTESIAN_POINT ( 'NONE',  ( -27.16883889988624290, 48.92500000273120264, -19.73931689729374028 ) ) ;
#4496 = CARTESIAN_POINT ( 'NONE',  ( 23.41746825000000243, 16.52499999726882152, 7.608796670333735079 ) ) ;
#4497 = CARTESIAN_POINT ( 'NONE',  ( 26.29305231718578995, 7.700000005462392494, -19.10302069950538240 ) ) ;
#4498 = CARTESIAN_POINT ( 'NONE',  ( -27.16883889988624290, 66.92500000273119554, -19.73931689729374028 ) ) ;
#4499 = DIRECTION ( 'NONE',  ( -0.000000000000000000, -1.000000000000000000, -0.000000000000000000 ) ) ;
#4500 = CARTESIAN_POINT ( 'NONE',  ( 26.29305231718579350, 54.80000000000001847, 19.10302069950537529 ) ) ;
#4501 = CARTESIAN_POINT ( 'NONE',  ( 23.41746825000000243, 0.7249999972688272454, -7.608796670333727974 ) ) ;
#4502 = CARTESIAN_POINT ( 'NONE',  ( 20.75514604977249178, 20.07500000273118346, 28.56700777964553950 ) ) ;
#4503 = VECTOR ( 'NONE', #4606, 1000.000000000000000 ) ;
#4504 = LINE ( 'NONE', #9477, #18959 ) ;
#4505 = CARTESIAN_POINT ( 'NONE',  ( 7.025853678916867295, 29.75482666574269075, 26.06988505166722803 ) ) ;
#4506 = CARTESIAN_POINT ( 'NONE',  ( -8.601468415847518756, 81.07500000273120122, -11.83890561707634781 ) ) ;
#4507 = CARTESIAN_POINT ( 'NONE',  ( -13.38432950954956624, -58.51673569255127205, 0.000000000000000000 ) ) ;
#4508 = CARTESIAN_POINT ( 'NONE',  ( 15.31642273298461632, -59.03347138510255832, 1.875720807433735970E-15 ) ) ;
#4509 = CARTESIAN_POINT ( 'NONE',  ( -10.04305231718578462, 4.400000000000001243, 30.90933677959249337 ) ) ;
#4510 = EDGE_LOOP ( 'NONE', ( #15697, #18450, #22380, #31090 ) ) ;
#4511 = CARTESIAN_POINT ( 'NONE',  ( 18.94512977948575738, 10.92499999726881299, 13.76444248337723408 ) ) ;
#4512 = CYLINDRICAL_SURFACE ( 'NONE', #20590, 32.50000000000000000 ) ;
#4513 = CARTESIAN_POINT ( 'NONE',  ( -6.988114217767819270, 52.10416666666666430, 26.07999730980490583 ) ) ;
#4514 = CARTESIAN_POINT ( 'NONE',  ( 27.16883889988624290, 61.92500000273119554, 19.73931689729373673 ) ) ;
#4515 = CARTESIAN_POINT ( 'NONE',  ( 6.486482029760649416E-15, 21.87500000273118062, 35.31076352940723240 ) ) ;
#4516 = CARTESIAN_POINT ( 'NONE',  ( -2.162160676586881955E-15, 12.87500000273117884, -35.31076352940723240 ) ) ;
#4517 = CARTESIAN_POINT ( 'NONE',  ( -6.988114217767819270, 28.04166666666666075, 26.07999730980490583 ) ) ;
#4518 = DIRECTION ( 'NONE',  ( 0.000000000000000000, -1.000000000000000000, 0.000000000000000000 ) ) ;
#4519 = CARTESIAN_POINT ( 'NONE',  ( -28.00173670424549499, 23.46392333425730570, -7.543491769121417612 ) ) ;
#4520 = CARTESIAN_POINT ( 'NONE',  ( 7.505752307972854531, 64.13541666666667140, -28.01184896238303423 ) ) ;
#4521 = CARTESIAN_POINT ( 'NONE',  ( -20.75514604977248823, 4.825000002731186122, -28.56700777964554305 ) ) ;
#4522 = CARTESIAN_POINT ( 'NONE',  ( 32.50000000000000000, 3.099999999999989431, -10.55989012756945833 ) ) ;
#4523 = CARTESIAN_POINT ( 'NONE',  ( 26.29305231718578995, 43.20000000000000284, -19.10302069950538240 ) ) ;
#4524 = CARTESIAN_POINT ( 'NONE',  ( 10.37757302488624056, 42.52500000273118275, -31.93888565452638417 ) ) ;
#4525 = CARTESIAN_POINT ( 'NONE',  ( -14.47279130897152122, 18.42499999726882365, 19.92008829642072243 ) ) ;
#4526 = EDGE_CURVE ( 'NONE', #11830, #7617, #7016, .T. ) ;
#4527 = CARTESIAN_POINT ( 'NONE',  ( 32.50000000000000000, 21.60000000546237331, -10.55989012756945833 ) ) ;
#4528 = ORIENTED_EDGE ( 'NONE', *, *, #4748, .T. ) ;
#4529 = CARTESIAN_POINT ( 'NONE',  ( 20.75514604977248467, 60.67500000273118133, -28.56700777964554305 ) ) ;
#4530 = CARTESIAN_POINT ( 'NONE',  ( 32.50000000000000711, 42.90000000000001279, 10.55989012756945122 ) ) ;
#4531 = CIRCLE ( 'NONE', #1770, 30.91025403784432868 ) ;
#4532 = CARTESIAN_POINT ( 'NONE',  ( -7.236395654485763274, 12.02499999726880375, 22.27133577429736633 ) ) ;
#4533 = CARTESIAN_POINT ( 'NONE',  ( -19.06425588902591173, 37.50038166759063074, -19.11951029504763611 ) ) ;
#4534 = ORIENTED_EDGE ( 'NONE', *, *, #1063, .T. ) ;
#4535 = CARTESIAN_POINT ( 'NONE',  ( -10.37757302488624411, 32.72500000273119269, -31.93888565452638417 ) ) ;
#4536 = CIRCLE ( 'NONE', #10037, 24.49999999999999645 ) ;
#4537 = CARTESIAN_POINT ( 'NONE',  ( 19.82091636218621034, 5.799999999999999822, 14.40073868116559730 ) ) ;
#4538 = EDGE_LOOP ( 'NONE', ( #3355, #32044 ) ) ;
#4539 = CARTESIAN_POINT ( 'NONE',  ( 2.521031746877078694E-15, -43.58578643762690064, 0.000000000000000000 ) ) ;
#4540 = CARTESIAN_POINT ( 'NONE',  ( 33.58253175000000113, 70.12500000273119838, -4.112674001490185761E-15 ) ) ;
#4541 = CARTESIAN_POINT ( 'NONE',  ( -30.02300923189239512, 35.63281249999998579, 2.654126918244515359E-13 ) ) ;
#4542 = CARTESIAN_POINT ( 'NONE',  ( 1.577395562988744260E-15, 10.49999999999998757, -25.76082449383753925 ) ) ;
#4543 = CARTESIAN_POINT ( 'NONE',  ( 18.94512977948575738, 2.924999997268806773, 13.76444248337723408 ) ) ;
#4544 = CARTESIAN_POINT ( 'NONE',  ( -33.58253175000000113, 7.225000002731182924, 10.91162601494193929 ) ) ;
#4545 = CARTESIAN_POINT ( 'NONE',  ( -0.04044903255044120238, 48.80430583240936215, -30.02300923189239867 ) ) ;
#4546 = CARTESIAN_POINT ( 'NONE',  ( 15.00000000000000355, 74.90000000000000568, 4.873795443493592394 ) ) ;
#4547 = CARTESIAN_POINT ( 'NONE',  ( -7.505752307972844761, 65.85416666666665719, 28.01184896238304134 ) ) ;
#4548 = DIRECTION ( 'NONE',  ( 0.000000000000000000, 0.000000000000000000, -1.000000000000000000 ) ) ;
#4549 = CARTESIAN_POINT ( 'NONE',  ( -15.00000000000000000, 74.15000000546237402, -4.873795443493594171 ) ) ;
#4550 = CARTESIAN_POINT ( 'NONE',  ( -7.570916362186210335, 12.34999999453761887, -23.30088464923126779 ) ) ;
#4551 = CARTESIAN_POINT ( 'NONE',  ( 2.897257156509938333E-15, 78.75000000546236834, 15.77193336357400710 ) ) ;
#4552 = CARTESIAN_POINT ( 'NONE',  ( 19.09188309203694800, 24.03124999999999645, 19.09188309203660694 ) ) ;
#4553 = CARTESIAN_POINT ( 'NONE',  ( -10.37757302488624411, 30.72500000273117848, -31.93888565452638417 ) ) ;
#4554 = DIRECTION ( 'NONE',  ( -0.000000000000000000, -1.000000000000000000, -0.000000000000000000 ) ) ;
#4555 = CARTESIAN_POINT ( 'NONE',  ( 27.16883889988624290, 44.17500000273118133, 19.73931689729373673 ) ) ;
#4556 = CARTESIAN_POINT ( 'NONE',  ( 10.37757302488624767, 19.97500000273119625, 31.93888565452638417 ) ) ;
#4557 = CARTESIAN_POINT ( 'NONE',  ( 5.779280353836490358E-15, 68.49999999999998579, 32.49999999999999289 ) ) ;
#4558 = VECTOR ( 'NONE', #9899, 1000.000000000000000 ) ;
#4559 = CARTESIAN_POINT ( 'NONE',  ( -1.756012107511856980E-14, 2.500000000000005773, -24.50000000000000000 ) ) ;
#4560 = CARTESIAN_POINT ( 'NONE',  ( -8.446640517145639571E-15, 78.49999999999998579, 32.49999999999999289 ) ) ;
#4561 =( BOUNDED_CURVE ( )  B_SPLINE_CURVE ( 2, ( #12992, #31844, #15916, #20893, #15747, #15400, #270, #26202, #31342, #26372, #18662, #18493, #2523 ),
 .UNSPECIFIED., .F., .T. ) 
 B_SPLINE_CURVE_WITH_KNOTS ( ( 3, 2, 2, 2, 2, 2, 3 ),
 ( 0.09615384615384615918, 0.09743589743589743668, 0.1000000000000000056, 0.1025641025641025605, 0.1051282051282051294, 0.1076923076923076983, 0.1089743589743589758 ),
 .UNSPECIFIED. ) 
 CURVE ( )  GEOMETRIC_REPRESENTATION_ITEM ( )  RATIONAL_B_SPLINE_CURVE ( ( 0.9755282581475767101, 0.9755282581475768211, 1.000000000000000000, 0.9510565162951535312, 1.000000000000000000, 0.9510565162951535312, 1.000000000000000000, 0.9510565162951535312, 1.000000000000000000, 0.9510565162951535312, 1.000000000000000000, 0.9755282581475768211, 0.9755282581475768211 ) ) 
 REPRESENTATION_ITEM ( '' )  );
#4562 = CARTESIAN_POINT ( 'NONE',  ( 10.04305231718579705, 60.60000000000000142, 30.90933677959248982 ) ) ;
#4563 = CARTESIAN_POINT ( 'NONE',  ( -18.94512977948576093, 11.82499999726882578, 13.76444248337722698 ) ) ;
#4564 = CARTESIAN_POINT ( 'NONE',  ( -27.16883889988623935, 61.32500000273119412, 19.73931689729374739 ) ) ;
#4565 = CARTESIAN_POINT ( 'NONE',  ( -12.13525491562421088, 77.80000000000003979, -8.816778784387096835 ) ) ;
#4566 = CARTESIAN_POINT ( 'NONE',  ( -14.01125832528328985, 34.76784749907601935, -24.18731323226223040 ) ) ;
#4567 = CARTESIAN_POINT ( 'NONE',  ( -33.58253175000000113, 77.27500000273117564, -10.91162601494193218 ) ) ;
#4568 = CARTESIAN_POINT ( 'NONE',  ( 20.75514604977249178, 15.82500000273117102, 28.56700777964553950 ) ) ;
#4569 = CARTESIAN_POINT ( 'NONE',  ( 14.47279130897151767, 13.42499999726880411, -19.92008829642072598 ) ) ;
#4570 = CARTESIAN_POINT ( 'NONE',  ( -6.988114217767819270, 58.97916666666666430, 26.07999730980490583 ) ) ;
#4571 = ORIENTED_EDGE ( 'NONE', *, *, #31652, .F. ) ;
#4572 = CARTESIAN_POINT ( 'NONE',  ( -2.162160676586881955E-15, 50.62500000273118417, -35.31076352940723240 ) ) ;
#4573 = CARTESIAN_POINT ( 'NONE',  ( 10.37757302488624767, 23.97500000273118559, 31.93888565452638417 ) ) ;
#4574 = ORIENTED_EDGE ( 'NONE', *, *, #21402, .F. ) ;
#4575 = CARTESIAN_POINT ( 'NONE',  ( -2.584737979205441561E-13, 33.05468750000000000, -30.02300923189239512 ) ) ;
#4576 = CARTESIAN_POINT ( 'NONE',  ( 7.468012846824777284, 36.06809000092397355, 28.02196122052045268 ) ) ;
#4577 = CARTESIAN_POINT ( 'NONE',  ( -4.223320258572819786E-15, 9.499999999999992895, 24.50000000000000000 ) ) ;
#4578 = CARTESIAN_POINT ( 'NONE',  ( -32.50000000000000000, 72.50000000546236834, 0.000000000000000000 ) ) ;
#4579 = CARTESIAN_POINT ( 'NONE',  ( -7.236395654485763274, 6.524999997268826846, 22.27133577429736633 ) ) ;
#4580 = AXIS2_PLACEMENT_3D ( 'NONE', #13019, #31369, #5120 ) ;
#4581 = CARTESIAN_POINT ( 'NONE',  ( -7.236395654485763274, 12.02499999726880375, 22.27133577429736633 ) ) ;
#4582 = CARTESIAN_POINT ( 'NONE',  ( -27.16883889988624290, 17.17500000273119909, -19.73931689729374028 ) ) ;
#4583 = CARTESIAN_POINT ( 'NONE',  ( 32.50000000000000000, 21.50000000546237189, -3.980102097228898626E-15 ) ) ;
#4584 = CARTESIAN_POINT ( 'NONE',  ( 26.29305231718579350, 68.79999999999999716, 19.10302069950537529 ) ) ;
#4585 = CARTESIAN_POINT ( 'NONE',  ( -7.570916362186215665, 5.399999999999987921, 23.30088464923126423 ) ) ;
#4586 = CARTESIAN_POINT ( 'NONE',  ( 20.08610463437158344, 66.69999999999998863, 27.64615127144129403 ) ) ;
#4587 = CARTESIAN_POINT ( 'NONE',  ( 20.47846945139902530, 63.28163166759064495, 20.53372385742071771 ) ) ;
#4588 = CARTESIAN_POINT ( 'NONE',  ( -27.16883889988623935, 27.57500000273119412, 19.73931689729374739 ) ) ;
#4589 = CARTESIAN_POINT ( 'NONE',  ( 20.50609665441005092, 34.34374999999999289, 20.50609665440969209 ) ) ;
#4590 = DIRECTION ( 'NONE',  ( 0.000000000000000000, 0.000000000000000000, 1.000000000000000000 ) ) ;
#4591 = CARTESIAN_POINT ( 'NONE',  ( -23.41746825000000243, 18.02499999726880731, -7.608796670333730638 ) ) ;
#4592 = CARTESIAN_POINT ( 'NONE',  ( 32.50000000000000000, 7.100000000000007638, -10.55989012756945833 ) ) ;
#4593 = CARTESIAN_POINT ( 'NONE',  ( -24.50000000000001066, 17.09999999999998366, 7.960532557706201828 ) ) ;
#4594 = CARTESIAN_POINT ( 'NONE',  ( 14.01125832528330051, 53.67409749907601935, 24.18731323226221974 ) ) ;
#4595 = CARTESIAN_POINT ( 'NONE',  ( 33.58253175000000113, 54.22500000273117848, -10.91162601494193751 ) ) ;
#4596 = CARTESIAN_POINT ( 'NONE',  ( 20.75514604977248467, 64.67500000273118133, -28.56700777964554305 ) ) ;
#4597 = CARTESIAN_POINT ( 'NONE',  ( 20.75514604977249178, 44.07500000273117990, 28.56700777964553950 ) ) ;
#4598 = FACE_OUTER_BOUND ( 'NONE', #15219, .T. ) ;
#4599 = LINE ( 'NONE', #4257, #29797 ) ;
#4600 = DIRECTION ( 'NONE',  ( -1.224646799147353454E-16, 1.000000000000000000, -0.000000000000000000 ) ) ;
#4601 = CARTESIAN_POINT ( 'NONE',  ( -24.48923876278562517, 16.99999999999998579, -0.4945881427486832349 ) ) ;
#4602 = DIRECTION ( 'NONE',  ( -1.000000000000000000, 0.000000000000000000, 0.000000000000000000 ) ) ;
#4603 = CARTESIAN_POINT ( 'NONE',  ( -2.162160676586881955E-15, 20.62500000273119483, -35.31076352940723240 ) ) ;
#4604 = CYLINDRICAL_SURFACE ( 'NONE', #9465, 26.50000000000000355 ) ;
#4605 = FACE_BOUND ( 'NONE', #20807, .T. ) ;
#4606 = DIRECTION ( 'NONE',  ( 0.000000000000000000, 1.000000000000000000, 0.000000000000000000 ) ) ;
#4607 = CARTESIAN_POINT ( 'NONE',  ( -20.47846945139866648, 61.26524333240935505, 20.53372385742108008 ) ) ;
#4608 = CARTESIAN_POINT ( 'NONE',  ( 6.277390505771533514E-15, 39.00000000546236834, 34.17252228774368916 ) ) ;
#4609 = EDGE_CURVE ( 'NONE', #7355, #27495, #33250, .T. ) ;
#4610 = CARTESIAN_POINT ( 'NONE',  ( -10.04305231718578462, 60.90000000546235981, 30.90933677959249337 ) ) ;
#4611 = CARTESIAN_POINT ( 'NONE',  ( 10.37757302488624056, 30.52500000273117209, -31.93888565452638417 ) ) ;
#4612 = CARTESIAN_POINT ( 'NONE',  ( 24.20753774853731244, 37.06510416666666430, -13.97622843553632599 ) ) ;
#4613 = EDGE_CURVE ( 'NONE', #9319, #7495, #22494, .T. ) ;
#4614 = ORIENTED_EDGE ( 'NONE', *, *, #1942, .F. ) ;
#4615 = CARTESIAN_POINT ( 'NONE',  ( 33.58253175000000113, 68.22500000273116427, -10.91162601494193751 ) ) ;
#4616 = CARTESIAN_POINT ( 'NONE',  ( -15.01150461594595775, 41.93489583333333570, 26.00068869287368756 ) ) ;
#4617 = CARTESIAN_POINT ( 'NONE',  ( -1.778240108872766143E-15, 31.49999999999998579, -32.49999999999999289 ) ) ;
#4618 = VERTEX_POINT ( 'NONE', #21257 ) ;
#4619 = CARTESIAN_POINT ( 'NONE',  ( 28.00173670424549499, 56.12017333425732346, 7.543491769121417612 ) ) ;
#4620 = CARTESIAN_POINT ( 'NONE',  ( -19.11951029504763611, 60.70350666759063785, 19.06425588902592239 ) ) ;
#4621 = CARTESIAN_POINT ( 'NONE',  ( -27.16883889988624290, 10.92500000273120797, -19.73931689729374028 ) ) ;
#4622 = CARTESIAN_POINT ( 'NONE',  ( -20.47846945139866648, 16.57774333240934794, 20.53372385742108008 ) ) ;
#4623 = CARTESIAN_POINT ( 'NONE',  ( -26.50000000000000355, -2.000000000000000000, 0.000000000000000000 ) ) ;
#4624 = CARTESIAN_POINT ( 'NONE',  ( 20.75514604977249178, 38.07500000273116569, 28.56700777964553950 ) ) ;
#4625 = CARTESIAN_POINT ( 'NONE',  ( 26.29305231718579350, 41.30000000546238681, 19.10302069950537529 ) ) ;
#4626 = CARTESIAN_POINT ( 'NONE',  ( 12.13525491562420910, 77.19999999999998863, -8.816778784387098611 ) ) ;
#4627 = CARTESIAN_POINT ( 'NONE',  ( -20.75514604977248823, 20.82500000273119412, -28.56700777964554305 ) ) ;
#4628 = FACE_OUTER_BOUND ( 'NONE', #33439, .T. ) ;
#4629 = CARTESIAN_POINT ( 'NONE',  ( -10.37757302488624411, 52.97500000273119980, -31.93888565452638417 ) ) ;
#4630 = SURFACE_STYLE_USAGE ( .BOTH. , #14762 ) ;
#4631 = CARTESIAN_POINT ( 'NONE',  ( 26.29305231718578995, 29.19999999999998863, -19.10302069950538240 ) ) ;
#4632 = CARTESIAN_POINT ( 'NONE',  ( -20.08610463437156923, 28.30000000000000782, 27.64615127144130113 ) ) ;
#4633 = CARTESIAN_POINT ( 'NONE',  ( 14.47279130897151589, 18.32499999726882578, 19.92008829642072953 ) ) ;
#4634 = CARTESIAN_POINT ( 'NONE',  ( 27.16883889988623935, 76.32500000273118701, -19.73931689729374384 ) ) ;
#4635 = CARTESIAN_POINT ( 'NONE',  ( 32.63512777199724724, -24.47487373415290790, 3.996650476574133167E-15 ) ) ;
#4636 = CARTESIAN_POINT ( 'NONE',  ( 13.91746825000000065, 74.27500000273121827, 4.522059556121115875 ) ) ;
#4637 = CARTESIAN_POINT ( 'NONE',  ( -20.75514604977248112, 61.67500000273117422, 28.56700777964554661 ) ) ;
#4638 = CARTESIAN_POINT ( 'NONE',  ( 12.13525491562420910, 75.45000000546237118, -8.816778784387098611 ) ) ;
#4639 = ORIENTED_EDGE ( 'NONE', *, *, #30160, .F. ) ;
#4640 = CARTESIAN_POINT ( 'NONE',  ( -10.37757302488624411, 16.72500000273119269, -31.93888565452638417 ) ) ;
#4641 = CARTESIAN_POINT ( 'NONE',  ( 19.82091636218621389, 7.949999994537631842, -14.40073868116559197 ) ) ;
#4642 = CARTESIAN_POINT ( 'NONE',  ( -26.09010956794232428, 23.17746500092398065, 6.950374756619732253 ) ) ;
#4643 = CARTESIAN_POINT ( 'NONE',  ( 19.82091636218621034, 7.549999994537620829, 14.40073868116559730 ) ) ;
#4644 = CARTESIAN_POINT ( 'NONE',  ( 33.58253175000000823, 38.02500000273117564, 10.91162601494192863 ) ) ;
#4645 = CARTESIAN_POINT ( 'NONE',  ( -27.16883889988623935, 3.575000002731185234, 19.73931689729374739 ) ) ;
#4646 = CARTESIAN_POINT ( 'NONE',  ( 6.486482029760648627E-15, 55.87500000273118417, 35.31076352940722529 ) ) ;
#4647 = CARTESIAN_POINT ( 'NONE',  ( 7.543491769121427382, 48.38579833425730925, -28.00173670424548433 ) ) ;
#4648 = CARTESIAN_POINT ( 'NONE',  ( -1.778240108872766143E-15, 51.50000000000000711, -32.49999999999999289 ) ) ;
#4649 = CARTESIAN_POINT ( 'NONE',  ( 26.02091320914876960, 36.20013916574269075, 14.97647472619900455 ) ) ;
#4650 = CARTESIAN_POINT ( 'NONE',  ( -10.04305231718579172, 60.10000000546238397, -30.90933677959248982 ) ) ;
#4651 = EDGE_CURVE ( 'NONE', #24994, #33572, #16797, .T. ) ;
#4652 = CARTESIAN_POINT ( 'NONE',  ( -8.601468415847515203, 71.17500000273118133, 11.83890561707634959 ) ) ;
#4653 = CARTESIAN_POINT ( 'NONE',  ( 0.000000000000000000, 82.00000000000001421, 0.000000000000000000 ) ) ;
#4654 = CARTESIAN_POINT ( 'NONE',  ( 19.06425588902558133, 66.42149333240935505, -19.11951029504797006 ) ) ;
#4655 = CARTESIAN_POINT ( 'NONE',  ( -23.41746825000000598, 2.224999997268808816, 7.608796670333726198 ) ) ;
#4656 = CARTESIAN_POINT ( 'NONE',  ( 10.04305231718579705, 77.10000000546237686, 30.90933677959248982 ) ) ;
#4657 = DIRECTION ( 'NONE',  ( 0.8660254037844387076, 0.000000000000000000, -0.5000000000000001110 ) ) ;
#4658 = CARTESIAN_POINT ( 'NONE',  ( -10.37757302488623701, 37.77500000273118985, 31.93888565452638417 ) ) ;
#4659 = CARTESIAN_POINT ( 'NONE',  ( 23.41746824999999887, 11.12499999726881938, 0.000000000000000000 ) ) ;
#4660 = ORIENTED_EDGE ( 'NONE', *, *, #11534, .T. ) ;
#4661 = CARTESIAN_POINT ( 'NONE',  ( 33.58253175000000113, 74.37500000273116996, -4.112674001490185761E-15 ) ) ;
#4662 = CARTESIAN_POINT ( 'NONE',  ( 6.277390505771533514E-15, 25.00000000546238255, 34.17252228774368916 ) ) ;
#4663 = CARTESIAN_POINT ( 'NONE',  ( 7.505752307972854531, 40.07291666666666430, -28.01184896238303423 ) ) ;
#4664 = CARTESIAN_POINT ( 'NONE',  ( -32.50000000000000000, 64.50000000546238255, 0.000000000000000000 ) ) ;
#4665 = ORIENTED_EDGE ( 'NONE', *, *, #3422, .T. ) ;
#4666 = CARTESIAN_POINT ( 'NONE',  ( 24.50000000000000000, 5.749999994537624559, 0.000000000000000000 ) ) ;
#4667 = CARTESIAN_POINT ( 'NONE',  ( 33.58253175000000113, 46.22500000273119269, -10.91162601494193751 ) ) ;
#4668 = CARTESIAN_POINT ( 'NONE',  ( 18.94512977948576093, 16.82499999726880091, -13.76444248337722875 ) ) ;
#4669 = CARTESIAN_POINT ( 'NONE',  ( 10.04305231718578817, 5.900000005462368691, -30.90933677959249337 ) ) ;
#4670 = DIRECTION ( 'NONE',  ( 0.000000000000000000, 0.000000000000000000, 1.000000000000000000 ) ) ;
#4671 = DIRECTION ( 'NONE',  ( -0.000000000000000000, -1.000000000000000000, -0.000000000000000000 ) ) ;
#4672 = VECTOR ( 'NONE', #28262, 1000.000000000000000 ) ;
#4673 = CARTESIAN_POINT ( 'NONE',  ( -10.04305231718579172, 49.60000000000000853, -30.90933677959248982 ) ) ;
#4674 = CARTESIAN_POINT ( 'NONE',  ( 2.067204126564591252E-14, 2.500000000000004885, -24.50000000000000000 ) ) ;
#4675 = CARTESIAN_POINT ( 'NONE',  ( -20.75514604977248112, 17.67500000273117422, 28.56700777964554661 ) ) ;
#4676 = CARTESIAN_POINT ( 'NONE',  ( 7.570916362186213000, 0.4000000000000114575, -23.30088464923126423 ) ) ;
#4677 = CARTESIAN_POINT ( 'NONE',  ( -13.94119854578892514, 26.74701416574268720, 24.22776226481266448 ) ) ;
#4678 = CARTESIAN_POINT ( 'NONE',  ( -4.300734207923755825, 75.77500000273118985, 13.23629886949340673 ) ) ;
#4679 = DIRECTION ( 'NONE',  ( -1.000000000000000000, -1.224646799147353454E-16, 0.000000000000000000 ) ) ;
#4680 = CARTESIAN_POINT ( 'NONE',  ( 0.000000000000000000, 0.000000000000000000, 0.000000000000000000 ) ) ;
#4681 = CARTESIAN_POINT ( 'NONE',  ( -32.50000000000000000, 4.099999999999986322, 10.55989012756946366 ) ) ;
#4682 = ORIENTED_EDGE ( 'NONE', *, *, #29841, .T. ) ;
#4683 = CARTESIAN_POINT ( 'NONE',  ( -23.41746825000000243, 16.02499999726881086, -7.608796670333730638 ) ) ;
#4684 = CARTESIAN_POINT ( 'NONE',  ( -18.94512977948575738, 1.424999997268805441, -13.76444248337723231 ) ) ;
#4685 = CARTESIAN_POINT ( 'NONE',  ( -6.988114217768288228, 50.09895833333332860, -26.07999730980477437 ) ) ;
#4686 = CARTESIAN_POINT ( 'NONE',  ( -10.37757302488624411, 58.72500000273119269, -31.93888565452638417 ) ) ;
#4687 = CARTESIAN_POINT ( 'NONE',  ( -27.16883889988624290, 21.17500000273118843, -19.73931689729374028 ) ) ;
#4688 = CARTESIAN_POINT ( 'NONE',  ( 33.58253175000000113, 10.47500000273118204, -10.91162601494193751 ) ) ;
#4689 = CARTESIAN_POINT ( 'NONE',  ( 27.95245687107223276, 30.47656250000000355, -2.463307335887066074E-13 ) ) ;
#4690 = CARTESIAN_POINT ( 'NONE',  ( 20.53372385742072481, 21.17225666759064850, -20.47846945139902175 ) ) ;
#4691 = CARTESIAN_POINT ( 'NONE',  ( -15.01150461594642138, 63.70572916666667140, -26.00068869287340334 ) ) ;
#4692 = CARTESIAN_POINT ( 'NONE',  ( 33.58253175000000113, 4.225000002731190030, -10.91162601494193751 ) ) ;
#4693 = CARTESIAN_POINT ( 'NONE',  ( 5.147494310547434893, 68.55125428154684641, 32.49999999999999289 ) ) ;
#4694 = CARTESIAN_POINT ( 'NONE',  ( 20.08610463437157279, 39.30000000000001137, -27.64615127144129758 ) ) ;
#4695 = CARTESIAN_POINT ( 'NONE',  ( 6.486482029760648627E-15, 43.62500000273116996, 35.31076352940722529 ) ) ;
#4696 = CARTESIAN_POINT ( 'NONE',  ( 18.94512977948576093, 6.824999997268821339, -13.76444248337722875 ) ) ;
#4697 = CARTESIAN_POINT ( 'NONE',  ( -4.223320258572819786E-15, 13.50000000000000355, 24.50000000000000000 ) ) ;
#4698 = ORIENTED_EDGE ( 'NONE', *, *, #4457, .T. ) ;
#4699 = CARTESIAN_POINT ( 'NONE',  ( 10.37757302488624767, 51.97500000273118559, 31.93888565452638417 ) ) ;
#4700 = LINE ( 'NONE', #23246, #19569 ) ;
#4701 = CARTESIAN_POINT ( 'NONE',  ( -19.06425588902591173, 40.93788166759063785, -19.11951029504763611 ) ) ;
#4702 = CARTESIAN_POINT ( 'NONE',  ( 10.37757302488624767, 73.97500000273119269, 31.93888565452638417 ) ) ;
#4703 = ORIENTED_EDGE ( 'NONE', *, *, #20979, .F. ) ;
#4704 = CARTESIAN_POINT ( 'NONE',  ( 27.16883889988623935, 22.32500000273117280, -19.73931689729374384 ) ) ;
#4705 = CARTESIAN_POINT ( 'NONE',  ( 26.00068869287340334, 19.87760416666666430, -15.01150461594642316 ) ) ;
#4706 = EDGE_LOOP ( 'NONE', ( #2983, #19651, #11954, #25514 ) ) ;
#4707 = VECTOR ( 'NONE', #8638, 1000.000000000000000 ) ;
#4708 = CARTESIAN_POINT ( 'NONE',  ( 7.428728520588063561E-18, -23.06066017177981564, 0.000000000000000000 ) ) ;
#4709 = CARTESIAN_POINT ( 'NONE',  ( 33.58253175000000113, 70.22500000273120691, -10.91162601494193751 ) ) ;
#4710 = CARTESIAN_POINT ( 'NONE',  ( 26.00068869287340334, 43.94010416666665719, -15.01150461594642316 ) ) ;
#4711 = CARTESIAN_POINT ( 'NONE',  ( 15.14183272437241889, 13.70000000000000462, 20.84094480462498211 ) ) ;
#4712 = DIRECTION ( 'NONE',  ( -0.000000000000000000, -1.000000000000000000, -0.000000000000000000 ) ) ;
#4713 = CARTESIAN_POINT ( 'NONE',  ( -2.162160676586881955E-15, 8.625000002731169957, -35.31076352940723240 ) ) ;
#4714 = DIRECTION ( 'NONE',  ( -0.000000000000000000, 1.000000000000000000, -0.000000000000000000 ) ) ;
#4715 = CARTESIAN_POINT ( 'NONE',  ( -20.53372385742107653, 48.37461833240936215, -20.47846945139867003 ) ) ;
#4716 = CARTESIAN_POINT ( 'NONE',  ( 4.635254915624209993, 75.40000000000001990, -14.26584774442730463 ) ) ;
#4717 = CARTESIAN_POINT ( 'NONE',  ( -26.00068869287340334, 62.84635416666667140, 15.01150461594643559 ) ) ;
#4718 = CARTESIAN_POINT ( 'NONE',  ( -26.29305231718578995, 70.19999999999998863, 19.10302069950538595 ) ) ;
#4719 = CARTESIAN_POINT ( 'NONE',  ( 32.50000000000000000, 23.09999999999999432, -10.55989012756945833 ) ) ;
#4720 = CARTESIAN_POINT ( 'NONE',  ( 15.14183272437242245, 16.04999999453762882, -20.84094480462497856 ) ) ;
#4721 = CARTESIAN_POINT ( 'NONE',  ( -11.25946833292375793, 78.67500000273119554, -8.180482586598733619 ) ) ;
#4722 = CARTESIAN_POINT ( 'NONE',  ( 13.97622843553633665, 20.73697916666666075, 24.20753774853730889 ) ) ;
#4723 = CARTESIAN_POINT ( 'NONE',  ( 27.16883889988623935, 32.32500000273119412, -19.73931689729374384 ) ) ;
#4724 = CARTESIAN_POINT ( 'NONE',  ( 33.58253175000000113, 42.37500000273118417, -4.112674001490185761E-15 ) ) ;
#4725 = CARTESIAN_POINT ( 'NONE',  ( -33.58253175000000113, 21.37500000273118062, 0.000000000000000000 ) ) ;
#4726 = CARTESIAN_POINT ( 'NONE',  ( -1.778240108872766143E-15, 12.00000000546238077, -32.49999999999999289 ) ) ;
#4727 = CARTESIAN_POINT ( 'NONE',  ( 20.75514604977249178, 73.82500000273120122, 28.56700777964553950 ) ) ;
#4728 = CARTESIAN_POINT ( 'NONE',  ( -32.50000000000000000, 65.89999999999999147, -10.55989012756945300 ) ) ;
#4729 = CARTESIAN_POINT ( 'NONE',  ( 32.50000000000000000, 60.99999999999998579, -3.980102097228898626E-15 ) ) ;
#4730 = CYLINDRICAL_SURFACE ( 'NONE', #25949, 32.50000000000000000 ) ;
#4731 = CARTESIAN_POINT ( 'NONE',  ( 20.75514604977249178, 65.82500000273115859, 28.56700777964553950 ) ) ;
#4732 = CARTESIAN_POINT ( 'NONE',  ( -9.270509831248419985, 78.29999999999995453, 12.75976212528060039 ) ) ;
#4733 = CARTESIAN_POINT ( 'NONE',  ( 6.950374756619257965, 42.07253499907601935, -26.09010956794244507 ) ) ;
#4734 = CARTESIAN_POINT ( 'NONE',  ( -33.58253175000000113, 71.47500000273119269, 10.91162601494193929 ) ) ;
#4735 = CARTESIAN_POINT ( 'NONE',  ( 20.75514604977248467, 8.425000002731204418, -28.56700777964554305 ) ) ;
#4736 = CARTESIAN_POINT ( 'NONE',  ( 23.41746825000000243, 11.02499999726882152, 7.608796670333735079 ) ) ;
#4737 = CARTESIAN_POINT ( 'NONE',  ( -26.07999730980490583, 63.27604166666667140, -6.988114217767815717 ) ) ;
#4738 = EDGE_CURVE ( 'NONE', #15262, #16782, #4771, .T. ) ;
#4739 = ORIENTED_EDGE ( 'NONE', *, *, #2377, .T. ) ;
#4740 = CARTESIAN_POINT ( 'NONE',  ( 33.58253175000000823, 50.02500000273118985, 10.91162601494192863 ) ) ;
#4741 = ORIENTED_EDGE ( 'NONE', *, *, #12302, .T. ) ;
#4742 = CARTESIAN_POINT ( 'NONE',  ( 15.01150461594596308, 36.77864583333332860, -26.00068869287367335 ) ) ;
#4743 = CARTESIAN_POINT ( 'NONE',  ( 0.04044903254992426173, 31.05506916759064495, -30.02300923189239867 ) ) ;
#4744 = CARTESIAN_POINT ( 'NONE',  ( -1.778240108872766143E-15, 59.50000000000000711, -32.49999999999999289 ) ) ;
#4745 = CARTESIAN_POINT ( 'NONE',  ( 20.08610463437157279, 7.800000005462373487, -27.64615127144129758 ) ) ;
#4746 = CARTESIAN_POINT ( 'NONE',  ( 0.000000000000000000, 80.00000000000001421, -32.50000000000000000 ) ) ;
#4747 = CARTESIAN_POINT ( 'NONE',  ( -23.41746825000000598, 4.224999997268803931, 7.608796670333726198 ) ) ;
#4748 = EDGE_CURVE ( 'NONE', #14496, #21334, #23824, .T. ) ;
#4749 = EDGE_CURVE ( 'NONE', #10964, #27108, #31197, .T. ) ;
#4750 = CARTESIAN_POINT ( 'NONE',  ( -7.236395654485757944, 11.22499999726880837, -22.27133577429736988 ) ) ;
#4751 = CARTESIAN_POINT ( 'NONE',  ( -33.58253175000000113, 13.27500000273119518, -10.91162601494193218 ) ) ;
#4752 = CARTESIAN_POINT ( 'NONE',  ( 20.08610463437157279, 21.80000000546236549, -27.64615127144129758 ) ) ;
#4753 = CARTESIAN_POINT ( 'NONE',  ( -32.50000000000000000, 63.89999999999998437, -10.55989012756945478 ) ) ;
#4754 = CARTESIAN_POINT ( 'NONE',  ( 12.13525491562420910, 77.45000000546237118, -8.816778784387098611 ) ) ;
#4755 = FACE_OUTER_BOUND ( 'NONE', #16535, .T. ) ;
#4756 = CARTESIAN_POINT ( 'NONE',  ( -25.98046417659859486, 61.41965250092398776, -15.04653450569291628 ) ) ;
#4757 = CARTESIAN_POINT ( 'NONE',  ( -20.75514604977248823, 29.07500000273119056, -28.56700777964554305 ) ) ;
#4758 = CARTESIAN_POINT ( 'NONE',  ( -13.91746824999999887, 81.37500000273118417, 0.000000000000000000 ) ) ;
#4759 = CARTESIAN_POINT ( 'NONE',  ( 26.00068869287341045, 37.06510416666667140, -15.01150461594642493 ) ) ;
#4760 = CIRCLE ( 'NONE', #1437, 12.00000000000000178 ) ;
#4761 = CARTESIAN_POINT ( 'NONE',  ( 7.236395654485760609, 15.52499999726880731, -22.27133577429736633 ) ) ;
#4762 = CARTESIAN_POINT ( 'NONE',  ( 32.50000000000000000, 9.100000000000004974, -10.55989012756945833 ) ) ;
#4763 = CARTESIAN_POINT ( 'NONE',  ( -5.147494310547430452, 51.55125428154684641, -32.49999999999999289 ) ) ;
#4764 = CARTESIAN_POINT ( 'NONE',  ( 7.025853678916867295, 50.37982666574269075, 26.06988505166722803 ) ) ;
#4765 = CARTESIAN_POINT ( 'NONE',  ( -27.16883889988623935, 47.32500000273117990, 19.73931689729374739 ) ) ;
#4766 = CARTESIAN_POINT ( 'NONE',  ( 33.58253175000000113, 62.37500000273120548, -4.112674001490185761E-15 ) ) ;
#4767 = CARTESIAN_POINT ( 'NONE',  ( 10.37757302488624056, 42.77500000273118275, -31.93888565452638417 ) ) ;
#4768 = CARTESIAN_POINT ( 'NONE',  ( 0.000000000000000000, 16.99999999999998579, 0.000000000000000000 ) ) ;
#4769 = AXIS2_PLACEMENT_3D ( 'NONE', #30087, #14492, #19479 ) ;
#4770 = CARTESIAN_POINT ( 'NONE',  ( -27.95245687107223276, 15.00781249999999645, 2.498001805406602216E-13 ) ) ;
#4771 = LINE ( 'NONE', #18173, #31665 ) ;
#4772 = CARTESIAN_POINT ( 'NONE',  ( 10.04305231718578817, 51.90000000546238113, -30.90933677959249337 ) ) ;
#4773 = CARTESIAN_POINT ( 'NONE',  ( -2.092463501923844636E-15, 79.49999999999998579, -34.17252228774368916 ) ) ;
#4774 = CARTESIAN_POINT ( 'NONE',  ( -27.16883889988623935, 23.32500000273117635, 19.73931689729374739 ) ) ;
#4775 = DIRECTION ( 'NONE',  ( 0.000000000000000000, 1.000000000000000000, 0.000000000000000000 ) ) ;
#4776 = FACE_OUTER_BOUND ( 'NONE', #26198, .T. ) ;
#4777 = DIRECTION ( 'NONE',  ( 0.000000000000000000, 0.000000000000000000, -1.000000000000000000 ) ) ;
#4778 = CARTESIAN_POINT ( 'NONE',  ( -14.97647472619899389, 61.12201416574268364, 26.02091320914878025 ) ) ;
#4779 = CARTESIAN_POINT ( 'NONE',  ( 6.277390505771533514E-15, 41.00000000546236123, 34.17252228774368916 ) ) ;
#4780 = CARTESIAN_POINT ( 'NONE',  ( -5.147494310547377161, 60.05125428700924317, -32.50000000000002132 ) ) ;
#4781 = CARTESIAN_POINT ( 'NONE',  ( 20.75514604977248467, 26.42500000273118843, -28.56700777964554305 ) ) ;
#4782 = CARTESIAN_POINT ( 'NONE',  ( -24.20753774853756823, 35.91927083333332860, -13.97622843553588723 ) ) ;
#4783 = ORIENTED_EDGE ( 'NONE', *, *, #24050, .T. ) ;
#4784 = CARTESIAN_POINT ( 'NONE',  ( -33.58253175000000113, 71.12500000273118417, 0.000000000000000000 ) ) ;
#4785 = CARTESIAN_POINT ( 'NONE',  ( -15.01150461594642138, 43.08072916666666430, -26.00068869287340334 ) ) ;
#4786 = CARTESIAN_POINT ( 'NONE',  ( -1.778240108872766143E-15, 16.00000000546237899, -32.49999999999999289 ) ) ;
#4787 = ORIENTED_EDGE ( 'NONE', *, *, #33841, .T. ) ;
#4788 = CARTESIAN_POINT ( 'NONE',  ( -7.468012846824771955, 54.97434000092398065, -28.02196122052045624 ) ) ;
#4789 = CARTESIAN_POINT ( 'NONE',  ( -7.025853678916393008, 56.97954833425730925, 26.06988505166735592 ) ) ;
#4790 = CARTESIAN_POINT ( 'NONE',  ( -20.75514604977248112, 9.425000002731184878, 28.56700777964554661 ) ) ;
#4791 = CIRCLE ( 'NONE', #26729, 24.50000000000000000 ) ;
#4792 = CARTESIAN_POINT ( 'NONE',  ( -28.01184896238304134, 66.71354166666665719, -7.505752307972844761 ) ) ;
#4793 = CARTESIAN_POINT ( 'NONE',  ( 3.980102097228898626E-15, 80.00000000000001421, 32.50000000000000000 ) ) ;
#4794 = CARTESIAN_POINT ( 'NONE',  ( -33.58253175000000113, 37.37500000273119838, 0.000000000000000000 ) ) ;
#4795 = CARTESIAN_POINT ( 'NONE',  ( -10.04305231718578462, 44.90000000546237402, 30.90933677959249337 ) ) ;
#4796 = CARTESIAN_POINT ( 'NONE',  ( -15.00000000000000000, 76.00000000000001421, 0.000000000000000000 ) ) ;
#4797 = CARTESIAN_POINT ( 'NONE',  ( 6.486482029760649416E-15, 23.62500000273119127, 35.31076352940723240 ) ) ;
#4798 = CARTESIAN_POINT ( 'NONE',  ( 3.880418787951140036, 14.19874571299077637, -24.49999999999999645 ) ) ;
#4799 = CARTESIAN_POINT ( 'NONE',  ( 33.58253175000000823, 52.27500000273118985, 10.91162601494192863 ) ) ;
#4800 = CARTESIAN_POINT ( 'NONE',  ( 6.277390505771533514E-15, 26.50000000000000711, 34.17252228774368916 ) ) ;
#4801 = CARTESIAN_POINT ( 'NONE',  ( 10.04305231718578817, 27.40000000000000924, -30.90933677959249337 ) ) ;
#4802 = CARTESIAN_POINT ( 'NONE',  ( -24.50000000000000355, 0.9000000000000005773, -7.960532557706207157 ) ) ;
#4803 = ADVANCED_FACE ( 'NONE', ( #13014 ), #8661, .T. ) ;
#4804 = CARTESIAN_POINT ( 'NONE',  ( 27.16883889988624290, 67.92500000273119554, 19.73931689729373673 ) ) ;
#4805 = CARTESIAN_POINT ( 'NONE',  ( 20.08610463437157279, 63.30000000000001137, -27.64615127144129758 ) ) ;
#4806 = CARTESIAN_POINT ( 'NONE',  ( -13.91746824999999532, 75.27500000273118985, -4.522059556121115875 ) ) ;
#4807 = CARTESIAN_POINT ( 'NONE',  ( -33.58253175000000113, 63.47500000273117848, 10.91162601494193929 ) ) ;
#4808 = CARTESIAN_POINT ( 'NONE',  ( 15.00000000000000000, 71.35000000546237686, -4.873795443493596835 ) ) ;
#4809 = CARTESIAN_POINT ( 'NONE',  ( 32.50000000000000000, 7.600000005462378638, -10.55989012756945833 ) ) ;
#4810 = CARTESIAN_POINT ( 'NONE',  ( 20.75514604977248467, 18.42500000273117422, -28.56700777964554305 ) ) ;
#4811 = CARTESIAN_POINT ( 'NONE',  ( 24.50000000000000000, 11.74999999453762989, 0.000000000000000000 ) ) ;
#4812 = CARTESIAN_POINT ( 'NONE',  ( -27.95245687107223986, 16.44569416759064140, -0.04044903254993292840 ) ) ;
#4813 = CARTESIAN_POINT ( 'NONE',  ( 32.50000000000000711, 46.90000000000000568, 10.55989012756945122 ) ) ;
#4814 = CARTESIAN_POINT ( 'NONE',  ( 6.486482029760649416E-15, 41.62500000273116996, 35.31076352940723240 ) ) ;
#4815 = CARTESIAN_POINT ( 'NONE',  ( 10.04305231718578817, 57.39999999999999147, -30.90933677959249337 ) ) ;
#4816 = CARTESIAN_POINT ( 'NONE',  ( -10.37757302488623701, 57.77500000273121117, 31.93888565452638417 ) ) ;
#4817 = CARTESIAN_POINT ( 'NONE',  ( -0.04044903254990864921, 49.96131916759065206, 30.02300923189239867 ) ) ;
#4818 = CARTESIAN_POINT ( 'NONE',  ( 19.82091636218621034, 15.80000000000000782, 14.40073868116559730 ) ) ;
#4819 = CARTESIAN_POINT ( 'NONE',  ( -14.97647472619899389, 40.49701416574269786, 26.02091320914878025 ) ) ;
#4820 = CARTESIAN_POINT ( 'NONE',  ( 32.50000000000000000, 63.50000000546239676, -3.980102097228898626E-15 ) ) ;
#4821 = CARTESIAN_POINT ( 'NONE',  ( -4.300734207923759378, 78.97500000273122112, -13.23629886949340495 ) ) ;
#4822 = CARTESIAN_POINT ( 'NONE',  ( 26.29305231718579350, 62.79999999999999716, 19.10302069950537529 ) ) ;
#4823 = CARTESIAN_POINT ( 'NONE',  ( 19.11951029504797006, 67.28086833240935505, 19.06425588902558133 ) ) ;
#4824 = CARTESIAN_POINT ( 'NONE',  ( -32.50000000000000000, 53.90000000000001279, -10.55989012756945300 ) ) ;
#4825 = CARTESIAN_POINT ( 'NONE',  ( 32.50000000000000000, 75.60000000546236265, -10.55989012756945833 ) ) ;
#4826 = CARTESIAN_POINT ( 'NONE',  ( 30.02300923189239512, 13.28906249999999289, -2.619432448724977703E-13 ) ) ;
#4827 = CARTESIAN_POINT ( 'NONE',  ( 27.16883889988624290, 34.17500000273120264, 19.73931689729373673 ) ) ;
#4828 = CARTESIAN_POINT ( 'NONE',  ( 23.41746824999999887, 5.124999997268814056, 0.000000000000000000 ) ) ;
#4829 = EDGE_LOOP ( 'NONE', ( #850, #10070, #28426, #24088 ) ) ;
#4830 = CARTESIAN_POINT ( 'NONE',  ( -2.162160676586881955E-15, 76.87500000273115575, -35.31076352940723240 ) ) ;
#4831 = CARTESIAN_POINT ( 'NONE',  ( -20.08610463437157989, 26.20000000546237828, -27.64615127144129758 ) ) ;
#4832 = CARTESIAN_POINT ( 'NONE',  ( 28.01184896238304134, 44.36979166666666430, 7.505752307972846538 ) ) ;
#4833 = CARTESIAN_POINT ( 'NONE',  ( -7.505752307973343918, 56.97395833333333570, -28.01184896238290989 ) ) ;
#4834 = CARTESIAN_POINT ( 'NONE',  ( 27.16883889988623935, 52.57500000273118701, -19.73931689729374384 ) ) ;
#4835 = CARTESIAN_POINT ( 'NONE',  ( -26.29305231718578995, 60.70000000546238539, 19.10302069950538595 ) ) ;
#4836 = ORIENTED_EDGE ( 'NONE', *, *, #12067, .F. ) ;
#4837 = DIRECTION ( 'NONE',  ( 0.000000000000000000, -1.000000000000000000, 0.000000000000000000 ) ) ;
#4838 = CARTESIAN_POINT ( 'NONE',  ( 27.16883889988624290, 43.92500000273119554, 19.73931689729373673 ) ) ;
#4839 = CYLINDRICAL_SURFACE ( 'NONE', #14868, 32.50000000000000000 ) ;
#4840 = CARTESIAN_POINT ( 'NONE',  ( 27.16883889988624290, 66.17500000273118133, 19.73931689729373673 ) ) ;
#4841 = CARTESIAN_POINT ( 'NONE',  ( -20.08610463437156923, 6.800000005462376151, 27.64615127144130113 ) ) ;
#4842 = CARTESIAN_POINT ( 'NONE',  ( 33.58253175000000823, 60.02500000273116854, 10.91162601494192685 ) ) ;
#4843 = CARTESIAN_POINT ( 'NONE',  ( 0.000000000000000000, 80.00000000000001421, 0.000000000000000000 ) ) ;
#4844 = CARTESIAN_POINT ( 'NONE',  ( 26.29305231718578995, 45.19999999999998863, -19.10302069950538240 ) ) ;
#4845 = EDGE_CURVE ( 'NONE', #24499, #3193, #545, .T. ) ;
#4846 = CARTESIAN_POINT ( 'NONE',  ( -32.50000000000000000, 13.89999999999999680, -10.55989012756945300 ) ) ;
#4847 = CARTESIAN_POINT ( 'NONE',  ( 20.75514604977248467, 14.67500000273117955, -28.56700777964554305 ) ) ;
#4848 = CARTESIAN_POINT ( 'NONE',  ( -5.147494310547403806, 73.55125428154681799, -32.50000000000000711 ) ) ;
#4849 = CARTESIAN_POINT ( 'NONE',  ( -19.06425588902558133, 23.45274333240935150, 19.11951029504797006 ) ) ;
#4850 = CARTESIAN_POINT ( 'NONE',  ( -13.91746824999999532, 77.47500000273120691, 4.522059556121122093 ) ) ;
#4851 = DIRECTION ( 'NONE',  ( 0.000000000000000000, 0.000000000000000000, -1.000000000000000000 ) ) ;
#4852 = CARTESIAN_POINT ( 'NONE',  ( 5.779280353836490358E-15, 22.49999999999999645, 32.49999999999999289 ) ) ;
#4853 = ADVANCED_FACE ( 'NONE', ( #7856 ), #18005, .F. ) ;
#4854 = CARTESIAN_POINT ( 'NONE',  ( -33.58253175000000113, 77.27500000273117564, -10.91162601494193218 ) ) ;
#4855 = ORIENTED_EDGE ( 'NONE', *, *, #12029, .T. ) ;
#4856 = CARTESIAN_POINT ( 'NONE',  ( -14.47279130897151589, 11.82499999726882578, -19.92008829642072598 ) ) ;
#4857 = CARTESIAN_POINT ( 'NONE',  ( -4.523095164977117273E-15, 4.124999997268806951, 24.62258325217400312 ) ) ;
#4858 = CARTESIAN_POINT ( 'NONE',  ( 6.988114217767829928, 53.82291666666666430, -26.07999730980489872 ) ) ;
#4859 = CARTESIAN_POINT ( 'NONE',  ( 33.58253175000000113, 62.22500000273119269, -10.91162601494193751 ) ) ;
#4860 = CARTESIAN_POINT ( 'NONE',  ( 20.75514604977249178, 18.07500000273119056, 28.56700777964553950 ) ) ;
#4861 = CARTESIAN_POINT ( 'NONE',  ( 27.16883889988623935, 10.57500000273119056, -19.73931689729374384 ) ) ;
#4862 = CARTESIAN_POINT ( 'NONE',  ( 24.20753774853756113, 27.32552083333333215, 13.97622843553589789 ) ) ;
#4863 = CARTESIAN_POINT ( 'NONE',  ( -25.98046417659859486, 20.16965250092397355, -15.04653450569291628 ) ) ;
#4864 = CARTESIAN_POINT ( 'NONE',  ( -26.00068869287368756, 63.41927083333333570, -15.01150461594595775 ) ) ;
#4865 = CARTESIAN_POINT ( 'NONE',  ( -27.16883889988623935, 5.325000002731187010, 19.73931689729374739 ) ) ;
#4866 =( BOUNDED_CURVE ( )  B_SPLINE_CURVE ( 2, ( #9645, #22691, #30396, #20127, #184, #13593, #5523, #31431, #21321, #26627, #28514, #8253, #12908 ),
 .UNSPECIFIED., .F., .T. ) 
 B_SPLINE_CURVE_WITH_KNOTS ( ( 3, 2, 2, 2, 2, 2, 3 ),
 ( 0.6500000000000000222, 0.6600000000000000311, 0.6800000000000000488, 0.6999999999999999556, 0.7199999999999999734, 0.7399999999999999911, 0.7500000000000000000 ),
 .UNSPECIFIED. ) 
 CURVE ( )  GEOMETRIC_REPRESENTATION_ITEM ( )  RATIONAL_B_SPLINE_CURVE ( ( 0.9755282581475768211, 0.9755282581475768211, 1.000000000000000000, 0.9510565162951535312, 1.000000000000000000, 0.9510565162951535312, 1.000000000000000000, 0.9510565162951535312, 1.000000000000000000, 0.9510565162951535312, 1.000000000000000000, 0.9755282581475768211, 0.9755282581475768211 ) ) 
 REPRESENTATION_ITEM ( '' )  );
#4867 = CARTESIAN_POINT ( 'NONE',  ( 11.25946833292375793, 72.57500000273120122, -8.180482586598735395 ) ) ;
#4868 = CARTESIAN_POINT ( 'NONE',  ( 26.29305231718579350, 42.79999999999999005, 19.10302069950537529 ) ) ;
#4869 = CARTESIAN_POINT ( 'NONE',  ( 20.75514604977248467, 48.42500000273119554, -28.56700777964554305 ) ) ;
#4870 = CARTESIAN_POINT ( 'NONE',  ( 14.47279130897151589, 6.324999997268824892, 19.92008829642072953 ) ) ;
#4871 = CARTESIAN_POINT ( 'NONE',  ( 15.14183272437242067, 13.70000000000000462, 20.84094480462498211 ) ) ;
#4872 = EDGE_LOOP ( 'NONE', ( #18774, #31877, #27282, #19398 ) ) ;
#4873 = CARTESIAN_POINT ( 'NONE',  ( -33.58253175000000113, 53.47500000273117848, 10.91162601494193929 ) ) ;
#4874 = CARTESIAN_POINT ( 'NONE',  ( -10.04305231718578462, 4.900000005462368691, 30.90933677959249337 ) ) ;
#4875 = CARTESIAN_POINT ( 'NONE',  ( 24.18731323226247554, 45.95090250092398065, 14.01125832528285997 ) ) ;
#4876 = CARTESIAN_POINT ( 'NONE',  ( 20.75514604977249178, 76.07500000273118701, 28.56700777964553950 ) ) ;
#4877 = ORIENTED_EDGE ( 'NONE', *, *, #21121, .T. ) ;
#4878 = CARTESIAN_POINT ( 'NONE',  ( -20.75514604977248823, 24.82500000273117635, -28.56700777964554305 ) ) ;
#4879 = CARTESIAN_POINT ( 'NONE',  ( -20.50609665441004736, 11.99999999999999645, -20.50609665440969565 ) ) ;
#4880 = ORIENTED_EDGE ( 'NONE', *, *, #12497, .T. ) ;
#4881 = LINE ( 'NONE', #15872, #680 ) ;
#4882 = CARTESIAN_POINT ( 'NONE',  ( -10.37757302488624411, 58.72500000273117848, -31.93888565452638417 ) ) ;
#4883 = CARTESIAN_POINT ( 'NONE',  ( 30.02300923189239512, 37.35156249999997868, -2.619432448724977703E-13 ) ) ;
#4884 = CARTESIAN_POINT ( 'NONE',  ( 0.000000000000000000, -12.99999999999999822, 0.000000000000000000 ) ) ;
#4885 = CARTESIAN_POINT ( 'NONE',  ( -14.47279130897152299, 4.424999997268826313, 19.92008829642072243 ) ) ;
#4886 = CARTESIAN_POINT ( 'NONE',  ( -27.16883889988623935, 13.32500000273117990, 19.73931689729374739 ) ) ;
#4887 = CARTESIAN_POINT ( 'NONE',  ( 0.000000000000000000, -12.99999999999999822, 0.000000000000000000 ) ) ;
#4888 = CARTESIAN_POINT ( 'NONE',  ( 30.02300923189239867, 56.53868083240936215, -0.04044903255044467877 ) ) ;
#4889 = CARTESIAN_POINT ( 'NONE',  ( 9.270509831248423538, 73.29999999999996874, -12.75976212528059861 ) ) ;
#4890 = CARTESIAN_POINT ( 'NONE',  ( 26.00068869287367690, 65.13802083333334281, 15.01150461594596486 ) ) ;
#4891 = CARTESIAN_POINT ( 'NONE',  ( 5.147494310547434893, 19.05125428700922185, 32.49999999999999289 ) ) ;
#4892 = CARTESIAN_POINT ( 'NONE',  ( -32.50000000000000000, 17.89999999999998437, -10.55989012756945478 ) ) ;
#4893 = EDGE_CURVE ( 'NONE', #29527, #17796, #10273, .T. ) ;
#4894 = CARTESIAN_POINT ( 'NONE',  ( 15.14183272437242245, 10.04999999453761639, -20.84094480462497856 ) ) ;
#4895 = CARTESIAN_POINT ( 'NONE',  ( -8.601468415847515203, 79.17500000273120975, 11.83890561707634959 ) ) ;
#4896 = CARTESIAN_POINT ( 'NONE',  ( -24.20753774853756823, 22.16927083333332504, -13.97622843553588723 ) ) ;
#4897 = CARTESIAN_POINT ( 'NONE',  ( 33.58253175000000823, 32.02500000273118275, 10.91162601494192863 ) ) ;
#4898 = CARTESIAN_POINT ( 'NONE',  ( 0.000000000000000000, 80.00000000000001421, 0.000000000000000000 ) ) ;
#4899 = CARTESIAN_POINT ( 'NONE',  ( 10.37757302488624767, 43.97500000273117848, 31.93888565452638417 ) ) ;
#4900 = CARTESIAN_POINT ( 'NONE',  ( 33.58253175000000113, 20.47500000273119980, -10.91162601494193574 ) ) ;
#4901 = CARTESIAN_POINT ( 'NONE',  ( -4.635254915624208216, 80.40000000000000568, 14.26584774442730463 ) ) ;
#4902 = CARTESIAN_POINT ( 'NONE',  ( -33.58253175000000113, 75.02500000273117564, -10.91162601494193041 ) ) ;
#4903 = CARTESIAN_POINT ( 'NONE',  ( 26.29305231718578995, 59.70000000546238539, -19.10302069950538240 ) ) ;
#4904 = CARTESIAN_POINT ( 'NONE',  ( -20.08610463437157989, 59.70000000000000284, -27.64615127144129758 ) ) ;
#4905 = CARTESIAN_POINT ( 'NONE',  ( 18.94512977948576093, 16.82499999726880091, -13.76444248337722875 ) ) ;
#4906 = CARTESIAN_POINT ( 'NONE',  ( -33.58253175000000113, 63.02500000273118985, -10.91162601494193041 ) ) ;
#4907 = CARTESIAN_POINT ( 'NONE',  ( -7.236395654485763274, 6.524999997268826846, 22.27133577429736633 ) ) ;
#4908 = EDGE_CURVE ( 'NONE', #22684, #15950, #23655, .T. ) ;
#4909 = CARTESIAN_POINT ( 'NONE',  ( 33.58253175000000113, 76.37500000273118417, -4.112674001490185761E-15 ) ) ;
#4910 = CARTESIAN_POINT ( 'NONE',  ( -20.75514604977248823, 6.825000002731195892, -28.56700777964554305 ) ) ;
#4911 = CARTESIAN_POINT ( 'NONE',  ( 14.47279130897151589, 16.82499999726881512, 19.92008829642072953 ) ) ;
#4912 = CARTESIAN_POINT ( 'NONE',  ( 26.09010956794232428, 18.02121500092397710, -6.950374756619718042 ) ) ;
#4913 = VERTEX_POINT ( 'NONE', #32202 ) ;
#4914 = CARTESIAN_POINT ( 'NONE',  ( 33.58253175000000823, 46.02500000273118275, 10.91162601494192863 ) ) ;
#4915 = ORIENTED_EDGE ( 'NONE', *, *, #8318, .F. ) ;
#4916 = ORIENTED_EDGE ( 'NONE', *, *, #32529, .T. ) ;
#4917 = CARTESIAN_POINT ( 'NONE',  ( -26.00068869287340334, 38.78385416666665719, 15.01150461594643382 ) ) ;
#4918 = CARTESIAN_POINT ( 'NONE',  ( 3.880418787951134707, 9.551254281546839309, 24.50000000000000000 ) ) ;
#4919 = CARTESIAN_POINT ( 'NONE',  ( -10.04305231718579172, 2.100000005462371533, -30.90933677959248982 ) ) ;
#4920 = CARTESIAN_POINT ( 'NONE',  ( -24.50000000000000000, 8.649999994537632020, -7.960532557706207157 ) ) ;
#4921 = CARTESIAN_POINT ( 'NONE',  ( -23.41746825000000598, 2.224999997268808816, 7.608796670333726198 ) ) ;
#4922 = CARTESIAN_POINT ( 'NONE',  ( -23.41746825000000598, 9.724999997268804819, 7.608796670333726198 ) ) ;
#4923 = CARTESIAN_POINT ( 'NONE',  ( 10.37757302488624056, 14.77500000273118630, -31.93888565452638417 ) ) ;
#4924 = CARTESIAN_POINT ( 'NONE',  ( 10.04305231718578817, 15.90000000546237757, -30.90933677959249337 ) ) ;
#4925 = CARTESIAN_POINT ( 'NONE',  ( -2.092463501923844636E-15, 63.50000000000000000, -34.17252228774368916 ) ) ;
#4926 = CARTESIAN_POINT ( 'NONE',  ( 15.14183272437242067, 11.44999999453763095, 20.84094480462498211 ) ) ;
#4927 = CARTESIAN_POINT ( 'NONE',  ( 3.445340210940985210E-14, 5.499999999999997335, 24.50000000000000000 ) ) ;
#4928 = CARTESIAN_POINT ( 'NONE',  ( -28.02196122052045268, 60.98996500092398065, 7.468012846824790607 ) ) ;
#4929 = CARTESIAN_POINT ( 'NONE',  ( -32.50000000000000000, 32.50000000546238255, 0.000000000000000000 ) ) ;
#4930 = CARTESIAN_POINT ( 'NONE',  ( -20.50609665440969209, 38.64062500000000000, 20.50609665441005092 ) ) ;
#4931 = SHAPE_DEFINITION_REPRESENTATION ( #13749, #19696 ) ;
#4932 = CARTESIAN_POINT ( 'NONE',  ( 23.41746824999999887, 17.12499999726882649, 0.000000000000000000 ) ) ;
#4933 = CARTESIAN_POINT ( 'NONE',  ( -32.50000000000000000, 8.100000000000006750, 10.55989012756946366 ) ) ;
#4934 = CARTESIAN_POINT ( 'NONE',  ( -4.635254915624208216, 74.40000000000001990, 14.26584774442730463 ) ) ;
#4935 = CARTESIAN_POINT ( 'NONE',  ( -26.09010956794245217, 54.96315999907602645, -6.950374756619243755 ) ) ;
#4936 = CARTESIAN_POINT ( 'NONE',  ( 27.16883889988623935, 52.32500000273118701, -19.73931689729374384 ) ) ;
#4937 = CARTESIAN_POINT ( 'NONE',  ( 33.58253175000000113, 60.37500000273120548, -4.112674001490185761E-15 ) ) ;
#4938 = CARTESIAN_POINT ( 'NONE',  ( -27.16883889988623935, 39.57500000273117280, 19.73931689729374739 ) ) ;
#4939 = CARTESIAN_POINT ( 'NONE',  ( 14.47279130897151944, 14.92499999726881477, -19.92008829642072598 ) ) ;
#4940 = CARTESIAN_POINT ( 'NONE',  ( 6.988114217767829928, 16.01041666666666075, -26.07999730980489872 ) ) ;
#4941 = CARTESIAN_POINT ( 'NONE',  ( -5.147494310547423346, 62.44874571845315359, 32.50000000000000000 ) ) ;
#4942 = DIRECTION ( 'NONE',  ( -1.224646799147353454E-16, 1.000000000000000000, -0.000000000000000000 ) ) ;
#4943 = CARTESIAN_POINT ( 'NONE',  ( -32.50000000000000000, 27.99999999999999645, 0.000000000000000000 ) ) ;
#4944 = CARTESIAN_POINT ( 'NONE',  ( -10.37757302488624411, 12.72500000273117671, -31.93888565452638417 ) ) ;
#4945 = CARTESIAN_POINT ( 'NONE',  ( -26.29305231718578995, 62.70000000546238539, 19.10302069950538595 ) ) ;
#4946 = CARTESIAN_POINT ( 'NONE',  ( -7.579748464070165821E-14, 12.24999999453762456, -24.50000000000000000 ) ) ;
#4947 = EDGE_CURVE ( 'NONE', #3774, #4956, #20518, .T. ) ;
#4948 = DIRECTION ( 'NONE',  ( 0.000000000000000000, 0.000000000000000000, -1.000000000000000000 ) ) ;
#4949 = CARTESIAN_POINT ( 'NONE',  ( 27.95245687107223276, 15.28868083240935505, -0.04044903255042905932 ) ) ;
#4950 = CARTESIAN_POINT ( 'NONE',  ( 10.04305231718579705, 35.10000000546238397, 30.90933677959248982 ) ) ;
#4951 = CARTESIAN_POINT ( 'NONE',  ( -20.08610463437156923, 66.29999999999999716, 27.64615127144130113 ) ) ;
#4952 = PRODUCT ( 'bellows suction cup', 'bellows suction cup', '', ( #23473 ) ) ;
#4953 = CARTESIAN_POINT ( 'NONE',  ( 33.58253175000000823, 24.02500000273117919, 10.91162601494192685 ) ) ;
#4954 = CARTESIAN_POINT ( 'NONE',  ( 6.988114217767829928, 43.51041666666666430, -26.07999730980489872 ) ) ;
#4955 = EDGE_CURVE ( 'NONE', #6049, #20971, #26216, .T. ) ;
#4956 = VERTEX_POINT ( 'NONE', #18846 ) ;
#4957 = CARTESIAN_POINT ( 'NONE',  ( 10.37757302488624056, 60.52500000273118275, -31.93888565452638417 ) ) ;
#4958 = CARTESIAN_POINT ( 'NONE',  ( 26.00068869287367335, 47.95052083333331439, 15.01150461594596308 ) ) ;
#4959 = ORIENTED_EDGE ( 'NONE', *, *, #27703, .F. ) ;
#4960 = CARTESIAN_POINT ( 'NONE',  ( 26.02091320914851025, 62.56548583425730925, -14.97647472619946463 ) ) ;
#4961 = CARTESIAN_POINT ( 'NONE',  ( 24.22776226481241224, 59.12798583425730925, -13.94119854578936923 ) ) ;
#4962 = ORIENTED_EDGE ( 'NONE', *, *, #17336, .F. ) ;
#4963 = CARTESIAN_POINT ( 'NONE',  ( -27.16883889988623935, 9.325000002731190563, 19.73931689729374739 ) ) ;
#4964 =( BOUNDED_CURVE ( )  B_SPLINE_CURVE ( 2, ( #23967, #8167, #16082, #26536, #26867, #13832, #10921, #13669, #16743, #32176, #437, #29265, #5768 ),
 .UNSPECIFIED., .F., .T. ) 
 B_SPLINE_CURVE_WITH_KNOTS ( ( 3, 2, 2, 2, 2, 2, 3 ),
 ( 0.4551282051282051211, 0.4564102564102563986, 0.4589743589743589536, 0.4615384615384615641, 0.4641025641025641191, 0.4666666666666666741, 0.4679487179487179516 ),
 .UNSPECIFIED. ) 
 CURVE ( )  GEOMETRIC_REPRESENTATION_ITEM ( )  RATIONAL_B_SPLINE_CURVE ( ( 0.9755282581475768211, 0.9755282581475768211, 1.000000000000000000, 0.9510565162951535312, 1.000000000000000000, 0.9510565162951535312, 1.000000000000000000, 0.9510565162951535312, 1.000000000000000000, 0.9510565162951535312, 1.000000000000000000, 0.9755282581475768211, 0.9755282581475768211 ) ) 
 REPRESENTATION_ITEM ( '' )  );
#4965 = EDGE_CURVE ( 'NONE', #29760, #12253, #15816, .T. ) ;
#4966 = CARTESIAN_POINT ( 'NONE',  ( 7.468012846824281681, 14.57253499907601935, -28.02196122052058058 ) ) ;
#4967 = CARTESIAN_POINT ( 'NONE',  ( -20.08610463437157989, 45.69999999999998153, -27.64615127144129758 ) ) ;
#4968 = CARTESIAN_POINT ( 'NONE',  ( 27.16883889988624290, 36.17500000273118843, 19.73931689729373673 ) ) ;
#4969 = CARTESIAN_POINT ( 'NONE',  ( -32.50000000000000000, 40.60000000546239107, 10.55989012756946366 ) ) ;
#4970 =( BOUNDED_CURVE ( )  B_SPLINE_CURVE ( 2, ( #9863, #10043, #28055, #15193, #20172, #30615, #33188, #7798, #28396, #20858, #33888, #31304, #25992, #31139, #18287, #22911, #2486, #12954, #4543, #28732, #12784, #17593, #33720, #15711, #25656, #7464, #15017, #26167, #30965, #23428, #17947, #20340, #2659, #4885, #7111, #23257, #25487, #1966, #10217, #20697, #7630, #12441, #33367, #30790, #5056, #15540, #15876, #3168, #23935, #13638, #21695, #570, #736, #31639, #31477, #5738, #26333, #2996, #11061, #2821, #8298, #230, #23764, #18790, #16542, #21364, #16048, #21526, #404, #26995, #10717, #7969, #26503, #18455, #8469, #13469, #28898, #60, #24269, #10890, #5400, #5567, #13290, #21196, #24102, #31974, #26673, #18957, #29402, #29233, #8137, #29062, #10547, #18626, #31807, #5904, #16218, #16381, #26834, #3330, #13800, #19121, #11221, #32142, #8636, #29558, #6058, #13120, #23595, #21028, #30061, #6399, #30401, #32307, #6901, #3657, #29897, #16709, #27164, #14464, #3991, #11709, #1571, #6567, #11883, #16874, #17382, #9473, #9134, #19615, #12048, #14296, #27501, #6730, #17041, #6230, #19954, #27337, #22518, #14133, #17213, #32639, #3823, #21859, #8799, #24589, #32969, #24920, #1405, #3493, #22354, #19779, #1061, #32801, #11384, #11542, #9294, #27671, #30228, #902, #4161, #19282, #19451, #24425, #29725, #13962, #22024, #14634, #25093, #32468, #8969, #24754, #1230, #22192, #28012, #7593, #18070, #33144, #15496, #20474, #7238 ),
 .UNSPECIFIED., .F., .T. ) 
 B_SPLINE_CURVE_WITH_KNOTS ( ( 3, 2, 2, 2, 2, 2, 2, 2, 2, 2, 2, 2, 2, 2, 2, 2, 2, 2, 2, 2, 2, 2, 2, 2, 2, 2, 2, 2, 2, 2, 2, 2, 2, 2, 2, 2, 2, 2, 2, 2, 2, 2, 2, 2, 2, 2, 2, 2, 2, 2, 2, 2, 2, 2, 2, 2, 2, 2, 2, 2, 2, 2, 2, 2, 2, 2, 2, 2, 2, 2, 2, 2, 2, 2, 2, 2, 2, 2, 2, 2, 2, 2, 2, 2, 2, 2, 2, 2, 2, 2, 3 ),
 ( 0.000000000000000000, 0.01111111111111111154, 0.02222222222222222307, 0.03333333333333333287, 0.04444444444444444614, 0.05555555555555555247, 0.06666666666666666574, 0.07777777777777777901, 0.08888888888888889228, 0.1000000000000000056, 0.1111111111111111049, 0.1222222222222222182, 0.1333333333333333315, 0.1444444444444444309, 0.1555555555555555580, 0.1666666666666666574, 0.1777777777777777846, 0.1888888888888888840, 0.2000000000000000111, 0.2111111111111111105, 0.2222222222222222099, 0.2333333333333333370, 0.2444444444444444364, 0.2555555555555555358, 0.2666666666666666630, 0.2777777777777777901, 0.2888888888888888618, 0.2999999999999999889, 0.3111111111111111160, 0.3222222222222222432, 0.3333333333333333148, 0.3444444444444444420, 0.3555555555555555691, 0.3666666666666666408, 0.3777777777777777679, 0.3888888888888888951, 0.4000000000000000222, 0.4111111111111110938, 0.4222222222222222210, 0.4333333333333333481, 0.4444444444444444198, 0.4555555555555555469, 0.4666666666666666741, 0.4777777777777778012, 0.4888888888888888729, 0.5000000000000000000, 0.5111111111111110716, 0.5222222222222222543, 0.5333333333333333259, 0.5444444444444443976, 0.5555555555555555802, 0.5666666666666666519, 0.5777777777777777235, 0.5888888888888889062, 0.5999999999999999778, 0.6111111111111111605, 0.6222222222222222321, 0.6333333333333333037, 0.6444444444444444864, 0.6555555555555555580, 0.6666666666666666297, 0.6777777777777778123, 0.6888888888888888840, 0.6999999999999999556, 0.7111111111111111382, 0.7222222222222222099, 0.7333333333333332815, 0.7444444444444444642, 0.7555555555555555358, 0.7666666666666667185, 0.7777777777777777901, 0.7888888888888888618, 0.8000000000000000444, 0.8111111111111111160, 0.8222222222222221877, 0.8333333333333333703, 0.8444444444444444420, 0.8555555555555555136, 0.8666666666666666963, 0.8777777777777777679, 0.8888888888888888395, 0.9000000000000000222, 0.9111111111111110938, 0.9222222222222222765, 0.9333333333333333481, 0.9444444444444444198, 0.9555555555555556024, 0.9666666666666666741, 0.9777777777777777457, 0.9888888888888889284, 1.000000000000000000 ),
 .UNSPECIFIED. ) 
 CURVE ( )  GEOMETRIC_REPRESENTATION_ITEM ( )  RATIONAL_B_SPLINE_CURVE ( ( 1.000000000000000000, 0.9510565162951535312, 1.000000000000000000, 0.9510565162951535312, 1.000000000000000000, 0.9510565162951535312, 1.000000000000000000, 0.9510565162951535312, 1.000000000000000000, 0.9510565162951535312, 1.000000000000000000, 0.9510565162951535312, 1.000000000000000000, 0.9510565162951535312, 1.000000000000000000, 0.9510565162951535312, 1.000000000000000000, 0.9510565162951535312, 1.000000000000000000, 0.9510565162951535312, 1.000000000000000000, 0.9510565162951535312, 1.000000000000000000, 0.9510565162951535312, 1.000000000000000000, 0.9510565162951535312, 1.000000000000000000, 0.9510565162951535312, 1.000000000000000000, 0.9510565162951535312, 1.000000000000000000, 0.9510565162951535312, 1.000000000000000000, 0.9510565162951535312, 1.000000000000000000, 0.9510565162951535312, 1.000000000000000000, 0.9510565162951535312, 1.000000000000000000, 0.9510565162951535312, 1.000000000000000000, 0.9510565162951535312, 1.000000000000000000, 0.9510565162951535312, 1.000000000000000000, 0.9510565162951535312, 1.000000000000000000, 0.9510565162951535312, 1.000000000000000000, 0.9510565162951535312, 1.000000000000000000, 0.9510565162951535312, 1.000000000000000000, 0.9510565162951535312, 1.000000000000000000, 0.9510565162951535312, 1.000000000000000000, 0.9510565162951535312, 1.000000000000000000, 0.9510565162951535312, 1.000000000000000000, 0.9510565162951535312, 1.000000000000000000, 0.9510565162951535312, 1.000000000000000000, 0.9510565162951535312, 1.000000000000000000, 0.9510565162951535312, 1.000000000000000000, 0.9510565162951535312, 1.000000000000000000, 0.9510565162951535312, 1.000000000000000000, 0.9510565162951535312, 1.000000000000000000, 0.9510565162951535312, 1.000000000000000000, 0.9510565162951535312, 1.000000000000000000, 0.9510565162951535312, 1.000000000000000000, 0.9510565162951535312, 1.000000000000000000, 0.9510565162951535312, 1.000000000000000000, 0.9510565162951535312, 1.000000000000000000, 0.9510565162951535312, 1.000000000000000000, 0.9510565162951535312, 1.000000000000000000, 0.9510565162951535312, 1.000000000000000000, 0.9510565162951535312, 1.000000000000000000, 0.9510565162951535312, 1.000000000000000000, 0.9510565162951535312, 1.000000000000000000, 0.9510565162951535312, 1.000000000000000000, 0.9510565162951535312, 1.000000000000000000, 0.9510565162951535312, 1.000000000000000000, 0.9510565162951535312, 1.000000000000000000, 0.9510565162951535312, 1.000000000000000000, 0.9510565162951535312, 1.000000000000000000, 0.9510565162951535312, 1.000000000000000000, 0.9510565162951535312, 1.000000000000000000, 0.9510565162951535312, 1.000000000000000000, 0.9510565162951535312, 1.000000000000000000, 0.9510565162951535312, 1.000000000000000000, 0.9510565162951535312, 1.000000000000000000, 0.9510565162951535312, 1.000000000000000000, 0.9510565162951535312, 1.000000000000000000, 0.9510565162951535312, 1.000000000000000000, 0.9510565162951535312, 1.000000000000000000, 0.9510565162951535312, 1.000000000000000000, 0.9510565162951535312, 1.000000000000000000, 0.9510565162951535312, 1.000000000000000000, 0.9510565162951535312, 1.000000000000000000, 0.9510565162951535312, 1.000000000000000000, 0.9510565162951535312, 1.000000000000000000, 0.9510565162951535312, 1.000000000000000000, 0.9510565162951535312, 1.000000000000000000, 0.9510565162951535312, 1.000000000000000000, 0.9510565162951535312, 1.000000000000000000, 0.9510565162951535312, 1.000000000000000000, 0.9510565162951535312, 1.000000000000000000, 0.9510565162951535312, 1.000000000000000000, 0.9510565162951535312, 1.000000000000000000, 0.9510565162951535312, 1.000000000000000000, 0.9510565162951535312, 1.000000000000000000, 0.9510565162951535312, 1.000000000000000000, 0.9510565162951535312, 1.000000000000000000, 0.9510565162951535312, 1.000000000000000000, 0.9510565162951535312, 1.000000000000000000, 0.9510565162951535312, 1.000000000000000000, 0.9510565162951535312, 1.000000000000000000, 0.9510565162951535312, 1.000000000000000000, 0.9510565162951535312, 1.000000000000000000, 0.9510565162951535312, 1.000000000000000000 ) ) 
 REPRESENTATION_ITEM ( '' )  );
#4971 = CARTESIAN_POINT ( 'NONE',  ( -9.270509831248425314, 79.69999999999997442, -12.75976212528059861 ) ) ;
#4972 = CARTESIAN_POINT ( 'NONE',  ( -20.08610463437156923, 48.30000000000001847, 27.64615127144130113 ) ) ;
#4973 = CARTESIAN_POINT ( 'NONE',  ( -2.162160676586881955E-15, 22.62500000273119127, -35.31076352940723240 ) ) ;
#4974 = CARTESIAN_POINT ( 'NONE',  ( -26.29305231718578995, 52.70000000546236407, 19.10302069950538595 ) ) ;
#4975 = CARTESIAN_POINT ( 'NONE',  ( 6.486482029760649416E-15, 49.87500000273119838, 35.31076352940723240 ) ) ;
#4976 = CARTESIAN_POINT ( 'NONE',  ( 32.50000000000000000, 31.00000000000001421, -3.980102097228898626E-15 ) ) ;
#4977 = CARTESIAN_POINT ( 'NONE',  ( -10.04305231718578462, 30.39999999999998437, 30.90933677959249337 ) ) ;
#4978 = CARTESIAN_POINT ( 'NONE',  ( 15.14183272437241889, 7.699999999999988631, 20.84094480462498211 ) ) ;
#4979 = CARTESIAN_POINT ( 'NONE',  ( -20.75514604977248823, 70.82500000273117280, -28.56700777964554305 ) ) ;
#4980 = CARTESIAN_POINT ( 'NONE',  ( -30.28308157046056337, 66.99999999999997158, 13.46430247876124753 ) ) ;
#4981 = CARTESIAN_POINT ( 'NONE',  ( -5.147494310547423346, 38.44874571845315359, 32.50000000000000000 ) ) ;
#4982 = CARTESIAN_POINT ( 'NONE',  ( -33.58253175000000113, 63.37500000273119127, 0.000000000000000000 ) ) ;
#4983 = CARTESIAN_POINT ( 'NONE',  ( 32.50000000000000711, 72.89999999999999147, 10.55989012756945122 ) ) ;
#4984 = CARTESIAN_POINT ( 'NONE',  ( -10.37757302488624411, 10.72500000273118914, -31.93888565452638417 ) ) ;
#4985 = CARTESIAN_POINT ( 'NONE',  ( -27.95245687107223986, 30.19569416759064140, -0.04044903254993292840 ) ) ;
#4986 = CARTESIAN_POINT ( 'NONE',  ( 24.50000000000000000, 9.849999994537622428, -7.960532557706203605 ) ) ;
#4987 = CARTESIAN_POINT ( 'NONE',  ( -27.16883889988623935, 35.32500000273118701, 19.73931689729374739 ) ) ;
#4988 = CARTESIAN_POINT ( 'NONE',  ( 32.50000000000000000, 57.10000000000000142, -10.55989012756945833 ) ) ;
#4989 = CARTESIAN_POINT ( 'NONE',  ( 5.147494310547434893, 18.55125428154684286, 32.49999999999999289 ) ) ;
#4990 = CARTESIAN_POINT ( 'NONE',  ( -4.300734207923759378, 74.47500000273116427, -13.23629886949340495 ) ) ;
#4991 = CARTESIAN_POINT ( 'NONE',  ( 28.02196122052058413, 46.36940999907602645, 7.468012846824272799 ) ) ;
#4992 = CARTESIAN_POINT ( 'NONE',  ( -26.29305231718578995, 60.70000000546237118, 19.10302069950538595 ) ) ;
#4993 = CARTESIAN_POINT ( 'NONE',  ( 2.688165632520823219E-15, 75.87500000273115575, 14.63369212191046387 ) ) ;
#4994 = CARTESIAN_POINT ( 'NONE',  ( -19.06425588902558133, 64.70274333240935505, 19.11951029504797006 ) ) ;
#4995 = CARTESIAN_POINT ( 'NONE',  ( -6.668400408272875007E-16, 0.5000000000000068834, -24.50000000000000355 ) ) ;
#4996 = CARTESIAN_POINT ( 'NONE',  ( -10.04305231718578462, 76.90000000546237402, 30.90933677959249337 ) ) ;
#4997 = CARTESIAN_POINT ( 'NONE',  ( -15.01150461594595775, 21.30989583333331794, 26.00068869287368756 ) ) ;
#4998 = CARTESIAN_POINT ( 'NONE',  ( -33.58253175000000113, 35.27500000273120406, -10.91162601494193218 ) ) ;
#4999 = CARTESIAN_POINT ( 'NONE',  ( -23.41746825000000243, 6.224999997268798602, 7.608796670333725309 ) ) ;
#5000 = ORIENTED_EDGE ( 'NONE', *, *, #11667, .F. ) ;
#5001 = CARTESIAN_POINT ( 'NONE',  ( -2.162160676586881955E-15, 74.87500000273116996, -35.31076352940723240 ) ) ;
#5002 = CARTESIAN_POINT ( 'NONE',  ( -20.08610463437157989, 22.20000000546238184, -27.64615127144129758 ) ) ;
#5003 = CARTESIAN_POINT ( 'NONE',  ( 30.02300923189239512, 40.78906249999998579, -2.619432448724977703E-13 ) ) ;
#5004 = CARTESIAN_POINT ( 'NONE',  ( 28.01184896238304134, 64.99479166666665719, 7.505752307972846538 ) ) ;
#5005 = CARTESIAN_POINT ( 'NONE',  ( 20.75514604977249178, 56.07500000273117990, 28.56700777964553950 ) ) ;
#5006 = CARTESIAN_POINT ( 'NONE',  ( -32.50000000000000000, 56.50000000546237544, 0.000000000000000000 ) ) ;
#5007 = DIRECTION ( 'NONE',  ( -1.224646799147353207E-16, -1.499759782661857882E-32, 1.000000000000000000 ) ) ;
#5008 = CARTESIAN_POINT ( 'NONE',  ( 20.75514604977248467, 42.42500000273117422, -28.56700777964554305 ) ) ;
#5009 = CARTESIAN_POINT ( 'NONE',  ( -2.375766604868041476, 72.44874571845316780, 14.99999999999999822 ) ) ;
#5010 = AXIS2_PLACEMENT_3D ( 'NONE', #25727, #31041, #28299 ) ;
#5011 = CARTESIAN_POINT ( 'NONE',  ( -20.75514604977248823, 69.07500000273115859, -28.56700777964554305 ) ) ;
#5012 = CARTESIAN_POINT ( 'NONE',  ( 20.08610463437157279, 5.800000005462378816, -27.64615127144129758 ) ) ;
#5013 = CARTESIAN_POINT ( 'NONE',  ( -10.37757302488623701, 61.52500000273118985, 31.93888565452638417 ) ) ;
#5014 = CARTESIAN_POINT ( 'NONE',  ( -7.505752307973343918, 12.28645833333333037, -28.01184896238290989 ) ) ;
#5015 = CARTESIAN_POINT ( 'NONE',  ( -10.04305231718578462, 48.39999999999999858, 30.90933677959249337 ) ) ;
#5016 = DIRECTION ( 'NONE',  ( -0.000000000000000000, -1.000000000000000000, -0.000000000000000000 ) ) ;
#5017 = CARTESIAN_POINT ( 'NONE',  ( 27.16883889988624290, 12.17500000273119554, 19.73931689729373673 ) ) ;
#5018 = CARTESIAN_POINT ( 'NONE',  ( -3.880418787951124493, 7.448745718453147369, 24.50000000000000355 ) ) ;
#5019 = CARTESIAN_POINT ( 'NONE',  ( 26.06988505166722803, 32.33295166574267654, -7.025853678916862854 ) ) ;
#5020 = CARTESIAN_POINT ( 'NONE',  ( -11.25946833292375793, 71.07500000273120122, 8.180482586598737171 ) ) ;
#5021 = FACE_OUTER_BOUND ( 'NONE', #24340, .T. ) ;
#5022 = CARTESIAN_POINT ( 'NONE',  ( -20.08610463437157989, 21.69999999999998153, -27.64615127144129758 ) ) ;
#5023 = CARTESIAN_POINT ( 'NONE',  ( 20.75514604977249178, 74.07500000273120122, 28.56700777964553950 ) ) ;
#5024 = VERTEX_POINT ( 'NONE', #6290 ) ;
#5025 = CARTESIAN_POINT ( 'NONE',  ( 23.41746824999999887, 15.12499999726882294, 0.000000000000000000 ) ) ;
#5026 = CARTESIAN_POINT ( 'NONE',  ( 23.41746824999999887, 2.524999997268799312, 7.608796670333735079 ) ) ;
#5027 = CARTESIAN_POINT ( 'NONE',  ( -13.97622843553632421, 56.83072916666665009, -24.20753774853731599 ) ) ;
#5028 = CARTESIAN_POINT ( 'NONE',  ( -10.37757302488624411, 52.72500000273121401, -31.93888565452638417 ) ) ;
#5029 = CARTESIAN_POINT ( 'NONE',  ( -27.16883889988623935, 19.57500000273119767, 19.73931689729374739 ) ) ;
#5030 = CARTESIAN_POINT ( 'NONE',  ( -33.58253175000000113, 1.375000002731191495, 0.000000000000000000 ) ) ;
#5031 = CARTESIAN_POINT ( 'NONE',  ( -24.20753774853756823, 39.35677083333333570, -13.97622843553588723 ) ) ;
#5032 = UNCERTAINTY_MEASURE_WITH_UNIT (LENGTH_MEASURE( 1.000000000000000082E-05 ), #17682, 'distance_accuracy_value', 'NONE');
#5033 = CARTESIAN_POINT ( 'NONE',  ( -20.53372385742071771, 19.45350666759063785, 20.47846945139902530 ) ) ;
#5034 = CARTESIAN_POINT ( 'NONE',  ( -28.00173670424535644, 23.73920166574268364, 7.543491769121936308 ) ) ;
#5035 = CARTESIAN_POINT ( 'NONE',  ( 6.486482029760649416E-15, 5.625000002731175286, 35.31076352940723240 ) ) ;
#5036 = CARTESIAN_POINT ( 'NONE',  ( 33.36402495954516212, 51.99999999999999289, -0.4025740098922445664 ) ) ;
#5037 = PRESENTATION_LAYER_ASSIGNMENT (  '', '', ( #17088 ) ) ;
#5038 = CARTESIAN_POINT ( 'NONE',  ( -33.58253175000000113, 45.22500000273117848, 10.91162601494193929 ) ) ;
#5039 = CARTESIAN_POINT ( 'NONE',  ( 18.94512977948575738, 12.42499999726881477, 13.76444248337723408 ) ) ;
#5040 = CARTESIAN_POINT ( 'NONE',  ( 2.584737979205442066E-13, 65.71093749999998579, 27.95245687107223276 ) ) ;
#5041 = ORIENTED_EDGE ( 'NONE', *, *, #16366, .T. ) ;
#5042 = EDGE_CURVE ( 'NONE', #28529, #17976, #11406, .T. ) ;
#5043 = CARTESIAN_POINT ( 'NONE',  ( -27.16883889988624290, 55.17500000273119554, -19.73931689729374028 ) ) ;
#5044 = CARTESIAN_POINT ( 'NONE',  ( -29.99999999999999645, -91.00000000000000000, 3.673940397442059967E-15 ) ) ;
#5045 = CARTESIAN_POINT ( 'NONE',  ( 0.04044903254993986036, 37.93006916759064495, -27.95245687107223986 ) ) ;
#5046 = CARTESIAN_POINT ( 'NONE',  ( 27.16883889988624290, 76.17500000273119554, 19.73931689729373673 ) ) ;
#5047 = EDGE_CURVE ( 'NONE', #22185, #17375, #29293, .T. ) ;
#5048 = ORIENTED_EDGE ( 'NONE', *, *, #16975, .F. ) ;
#5049 = CARTESIAN_POINT ( 'NONE',  ( 20.75514604977249178, 23.82500000273118701, 28.56700777964553950 ) ) ;
#5050 = CARTESIAN_POINT ( 'NONE',  ( -20.50609665440969209, 14.57812499999999645, 20.50609665441005092 ) ) ;
#5051 = VERTEX_POINT ( 'NONE', #6118 ) ;
#5052 = DIRECTION ( 'NONE',  ( 0.000000000000000000, 0.000000000000000000, 1.000000000000000000 ) ) ;
#5053 = CARTESIAN_POINT ( 'NONE',  ( -33.58253175000000113, 59.12500000273118417, 0.000000000000000000 ) ) ;
#5054 = CARTESIAN_POINT ( 'NONE',  ( -7.505752307973343918, 36.34895833333333570, -28.01184896238290989 ) ) ;
#5055 = CARTESIAN_POINT ( 'NONE',  ( 7.570916362186213000, 16.39999999999999858, -23.30088464923126423 ) ) ;
#5056 = CARTESIAN_POINT ( 'NONE',  ( 7.236395654485760609, 5.524999997268825958, -22.27133577429736633 ) ) ;
#5057 = CARTESIAN_POINT ( 'NONE',  ( -33.58253175000000113, 3.125000002731193049, 0.000000000000000000 ) ) ;
#5058 = CARTESIAN_POINT ( 'NONE',  ( -26.02091320914878025, 61.98138916574268364, -14.97647472619899389 ) ) ;
#5059 = CARTESIAN_POINT ( 'NONE',  ( -10.37757302488624411, 78.97500000273119269, -31.93888565452638417 ) ) ;
#5060 = CARTESIAN_POINT ( 'NONE',  ( 4.635254915624212657, 80.60000000000000853, 14.26584774442730286 ) ) ;
#5061 = CARTESIAN_POINT ( 'NONE',  ( 32.50000000000000711, 75.40000000546238823, 10.55989012756945122 ) ) ;
#5062 = CARTESIAN_POINT ( 'NONE',  ( 10.04305231718579705, 18.59999999999999076, 30.90933677959248982 ) ) ;
#5063 = CARTESIAN_POINT ( 'NONE',  ( -6.988114217768288228, 60.41145833333332149, -26.07999730980477437 ) ) ;
#5064 = CARTESIAN_POINT ( 'NONE',  ( 24.50000000000000355, 13.84999999453761177, -7.960532557706203605 ) ) ;
#5065 = CARTESIAN_POINT ( 'NONE',  ( 15.00000000000000355, 73.15000000546240244, 4.873795443493592394 ) ) ;
#5066 = CARTESIAN_POINT ( 'NONE',  ( -19.09188309203694445, 25.74999999999999645, -19.09188309203661049 ) ) ;
#5067 =( BOUNDED_SURFACE ( )  B_SPLINE_SURFACE ( 1, 2, ( 
 ( #6783, #7120, #22242, #4379, #17777, #19829, #30111, #1282, #27724, #20349, #22920, #9182, #9346, #11761, #4212, #4551, #30281, #33376, #11934, #22403, #22570, #1455, #17093, #17435, #9871, #14854, #6951, #30799, #6615, #17261, #14684, #25320, #7292, #9700, #1621, #15030, #32687, #33020, #17602, #12450, #28235, #32851, #4040, #1794, #30624, #9526, #24804, #19666, #27552, #12272, #27896, #14514, #25495, #1975, #24973, #20007, #30454, #22746, #33197, #20180, #12964, #15375, #23604, #7978, #10559, #18124, #18464, #71, #2144, #28908, #25665, #5065, #25830, #5409, #10227, #10050, #26002, #15888, #2495, #12619, #20707, #26344, #23438, #2671, #28569, #23086, #23267, #33549, #2320, #7474, #7808, #13302, #28742, #31316, #23777, #20531, #31149, #7640, #15722, #31650, #21038 ),
 ( #33899, #31488, #26177, #12793, #15550, #15201, #5238, #10390, #33729, #2833, #20868, #30974, #18297, #17956, #13130, #28405, #243, #4895, #10729, #21206, #8148, #18637, #4721, #11069, #13809, #414, #14143, #5913, #29735, #24111, #26682, #32318, #26843, #3008, #31983, #8980, #29074, #745, #3338, #32479, #3178, #3669, #27004, #24277, #3502, #579, #16228, #11230, #6068, #13647, #912, #6240, #19292, #1073, #21535, #21706, #8480, #5578, #27176, #13972, #18967, #16721, #22035, #24599, #32152, #24435, #8645, #19130, #10900, #16059, #29567, #23945, #16551, #11391, #29411, #21868, #8809, #11553, #26514, #13480, #21373, #31817, #8308, #18799, #29243, #16390, #5747, #25107, #27684, #12410, #19790, #7083, #14308, #6744, #9485, #6578, #19462, #4341, #19627, #1583, #20143 ) ),
 .UNSPECIFIED., .F., .F., .F. ) 
 B_SPLINE_SURFACE_WITH_KNOTS ( ( 2, 2 ),
 ( 3, 2, 2, 2, 2, 2, 2, 2, 2, 2, 2, 2, 2, 2, 2, 2, 2, 2, 2, 2, 2, 2, 2, 2, 2, 2, 2, 2, 2, 2, 2, 2, 2, 2, 2, 2, 2, 2, 2, 2, 2, 2, 2, 2, 2, 2, 2, 2, 2, 2, 3 ),
 ( 0.000000000000000000, 1.000000000000000000 ),
 ( 0.000000000000000000, 0.02000000000000000042, 0.04000000000000000083, 0.05999999999999999778, 0.08000000000000000167, 0.1000000000000000056, 0.1199999999999999956, 0.1400000000000000133, 0.1600000000000000033, 0.1799999999999999933, 0.2000000000000000111, 0.2200000000000000011, 0.2399999999999999911, 0.2600000000000000089, 0.2800000000000000266, 0.2999999999999999889, 0.3200000000000000067, 0.3400000000000000244, 0.3599999999999999867, 0.3800000000000000044, 0.4000000000000000222, 0.4199999999999999845, 0.4400000000000000022, 0.4600000000000000200, 0.4799999999999999822, 0.5000000000000000000, 0.5200000000000000178, 0.5400000000000000355, 0.5600000000000000533, 0.5799999999999999600, 0.5999999999999999778, 0.6199999999999999956, 0.6400000000000000133, 0.6600000000000000311, 0.6800000000000000488, 0.6999999999999999556, 0.7199999999999999734, 0.7399999999999999911, 0.7600000000000000089, 0.7800000000000000266, 0.8000000000000000444, 0.8199999999999999512, 0.8399999999999999689, 0.8599999999999999867, 0.8800000000000000044, 0.9000000000000000222, 0.9200000000000000400, 0.9399999999999999467, 0.9599999999999999645, 0.9799999999999999822, 1.000000000000000000 ),
 .UNSPECIFIED. ) 
 GEOMETRIC_REPRESENTATION_ITEM ( )  RATIONAL_B_SPLINE_SURFACE ( (
 ( 1.000000000000000000, 0.9510565162951535312, 1.000000000000000000, 0.9510565162951535312, 1.000000000000000000, 0.9510565162951535312, 1.000000000000000000, 0.9510565162951535312, 1.000000000000000000, 0.9510565162951535312, 1.000000000000000000, 0.9510565162951535312, 1.000000000000000000, 0.9510565162951535312, 1.000000000000000000, 0.9510565162951535312, 1.000000000000000000, 0.9510565162951535312, 1.000000000000000000, 0.9510565162951535312, 1.000000000000000000, 0.9510565162951535312, 1.000000000000000000, 0.9510565162951535312, 1.000000000000000000, 0.9510565162951535312, 1.000000000000000000, 0.9510565162951535312, 1.000000000000000000, 0.9510565162951535312, 1.000000000000000000, 0.9510565162951535312, 1.000000000000000000, 0.9510565162951535312, 1.000000000000000000, 0.9510565162951535312, 1.000000000000000000, 0.9510565162951535312, 1.000000000000000000, 0.9510565162951535312, 1.000000000000000000, 0.9510565162951535312, 1.000000000000000000, 0.9510565162951535312, 1.000000000000000000, 0.9510565162951535312, 1.000000000000000000, 0.9510565162951535312, 1.000000000000000000, 0.9510565162951535312, 1.000000000000000000, 0.9510565162951535312, 1.000000000000000000, 0.9510565162951535312, 1.000000000000000000, 0.9510565162951535312, 1.000000000000000000, 0.9510565162951535312, 1.000000000000000000, 0.9510565162951535312, 1.000000000000000000, 0.9510565162951535312, 1.000000000000000000, 0.9510565162951535312, 1.000000000000000000, 0.9510565162951535312, 1.000000000000000000, 0.9510565162951535312, 1.000000000000000000, 0.9510565162951535312, 1.000000000000000000, 0.9510565162951535312, 1.000000000000000000, 0.9510565162951535312, 1.000000000000000000, 0.9510565162951535312, 1.000000000000000000, 0.9510565162951535312, 1.000000000000000000, 0.9510565162951535312, 1.000000000000000000, 0.9510565162951535312, 1.000000000000000000, 0.9510565162951535312, 1.000000000000000000, 0.9510565162951535312, 1.000000000000000000, 0.9510565162951535312, 1.000000000000000000, 0.9510565162951535312, 1.000000000000000000, 0.9510565162951535312, 1.000000000000000000, 0.9510565162951535312, 1.000000000000000000, 0.9510565162951535312, 1.000000000000000000, 0.9510565162951535312, 1.000000000000000000, 0.9510565162951535312, 1.000000000000000000),
 ( 1.000000000000000000, 0.9510565162951535312, 1.000000000000000000, 0.9510565162951535312, 1.000000000000000000, 0.9510565162951535312, 1.000000000000000000, 0.9510565162951535312, 1.000000000000000000, 0.9510565162951535312, 1.000000000000000000, 0.9510565162951535312, 1.000000000000000000, 0.9510565162951535312, 1.000000000000000000, 0.9510565162951535312, 1.000000000000000000, 0.9510565162951535312, 1.000000000000000000, 0.9510565162951535312, 1.000000000000000000, 0.9510565162951535312, 1.000000000000000000, 0.9510565162951535312, 1.000000000000000000, 0.9510565162951535312, 1.000000000000000000, 0.9510565162951535312, 1.000000000000000000, 0.9510565162951535312, 1.000000000000000000, 0.9510565162951535312, 1.000000000000000000, 0.9510565162951535312, 1.000000000000000000, 0.9510565162951535312, 1.000000000000000000, 0.9510565162951535312, 1.000000000000000000, 0.9510565162951535312, 1.000000000000000000, 0.9510565162951535312, 1.000000000000000000, 0.9510565162951535312, 1.000000000000000000, 0.9510565162951535312, 1.000000000000000000, 0.9510565162951535312, 1.000000000000000000, 0.9510565162951535312, 1.000000000000000000, 0.9510565162951535312, 1.000000000000000000, 0.9510565162951535312, 1.000000000000000000, 0.9510565162951535312, 1.000000000000000000, 0.9510565162951535312, 1.000000000000000000, 0.9510565162951535312, 1.000000000000000000, 0.9510565162951535312, 1.000000000000000000, 0.9510565162951535312, 1.000000000000000000, 0.9510565162951535312, 1.000000000000000000, 0.9510565162951535312, 1.000000000000000000, 0.9510565162951535312, 1.000000000000000000, 0.9510565162951535312, 1.000000000000000000, 0.9510565162951535312, 1.000000000000000000, 0.9510565162951535312, 1.000000000000000000, 0.9510565162951535312, 1.000000000000000000, 0.9510565162951535312, 1.000000000000000000, 0.9510565162951535312, 1.000000000000000000, 0.9510565162951535312, 1.000000000000000000, 0.9510565162951535312, 1.000000000000000000, 0.9510565162951535312, 1.000000000000000000, 0.9510565162951535312, 1.000000000000000000, 0.9510565162951535312, 1.000000000000000000, 0.9510565162951535312, 1.000000000000000000, 0.9510565162951535312, 1.000000000000000000, 0.9510565162951535312, 1.000000000000000000, 0.9510565162951535312, 1.000000000000000000) ) ) 
 REPRESENTATION_ITEM ( '' )  SURFACE ( )  );
#5068 = CARTESIAN_POINT ( 'NONE',  ( -10.37757302488624411, 28.72500000273120335, -31.93888565452638417 ) ) ;
#5069 = CARTESIAN_POINT ( 'NONE',  ( -33.58253175000000113, 77.12500000273118417, 0.000000000000000000 ) ) ;
#5070 = CARTESIAN_POINT ( 'NONE',  ( 27.16883889988624290, 36.17500000273120264, 19.73931689729373673 ) ) ;
#5071 = CARTESIAN_POINT ( 'NONE',  ( -10.37757302488623701, 23.77500000273119340, 31.93888565452638417 ) ) ;
#5072 = CARTESIAN_POINT ( 'NONE',  ( -24.50000000000000711, 7.100000000000008527, 7.960532557706201828 ) ) ;
#5073 = CARTESIAN_POINT ( 'NONE',  ( 19.06425588902592239, 46.09413166759064495, 19.11951029504763611 ) ) ;
#5074 = CARTESIAN_POINT ( 'NONE',  ( 27.16883889988624290, 77.92500000273116711, 19.73931689729373673 ) ) ;
#5075 = CARTESIAN_POINT ( 'NONE',  ( -32.50000000000000000, 26.40000000546236691, -10.55989012756945300 ) ) ;
#5076 = CARTESIAN_POINT ( 'NONE',  ( 10.04305231718578817, 61.39999999999999858, -30.90933677959249337 ) ) ;
#5077 = FACE_OUTER_BOUND ( 'NONE', #6052, .T. ) ;
#5078 = CARTESIAN_POINT ( 'NONE',  ( -33.58253175000000113, 63.22500000273119269, 10.91162601494193929 ) ) ;
#5079 = VECTOR ( 'NONE', #2791, 1000.000000000000000 ) ;
#5080 = CARTESIAN_POINT ( 'NONE',  ( 7.236395654485755280, 10.72499999726880837, 22.27133577429736988 ) ) ;
#5081 = CARTESIAN_POINT ( 'NONE',  ( 33.58253175000000113, 70.37500000273121259, -4.112674001490185761E-15 ) ) ;
#5082 = CARTESIAN_POINT ( 'NONE',  ( 10.37757302488624056, 6.525000002731207616, -31.93888565452638417 ) ) ;
#5083 = CARTESIAN_POINT ( 'NONE',  ( -27.16883889988623935, 65.57500000273118701, 19.73931689729374739 ) ) ;
#5084 = CARTESIAN_POINT ( 'NONE',  ( -23.41746825000000598, 16.22499999726880304, 7.608796670333726198 ) ) ;
#5085 = CARTESIAN_POINT ( 'NONE',  ( -13.94119854578936923, 17.01861083425731280, -24.22776226481241224 ) ) ;
#5086 = VERTEX_POINT ( 'NONE', #16273 ) ;
#5087 = CARTESIAN_POINT ( 'NONE',  ( -20.75514604977248112, 45.42500000273119554, 28.56700777964554661 ) ) ;
#5088 = ORIENTED_EDGE ( 'NONE', *, *, #12201, .F. ) ;
#5089 = CARTESIAN_POINT ( 'NONE',  ( 20.50609665441005092, 41.21875000000000000, 20.50609665440969209 ) ) ;
#5090 = CARTESIAN_POINT ( 'NONE',  ( 0.000000000000000000, 52.00000000000000711, 0.000000000000000000 ) ) ;
#5091 = CARTESIAN_POINT ( 'NONE',  ( -20.08610463437156923, 6.800000005462376151, 27.64615127144130113 ) ) ;
#5092 = CARTESIAN_POINT ( 'NONE',  ( 32.50000000000000711, 27.40000000546239534, 10.55989012756945122 ) ) ;
#5093 = CARTESIAN_POINT ( 'NONE',  ( -7.236395654485757944, 3.724999997268802154, -22.27133577429736988 ) ) ;
#5094 = CARTESIAN_POINT ( 'NONE',  ( -23.41746824999999887, 15.62499999726882294, -2.867812753649727150E-15 ) ) ;
#5095 = CARTESIAN_POINT ( 'NONE',  ( 27.16883889988623935, 16.57500000273118346, -19.73931689729374384 ) ) ;
#5096 = CARTESIAN_POINT ( 'NONE',  ( 26.29305231718579350, 21.30000000546239391, 19.10302069950537529 ) ) ;
#5097 = AXIS2_PLACEMENT_3D ( 'NONE', #18673, #13518, #29283 ) ;
#5098 = CARTESIAN_POINT ( 'NONE',  ( -20.08610463437156923, 64.29999999999996874, 27.64615127144130113 ) ) ;
#5099 = CARTESIAN_POINT ( 'NONE',  ( -4.223320258572819786E-15, 11.24999999453763344, 24.50000000000000000 ) ) ;
#5100 = CARTESIAN_POINT ( 'NONE',  ( -20.50609665440969209, 14.57812499999999645, 20.50609665441005092 ) ) ;
#5101 = CARTESIAN_POINT ( 'NONE',  ( 13.91746825000000065, 80.27500000273117564, 4.522059556121114987 ) ) ;
#5102 = CARTESIAN_POINT ( 'NONE',  ( -15.01150461594595775, 41.93489583333333570, 26.00068869287368756 ) ) ;
#5103 = PRODUCT_CONTEXT ( 'NONE', #5706, 'mechanical' ) ;
#5104 = VECTOR ( 'NONE', #7934, 1000.000000000000000 ) ;
#5105 = DIRECTION ( 'NONE',  ( -0.000000000000000000, 1.000000000000000000, -0.000000000000000000 ) ) ;
#5106 = CARTESIAN_POINT ( 'NONE',  ( 7.236395654485755280, 14.72499999726881192, 22.27133577429736988 ) ) ;
#5107 = CARTESIAN_POINT ( 'NONE',  ( -26.29305231718578995, 10.19999999999998685, 19.10302069950538595 ) ) ;
#5108 = CARTESIAN_POINT ( 'NONE',  ( 5.147494310547434893, 17.05125428700922541, 32.49999999999999289 ) ) ;
#5109 = CARTESIAN_POINT ( 'NONE',  ( 13.94119854578893580, 52.52826416574268364, -24.22776226481265383 ) ) ;
#5110 = CARTESIAN_POINT ( 'NONE',  ( -10.37757302488624411, 52.72500000273119980, -31.93888565452638417 ) ) ;
#5111 = CARTESIAN_POINT ( 'NONE',  ( -33.58253175000000113, 55.47500000273119980, 10.91162601494193929 ) ) ;
#5112 = CARTESIAN_POINT ( 'NONE',  ( -10.37757302488623701, 43.77500000273118275, 31.93888565452638417 ) ) ;
#5113 = CARTESIAN_POINT ( 'NONE',  ( 5.779280353836490358E-15, 23.00000000546237899, 32.49999999999999289 ) ) ;
#5114 = CARTESIAN_POINT ( 'NONE',  ( 2.445080149700053643E-15, 74.50000000000001421, 15.00000000000000000 ) ) ;
#5115 = CARTESIAN_POINT ( 'NONE',  ( -7.570916362186210335, 8.599999999999996092, -23.30088464923126779 ) ) ;
#5116 = DIRECTION ( 'NONE',  ( 0.000000000000000000, 0.000000000000000000, -1.000000000000000000 ) ) ;
#5117 = CARTESIAN_POINT ( 'NONE',  ( 6.277390505771533514E-15, 76.50000000000001421, 34.17252228774368916 ) ) ;
#5118 = CARTESIAN_POINT ( 'NONE',  ( -10.37757302488623701, 15.52500000273120051, 31.93888565452638417 ) ) ;
#5119 = CARTESIAN_POINT ( 'NONE',  ( 10.04305231718578817, 7.400000000000018119, -30.90933677959249337 ) ) ;
#5120 = DIRECTION ( 'NONE',  ( -1.000000000000000000, 0.000000000000000000, -0.000000000000000000 ) ) ;
#5121 = CARTESIAN_POINT ( 'NONE',  ( 15.14183272437242067, 11.70000000000000817, 20.84094480462498211 ) ) ;
#5122 = CARTESIAN_POINT ( 'NONE',  ( 13.94119854578893580, 18.15326416574268720, -24.22776226481265383 ) ) ;
#5123 = CARTESIAN_POINT ( 'NONE',  ( 10.04305231718579705, 37.10000000546239107, 30.90933677959248982 ) ) ;
#5124 = CARTESIAN_POINT ( 'NONE',  ( -7.570916362186210335, 10.34999999453761710, -23.30088464923126779 ) ) ;
#5125 = CARTESIAN_POINT ( 'NONE',  ( 27.16883889988624290, 25.92500000273118133, 19.73931689729373673 ) ) ;
#5126 = CARTESIAN_POINT ( 'NONE',  ( 13.97622843553633665, 41.36197916666666430, 24.20753774853730889 ) ) ;
#5127 = PRODUCT_DEFINITION ( 'UNKNOWN', '', #30148, #27098 ) ;
#5128 = EDGE_LOOP ( 'NONE', ( #30565, #20332, #24416, #11247 ) ) ;
#5129 = CARTESIAN_POINT ( 'NONE',  ( 6.486482029760649416E-15, 61.62500000273118417, 35.31076352940723240 ) ) ;
#5130 = CARTESIAN_POINT ( 'NONE',  ( -30.02300923189239512, 45.94531249999997868, 2.654126918244515359E-13 ) ) ;
#5131 = ORIENTED_EDGE ( 'NONE', *, *, #16178, .T. ) ;
#5132 = CARTESIAN_POINT ( 'NONE',  ( 26.00068869287340334, 16.44010416666666430, -15.01150461594642316 ) ) ;
#5133 = CARTESIAN_POINT ( 'NONE',  ( 7.468012846824777284, 18.88059000092397355, 28.02196122052045268 ) ) ;
#5134 = CARTESIAN_POINT ( 'NONE',  ( -10.37757302488623701, 5.525000002731192517, 31.93888565452638417 ) ) ;
#5135 = CARTESIAN_POINT ( 'NONE',  ( 7.236395654485755280, 2.224999997268800378, 22.27133577429736988 ) ) ;
#5136 = CARTESIAN_POINT ( 'NONE',  ( 10.37757302488624056, 36.77500000273120406, -31.93888565452638417 ) ) ;
#5137 = CARTESIAN_POINT ( 'NONE',  ( -26.29305231718578995, 38.70000000546236407, 19.10302069950538595 ) ) ;
#5138 = CARTESIAN_POINT ( 'NONE',  ( -9.270509831248421762, 74.29999999999999716, 12.75976212528060039 ) ) ;
#5139 = CARTESIAN_POINT ( 'NONE',  ( 7.505752307972854531, 64.13541666666667140, -28.01184896238303423 ) ) ;
#5140 = CARTESIAN_POINT ( 'NONE',  ( -33.58253175000000113, 25.12500000273118417, 0.000000000000000000 ) ) ;
#5141 = CARTESIAN_POINT ( 'NONE',  ( 5.147494310547434893, 76.55125428154684641, 32.49999999999999289 ) ) ;
#5142 = CARTESIAN_POINT ( 'NONE',  ( -10.37757302488624411, 48.97500000273119269, -31.93888565452638417 ) ) ;
#5143 = PRESENTATION_STYLE_ASSIGNMENT (( #12870 ) ) ;
#5144 = CARTESIAN_POINT ( 'NONE',  ( -32.50000000000000000, 30.10000000000000853, 10.55989012756946366 ) ) ;
#5145 = CARTESIAN_POINT ( 'NONE',  ( -32.50000000000000000, 27.89999999999999147, -10.55989012756945478 ) ) ;
#5146 = CARTESIAN_POINT ( 'NONE',  ( -24.50000000000001066, 7.100000000000007638, 7.960532557706201828 ) ) ;
#5147 = CARTESIAN_POINT ( 'NONE',  ( 33.58253175000000113, 72.12500000273119838, -4.112674001490185761E-15 ) ) ;
#5148 = CARTESIAN_POINT ( 'NONE',  ( -8.446640517145639571E-15, 78.49999999999998579, 32.49999999999999289 ) ) ;
#5149 = CLOSED_SHELL ( 'NONE', ( #16079, #9447, #29369, #3340, #123, #2667, #9646, #28558, #31037 ) ) ;
#5150 = CARTESIAN_POINT ( 'NONE',  ( -8.724778166670336788, 73.99999999999997158, -12.10690039861944278 ) ) ;
#5151 = CARTESIAN_POINT ( 'NONE',  ( 33.58253175000000113, 58.47500000273119269, -10.91162601494193574 ) ) ;
#5152 = AXIS2_PLACEMENT_3D ( 'NONE', #1928, #4170, #32809 ) ;
#5153 = CARTESIAN_POINT ( 'NONE',  ( -32.50000000000000000, 40.50000000546238965, 0.000000000000000000 ) ) ;
#5154 = CARTESIAN_POINT ( 'NONE',  ( -2.162160676586881955E-15, 10.62500000273119127, -35.31076352940723240 ) ) ;
#5155 = CARTESIAN_POINT ( 'NONE',  ( -19.11951029504763611, 29.76600666759063429, 19.06425588902592239 ) ) ;
#5156 = CARTESIAN_POINT ( 'NONE',  ( 10.28315354913682356, 66.99999999999998579, -31.56665548893539963 ) ) ;
#5157 = CARTESIAN_POINT ( 'NONE',  ( 33.58253175000000113, 4.475000002731182924, -10.91162601494193574 ) ) ;
#5158 = CARTESIAN_POINT ( 'NONE',  ( -27.16883889988623935, 33.32500000273118701, 19.73931689729374739 ) ) ;
#5159 = CARTESIAN_POINT ( 'NONE',  ( 20.08610463437158344, 45.20000000546238539, 27.64615127144129403 ) ) ;
#5160 = LINE ( 'NONE', #26436, #9498 ) ;
#5161 = CARTESIAN_POINT ( 'NONE',  ( -11.25946833292375793, 76.67500000273119554, -8.180482586598733619 ) ) ;
#5162 = CARTESIAN_POINT ( 'NONE',  ( -14.97647472619899389, 50.80951416574269075, 26.02091320914878025 ) ) ;
#5163 = CARTESIAN_POINT ( 'NONE',  ( -32.50000000000000000, 54.50000000546238965, 0.000000000000000000 ) ) ;
#5164 = CARTESIAN_POINT ( 'NONE',  ( -13.91746824999999532, 77.47500000273117848, 4.522059556121122093 ) ) ;
#5165 = FACE_OUTER_BOUND ( 'NONE', #24170, .T. ) ;
#5166 = CARTESIAN_POINT ( 'NONE',  ( 6.988114217767829928, 19.44791666666666075, -26.07999730980489872 ) ) ;
#5167 =( BOUNDED_CURVE ( )  B_SPLINE_CURVE ( 2, ( #26912, #652, #29316, #32055, #23851, #3246, #5650, #11141, #24349, #13379, #8555, #26753, #28984 ),
 .UNSPECIFIED., .F., .T. ) 
 B_SPLINE_CURVE_WITH_KNOTS ( ( 3, 2, 2, 2, 2, 2, 3 ),
 ( 0.3012820512820512664, 0.3025641025641025439, 0.3051282051282051544, 0.3076923076923077094, 0.3102564102564102644, 0.3128205128205128194, 0.3141025641025640969 ),
 .UNSPECIFIED. ) 
 CURVE ( )  GEOMETRIC_REPRESENTATION_ITEM ( )  RATIONAL_B_SPLINE_CURVE ( ( 0.9755282581475768211, 0.9755282581475768211, 1.000000000000000000, 0.9510565162951535312, 1.000000000000000000, 0.9510565162951535312, 1.000000000000000000, 0.9510565162951535312, 1.000000000000000000, 0.9510565162951535312, 1.000000000000000000, 0.9755282581475768211, 0.9755282581475768211 ) ) 
 REPRESENTATION_ITEM ( '' )  );
#5168 = CARTESIAN_POINT ( 'NONE',  ( -1.778240108872766143E-15, 64.00000000546238255, -32.49999999999999289 ) ) ;
#5169 = CARTESIAN_POINT ( 'NONE',  ( -32.50000000000000000, 70.50000000546238255, 0.000000000000000000 ) ) ;
#5170 = CARTESIAN_POINT ( 'NONE',  ( -15.01150461594642138, 25.89322916666666430, -26.00068869287340334 ) ) ;
#5171 = EDGE_CURVE ( 'NONE', #12166, #33526, #21422, .T. ) ;
#5172 = CARTESIAN_POINT ( 'NONE',  ( -33.58253175000000113, 33.37500000273117706, 0.000000000000000000 ) ) ;
#5173 =( BOUNDED_CURVE ( )  B_SPLINE_CURVE ( 2, ( #4852, #15333, #25788, #1579, #14642, #25102, #12056, #32977, #8265, #5022, #5197, #26130, #197 ),
 .UNSPECIFIED., .F., .T. ) 
 B_SPLINE_CURVE_WITH_KNOTS ( ( 3, 2, 2, 2, 2, 2, 3 ),
 ( 0.7371794871794872250, 0.7384615384615385025, 0.7410256410256410575, 0.7435897435897436125, 0.7461538461538461675, 0.7487179487179487225, 0.7500000000000000000 ),
 .UNSPECIFIED. ) 
 CURVE ( )  GEOMETRIC_REPRESENTATION_ITEM ( )  RATIONAL_B_SPLINE_CURVE ( ( 0.9755282581475768211, 0.9755282581475768211, 1.000000000000000000, 0.9510565162951535312, 1.000000000000000000, 0.9510565162951535312, 1.000000000000000000, 0.9510565162951535312, 1.000000000000000000, 0.9510565162951535312, 1.000000000000000000, 0.9755282581475768211, 0.9755282581475768211 ) ) 
 REPRESENTATION_ITEM ( '' )  );
#5174 = CARTESIAN_POINT ( 'NONE',  ( -18.94512977948575738, 7.924999997268811214, -13.76444248337723231 ) ) ;
#5175 = VERTEX_POINT ( 'NONE', #14021 ) ;
#5176 = CARTESIAN_POINT ( 'NONE',  ( -20.47846945139902175, 37.50038166759063074, -20.53372385742072481 ) ) ;
#5177 = CARTESIAN_POINT ( 'NONE',  ( -26.29305231718579350, 22.30000000546237970, -19.10302069950537884 ) ) ;
#5178 = EDGE_CURVE ( 'NONE', #6369, #7411, #5928, .T. ) ;
#5179 = CARTESIAN_POINT ( 'NONE',  ( -20.50609665441004736, 46.37500000000000000, -20.50609665440969565 ) ) ;
#5180 = CARTESIAN_POINT ( 'NONE',  ( -30.02300923189239512, 63.13281250000000000, 2.654126918244515359E-13 ) ) ;
#5181 = CARTESIAN_POINT ( 'NONE',  ( -2.162160676586881955E-15, 50.87500000273119838, -35.31076352940723240 ) ) ;
#5182 = CARTESIAN_POINT ( 'NONE',  ( 20.08610463437158344, 59.20000000546237828, 27.64615127144129403 ) ) ;
#5183 = CARTESIAN_POINT ( 'NONE',  ( 3.778760231354629433E-15, 2.249999994537632553, -24.50000000000000355 ) ) ;
#5184 = CARTESIAN_POINT ( 'NONE',  ( -33.58253175000000113, 45.02500000273117564, -10.91162601494193218 ) ) ;
#5185 = CARTESIAN_POINT ( 'NONE',  ( -15.00000000000000000, 72.00000000000001421, 0.000000000000000000 ) ) ;
#5186 = CARTESIAN_POINT ( 'NONE',  ( 6.486482029760649416E-15, 69.87500000273121259, 35.31076352940723240 ) ) ;
#5187 = DIRECTION ( 'NONE',  ( -0.8660254037844369313, -0.5000000000000028866, 1.060575238724904943E-16 ) ) ;
#5188 = CARTESIAN_POINT ( 'NONE',  ( -33.58253175000000113, 63.02500000273118985, -10.91162601494193041 ) ) ;
#5189 = ADVANCED_FACE ( 'NONE', ( #16766 ), #14188, .F. ) ;
#5190 = CARTESIAN_POINT ( 'NONE',  ( -28.01184896238304134, 22.02604166666666430, -7.505752307972844761 ) ) ;
#5191 = CARTESIAN_POINT ( 'NONE',  ( -2.092463501923844636E-15, 49.50000000000001421, -34.17252228774368916 ) ) ;
#5192 = CARTESIAN_POINT ( 'NONE',  ( 7.236395654485755280, 2.224999997268800378, 22.27133577429736988 ) ) ;
#5193 = CARTESIAN_POINT ( 'NONE',  ( -20.75514604977248823, 9.075000002731183457, -28.56700777964554305 ) ) ;
#5194 = CARTESIAN_POINT ( 'NONE',  ( -24.18731323226221974, 37.34597249907603356, 14.01125832528330406 ) ) ;
#5195 = CARTESIAN_POINT ( 'NONE',  ( -13.91746824999999532, 79.47500000273117848, 4.522059556121122093 ) ) ;
#5196 = CARTESIAN_POINT ( 'NONE',  ( 20.75514604977248467, 76.67500000273116711, -28.56700777964554305 ) ) ;
#5197 = CARTESIAN_POINT ( 'NONE',  ( -10.04305231718579172, 21.60000000000000853, -30.90933677959248982 ) ) ;
#5198 = CARTESIAN_POINT ( 'NONE',  ( -10.37757302488623701, 77.77500000273117564, 31.93888565452638417 ) ) ;
#5199 = ORIENTED_EDGE ( 'NONE', *, *, #13566, .T. ) ;
#5200 = CARTESIAN_POINT ( 'NONE',  ( 0.000000000000000000, 80.00000000000001421, 0.000000000000000000 ) ) ;
#5201 = AXIS2_PLACEMENT_3D ( 'NONE', #9756, #9587, #15086 ) ;
#5202 = CARTESIAN_POINT ( 'NONE',  ( 13.97622843553589966, 57.40364583333333570, -24.20753774853756113 ) ) ;
#5203 = CARTESIAN_POINT ( 'NONE',  ( -33.58253175000000113, 51.22500000273119269, 10.91162601494193929 ) ) ;
#5204 = CARTESIAN_POINT ( 'NONE',  ( -10.37757302488624411, 14.97500000273120691, -31.93888565452638417 ) ) ;
#5205 = CARTESIAN_POINT ( 'NONE',  ( -2.162160676586881955E-15, 78.62500000273115575, -35.31076352940723240 ) ) ;
#5206 = CARTESIAN_POINT ( 'NONE',  ( 27.95245687107223276, 40.78906249999999289, -2.463307335887066074E-13 ) ) ;
#5207 = CARTESIAN_POINT ( 'NONE',  ( 15.04653450569292872, 27.90402750092397355, -25.98046417659857710 ) ) ;
#5208 = CARTESIAN_POINT ( 'NONE',  ( -28.02196122052058413, 17.15065999907602290, -7.468012846824272799 ) ) ;
#5209 = CARTESIAN_POINT ( 'NONE',  ( -26.29305231718579350, 72.30000000546236549, -19.10302069950537884 ) ) ;
#5210 = CARTESIAN_POINT ( 'NONE',  ( 24.50000000000000000, 0.000000000000000000, 0.000000000000000000 ) ) ;
#5211 = CARTESIAN_POINT ( 'NONE',  ( 27.16883889988624290, 37.92500000273118843, 19.73931689729373673 ) ) ;
#5212 = CARTESIAN_POINT ( 'NONE',  ( 23.41746824999999887, 10.62499999726881938, 0.000000000000000000 ) ) ;
#5213 = DIRECTION ( 'NONE',  ( -0.000000000000000000, 1.000000000000000000, -0.000000000000000000 ) ) ;
#5214 = VERTEX_POINT ( 'NONE', #19179 ) ;
#5215 = CARTESIAN_POINT ( 'NONE',  ( -10.37757302488624411, 54.97500000273118559, -31.93888565452638417 ) ) ;
#5216 = CARTESIAN_POINT ( 'NONE',  ( -2.375766604868041476, 70.69874572391553613, 14.99999999999999822 ) ) ;
#5217 = CARTESIAN_POINT ( 'NONE',  ( -13.94119854578936923, 41.08111083425730214, -24.22776226481241224 ) ) ;
#5218 = CARTESIAN_POINT ( 'NONE',  ( 27.16883889988623935, 76.57500000273120122, -19.73931689729374384 ) ) ;
#5219 = VERTEX_POINT ( 'NONE', #13693 ) ;
#5220 = CARTESIAN_POINT ( 'NONE',  ( -20.75514604977248112, 25.42500000273119198, 28.56700777964554661 ) ) ;
#5221 = FACE_OUTER_BOUND ( 'NONE', #20420, .T. ) ;
#5222 = MECHANICAL_DESIGN_GEOMETRIC_PRESENTATION_REPRESENTATION (  '', ( #26044 ), #27111 ) ;
#5223 = ORIENTED_EDGE ( 'NONE', *, *, #1782, .F. ) ;
#5224 = DIRECTION ( 'NONE',  ( 0.000000000000000000, -1.000000000000000000, 0.000000000000000000 ) ) ;
#5225 = CARTESIAN_POINT ( 'NONE',  ( 10.37757302488624056, 58.52500000273119696, -31.93888565452638417 ) ) ;
#5226 = CARTESIAN_POINT ( 'NONE',  ( -26.00068869287340334, 52.53385416666666430, 15.01150461594643382 ) ) ;
#5227 = CARTESIAN_POINT ( 'NONE',  ( -3.880418787951146697, 6.301254276084462091, -24.49999999999999645 ) ) ;
#5228 = FACE_OUTER_BOUND ( 'NONE', #11535, .T. ) ;
#5229 = CARTESIAN_POINT ( 'NONE',  ( -2.162160676586881955E-15, 4.625000002731208149, -35.31076352940723240 ) ) ;
#5230 = CARTESIAN_POINT ( 'NONE',  ( -4.635254915624208216, 78.65000000546237402, 14.26584774442730463 ) ) ;
#5231 = CARTESIAN_POINT ( 'NONE',  ( 14.97647472619900455, 59.40326416574269075, -26.02091320914876960 ) ) ;
#5232 = FACE_OUTER_BOUND ( 'NONE', #22640, .T. ) ;
#5233 = DIRECTION ( 'NONE',  ( 0.000000000000000000, 0.000000000000000000, 1.000000000000000000 ) ) ;
#5234 = CARTESIAN_POINT ( 'NONE',  ( 32.50000000000000000, 75.50000000546236834, -3.980102097228898626E-15 ) ) ;
#5235 = CARTESIAN_POINT ( 'NONE',  ( -32.50000000000000000, 14.09999999999999254, 10.55989012756946366 ) ) ;
#5236 = CARTESIAN_POINT ( 'NONE',  ( 24.20753774853731244, 61.12760416666666430, -13.97622843553633132 ) ) ;
#5237 = CARTESIAN_POINT ( 'NONE',  ( 19.82091636218621389, 9.949999994537634507, -14.40073868116559197 ) ) ;
#5238 = CARTESIAN_POINT ( 'NONE',  ( 4.300734207923757602, 80.27500000273118985, -13.23629886949340673 ) ) ;
#5239 = CARTESIAN_POINT ( 'NONE',  ( 19.09188309203694800, 34.34374999999999289, 19.09188309203660694 ) ) ;
#5240 = EDGE_CURVE ( 'NONE', #33508, #17247, #20307, .T. ) ;
#5241 = CARTESIAN_POINT ( 'NONE',  ( 20.75514604977248467, 30.42500000273117777, -28.56700777964554305 ) ) ;
#5242 = PRODUCT_DEFINITION_SHAPE ( 'NONE', 'NONE',  #5127 ) ;
#5243 = CARTESIAN_POINT ( 'NONE',  ( 33.58253175000000113, 74.12500000273118417, -4.112674001490185761E-15 ) ) ;
#5244 = CARTESIAN_POINT ( 'NONE',  ( -20.75514604977248823, 37.07500000273120122, -28.56700777964554305 ) ) ;
#5245 = CARTESIAN_POINT ( 'NONE',  ( 10.37757302488624056, 14.77500000273118630, -31.93888565452638417 ) ) ;
#5246 = CARTESIAN_POINT ( 'NONE',  ( 3.445340210940985210E-14, 7.499999999999994671, 24.50000000000000000 ) ) ;
#5247 = CARTESIAN_POINT ( 'NONE',  ( 0.04044903254993986036, 51.68006916759063785, -27.95245687107223986 ) ) ;
#5248 = CARTESIAN_POINT ( 'NONE',  ( -33.58253175000000113, 73.22500000273117848, 10.91162601494193929 ) ) ;
#5249 = STYLED_ITEM ( 'NONE', ( #14594 ), #10725 ) ;
#5250 = CARTESIAN_POINT ( 'NONE',  ( -10.04305231718579172, 57.60000000000000142, -30.90933677959248982 ) ) ;
#5251 = PLANE ( 'NONE',  #30889 ) ;
#5252 = CARTESIAN_POINT ( 'NONE',  ( -27.16883889988623935, 63.32500000273119412, 19.73931689729374739 ) ) ;
#5253 = CARTESIAN_POINT ( 'NONE',  ( -23.41746824999999887, 8.124999997268817609, -2.867812753649727150E-15 ) ) ;
#5254 = CARTESIAN_POINT ( 'NONE',  ( -20.75514604977248112, 75.67500000273118133, 28.56700777964554661 ) ) ;
#5255 = CARTESIAN_POINT ( 'NONE',  ( 33.58253175000000823, 6.025000002731191628, 10.91162601494192685 ) ) ;
#5256 = VECTOR ( 'NONE', #30579, 1000.000000000000114 ) ;
#5257 = CARTESIAN_POINT ( 'NONE',  ( -7.236395654485757944, 3.224999997268801266, -22.27133577429736988 ) ) ;
#5258 = CARTESIAN_POINT ( 'NONE',  ( 0.04044903254993986036, 13.86756916759064318, -27.95245687107223986 ) ) ;
#5259 = EDGE_LOOP ( 'NONE', ( #28388, #30221, #18020, #27449 ) ) ;
#5260 = CARTESIAN_POINT ( 'NONE',  ( -10.37757302488624411, 42.72500000273119980, -31.93888565452638417 ) ) ;
#5261 = ORIENTED_EDGE ( 'NONE', *, *, #32118, .F. ) ;
#5262 = CARTESIAN_POINT ( 'NONE',  ( -7.505752307973343918, 43.22395833333332860, -28.01184896238290989 ) ) ;
#5263 = CARTESIAN_POINT ( 'NONE',  ( 5.779280353836490358E-15, 30.49999999999999645, 32.49999999999999289 ) ) ;
#5264 = CARTESIAN_POINT ( 'NONE',  ( 32.50000000000000000, 7.500000005462373664, -3.980102097228898626E-15 ) ) ;
#5265 = FACE_OUTER_BOUND ( 'NONE', #17203, .T. ) ;
#5266 = CARTESIAN_POINT ( 'NONE',  ( 20.50609665440969565, 23.17187499999999289, -20.50609665441004736 ) ) ;
#5267 = CARTESIAN_POINT ( 'NONE',  ( -19.82091636218621389, 1.200000000000006617, 14.40073868116558842 ) ) ;
#5268 = CARTESIAN_POINT ( 'NONE',  ( 33.58253175000000113, 14.47500000273118737, -10.91162601494193751 ) ) ;
#5269 =( BOUNDED_CURVE ( )  B_SPLINE_CURVE ( 2, ( #20754, #21423, #27226, #16275, #3059, #8359, #799, #11281, #13694, #5793, #29458, #3720, #19016 ),
 .UNSPECIFIED., .F., .T. ) 
 B_SPLINE_CURVE_WITH_KNOTS ( ( 3, 2, 2, 2, 2, 2, 3 ),
 ( 0.6217948717948718063, 0.6230769230769230838, 0.6256410256410256387, 0.6282051282051281937, 0.6307692307692307487, 0.6333333333333333037, 0.6346153846153845812 ),
 .UNSPECIFIED. ) 
 CURVE ( )  GEOMETRIC_REPRESENTATION_ITEM ( )  RATIONAL_B_SPLINE_CURVE ( ( 0.9755282581475768211, 0.9755282581475768211, 1.000000000000000000, 0.9510565162951535312, 1.000000000000000000, 0.9510565162951535312, 1.000000000000000000, 0.9510565162951535312, 1.000000000000000000, 0.9510565162951535312, 1.000000000000000000, 0.9755282581475768211, 0.9755282581475768211 ) ) 
 REPRESENTATION_ITEM ( '' )  );
#5270 = CARTESIAN_POINT ( 'NONE',  ( 32.50000000000000000, 56.99999999999999289, -3.980102097228898626E-15 ) ) ;
#5271 = DIRECTION ( 'NONE',  ( -1.224646799147353454E-16, 1.000000000000000000, -0.000000000000000000 ) ) ;
#5272 = DIRECTION ( 'NONE',  ( 0.000000000000000000, 0.000000000000000000, 1.000000000000000000 ) ) ;
#5273 = CARTESIAN_POINT ( 'NONE',  ( -28.02196122052058413, 37.77565999907600514, -7.468012846824272799 ) ) ;
#5274 = CARTESIAN_POINT ( 'NONE',  ( -13.91746824999999532, 75.47500000273116427, 4.522059556121122093 ) ) ;
#5275 = CARTESIAN_POINT ( 'NONE',  ( -26.00068869287368756, 42.79427083333332149, -15.01150461594595775 ) ) ;
#5276 = CARTESIAN_POINT ( 'NONE',  ( 0.000000000000000000, 0.000000000000000000, 24.50000000000000000 ) ) ;
#5277 = CARTESIAN_POINT ( 'NONE',  ( -7.570916362186210335, 12.59999999999999964, -23.30088464923126779 ) ) ;
#5278 = CARTESIAN_POINT ( 'NONE',  ( -20.08610463437157989, 3.699999999999999289, -27.64615127144129758 ) ) ;
#5279 = CARTESIAN_POINT ( 'NONE',  ( 20.08610463437157279, 17.80000000546237615, -27.64615127144129758 ) ) ;
#5280 = EDGE_CURVE ( 'NONE', #6391, #17247, #29124, .T. ) ;
#5281 = CARTESIAN_POINT ( 'NONE',  ( 27.95245687107223276, 63.41368083240934794, -0.04044903255042905932 ) ) ;
#5282 = CARTESIAN_POINT ( 'NONE',  ( -10.37757302488624411, 50.72500000273119980, -31.93888565452638417 ) ) ;
#5283 = CARTESIAN_POINT ( 'NONE',  ( -10.37757302488624411, 52.97500000273118559, -31.93888565452638417 ) ) ;
#5284 = CARTESIAN_POINT ( 'NONE',  ( -27.16883889988623935, 35.57500000273120122, 19.73931689729374739 ) ) ;
#5285 = DIRECTION ( 'NONE',  ( -0.6936844842780661713, 0.7202789989107508672, 0.000000000000000000 ) ) ;
#5286 = EDGE_CURVE ( 'NONE', #20029, #1088, #429, .T. ) ;
#5287 = CARTESIAN_POINT ( 'NONE',  ( -6.988114217767819270, 14.29166666666666430, 26.07999730980490583 ) ) ;
#5288 = CARTESIAN_POINT ( 'NONE',  ( -10.04305231718578462, 62.40000000000001279, 30.90933677959249337 ) ) ;
#5289 = CARTESIAN_POINT ( 'NONE',  ( 7.168475036913831033, 16.99999999999999289, -22.36265383151947361 ) ) ;
#5290 = CARTESIAN_POINT ( 'NONE',  ( -32.50000000000000000, 27.89999999999999147, -10.55989012756945300 ) ) ;
#5291 = CARTESIAN_POINT ( 'NONE',  ( -33.58253175000000113, 15.02500000273120051, -10.91162601494193218 ) ) ;
#5292 = CARTESIAN_POINT ( 'NONE',  ( -8.601468415847518756, 81.07500000273121543, -11.83890561707634603 ) ) ;
#5293 = DIRECTION ( 'NONE',  ( -0.000000000000000000, -1.000000000000000000, -0.000000000000000000 ) ) ;
#5294 = CARTESIAN_POINT ( 'NONE',  ( 0.000000000000000000, 80.00000000000001421, 0.000000000000000000 ) ) ;
#5295 = CARTESIAN_POINT ( 'NONE',  ( -13.94119854578892514, 19.87201416574269075, 24.22776226481266448 ) ) ;
#5296 = CARTESIAN_POINT ( 'NONE',  ( -32.50000000000000000, 36.40000000546236691, -10.55989012756945478 ) ) ;
#5297 = FACE_OUTER_BOUND ( 'NONE', #22765, .T. ) ;
#5298 = CARTESIAN_POINT ( 'NONE',  ( 27.16883889988624290, 23.92500000273117777, 19.73931689729373673 ) ) ;
#5299 = CARTESIAN_POINT ( 'NONE',  ( 19.09188309203694800, 41.21875000000000000, 19.09188309203660694 ) ) ;
#5300 = EDGE_LOOP ( 'NONE', ( #25430, #32275, #16038, #33271 ) ) ;
#5301 = CARTESIAN_POINT ( 'NONE',  ( 33.58253175000000113, 60.12500000273117706, -4.112674001490185761E-15 ) ) ;
#5302 = ORIENTED_EDGE ( 'NONE', *, *, #6221, .F. ) ;
#5303 = CARTESIAN_POINT ( 'NONE',  ( 7.505752307972854531, 19.44791666666666075, -28.01184896238303423 ) ) ;
#5304 = CARTESIAN_POINT ( 'NONE',  ( -0.04044903254990864921, 15.58631916759064495, 30.02300923189239867 ) ) ;
#5305 = CARTESIAN_POINT ( 'NONE',  ( -2.162160676586881955E-15, 4.625000002731192161, -35.31076352940723240 ) ) ;
#5306 = DIRECTION ( 'NONE',  ( -0.000000000000000000, 1.000000000000000000, -0.000000000000000000 ) ) ;
#5307 = VECTOR ( 'NONE', #15292, 1000.000000000000000 ) ;
#5308 = CARTESIAN_POINT ( 'NONE',  ( -20.75514604977248112, 33.67500000273119554, 28.56700777964554661 ) ) ;
#5309 =( BOUNDED_CURVE ( )  B_SPLINE_CURVE ( 2, ( #3256, #24191, #7169, #17651, #22124, #17309, #3921, #22618, #2023, #14902, #1330, #25366, #27430 ),
 .UNSPECIFIED., .F., .T. ) 
 B_SPLINE_CURVE_WITH_KNOTS ( ( 3, 2, 2, 2, 2, 2, 3 ),
 ( 0.5277777777777777901, 0.5333333333333333259, 0.5444444444444443976, 0.5555555555555555802, 0.5666666666666666519, 0.5777777777777777235, 0.5833333333333332593 ),
 .UNSPECIFIED. ) 
 CURVE ( )  GEOMETRIC_REPRESENTATION_ITEM ( )  RATIONAL_B_SPLINE_CURVE ( ( 0.9755282581475768211, 0.9755282581475768211, 1.000000000000000000, 0.9510565162951535312, 1.000000000000000000, 0.9510565162951535312, 1.000000000000000000, 0.9510565162951535312, 1.000000000000000000, 0.9510565162951535312, 1.000000000000000000, 0.9755282581475770431, 0.9755282581475768211 ) ) 
 REPRESENTATION_ITEM ( '' )  );
#5310 = CARTESIAN_POINT ( 'NONE',  ( -10.04305231718579172, 40.10000000546237686, -30.90933677959248982 ) ) ;
#5311 = FACE_OUTER_BOUND ( 'NONE', #33092, .T. ) ;
#5312 = DIRECTION ( 'NONE',  ( 0.2583678462756400229, 0.9660466117175129375, 3.164093559440580996E-17 ) ) ;
#5313 = CARTESIAN_POINT ( 'NONE',  ( -4.635254915624211769, 81.60000000000000853, -14.26584774442730286 ) ) ;
#5314 = CARTESIAN_POINT ( 'NONE',  ( -10.37757302488624411, 46.97500000273119269, -31.93888565452638417 ) ) ;
#5315 = AXIS2_PLACEMENT_3D ( 'NONE', #5554, #723, #11209 ) ;
#5316 = ORIENTED_EDGE ( 'NONE', *, *, #15607, .F. ) ;
#5317 = CARTESIAN_POINT ( 'NONE',  ( 10.04305231718578817, 21.39999999999998792, -30.90933677959249337 ) ) ;
#5318 = CARTESIAN_POINT ( 'NONE',  ( -10.04305231718579172, 25.60000000000001208, -30.90933677959248982 ) ) ;
#5319 = CARTESIAN_POINT ( 'NONE',  ( -15.14183272437241889, 4.699999999999995737, -20.84094480462497856 ) ) ;
#5320 = CARTESIAN_POINT ( 'NONE',  ( 10.37757302488624056, 72.52500000273120406, -31.93888565452638417 ) ) ;
#5321 = CARTESIAN_POINT ( 'NONE',  ( -32.98389303421630103, 66.99999999999998579, -5.656568564006192013 ) ) ;
#5322 = CARTESIAN_POINT ( 'NONE',  ( 3.730319287574177523, 74.00000000000004263, -13.94370120449079842 ) ) ;
#5323 = CARTESIAN_POINT ( 'NONE',  ( 20.75514604977249178, 60.07500000273120122, 28.56700777964553950 ) ) ;
#5324 = CARTESIAN_POINT ( 'NONE',  ( 10.04305231718578817, 73.40000000000001990, -30.90933677959249337 ) ) ;
#5325 = CARTESIAN_POINT ( 'NONE',  ( 20.75514604977249178, 9.825000002731188786, 28.56700777964553950 ) ) ;
#5326 = CARTESIAN_POINT ( 'NONE',  ( 27.95245687107223986, 28.47694416759064495, 0.04044903254993640479 ) ) ;
#5327 = CARTESIAN_POINT ( 'NONE',  ( -11.64495469945077311, 66.99999999999998579, -31.50463004621152763 ) ) ;
#5328 = CARTESIAN_POINT ( 'NONE',  ( 6.486482029760648627E-15, 5.875000002731167292, 35.31076352940722529 ) ) ;
#5329 = CARTESIAN_POINT ( 'NONE',  ( 33.58253175000000113, 34.12500000273117706, -4.112674001490185761E-15 ) ) ;
#5330 = CARTESIAN_POINT ( 'NONE',  ( 10.04305231718578817, 45.90000000546237402, -30.90933677959249337 ) ) ;
#5331 = PLANE ( 'NONE',  #15000 ) ;
#5332 = CARTESIAN_POINT ( 'NONE',  ( 13.91746825000000065, 75.77500000273117564, 4.522059556121115875 ) ) ;
#5333 = CARTESIAN_POINT ( 'NONE',  ( 7.543491769121922985, 43.50482666574268364, 28.00173670424535644 ) ) ;
#5334 = CARTESIAN_POINT ( 'NONE',  ( 32.50000000000000000, 57.60000000546237686, -10.55989012756945833 ) ) ;
#5335 = CARTESIAN_POINT ( 'NONE',  ( -11.25946833292375793, 77.57500000273121543, 8.180482586598737171 ) ) ;
#5336 = CARTESIAN_POINT ( 'NONE',  ( -6.988114217767819270, 14.29166666666666430, 26.07999730980490583 ) ) ;
#5337 = CARTESIAN_POINT ( 'NONE',  ( 7.570916362186213000, 0.4000000000000114575, -23.30088464923126423 ) ) ;
#5338 = AXIS2_PLACEMENT_3D ( 'NONE', #15957, #311, #26413 ) ;
#5339 = CARTESIAN_POINT ( 'NONE',  ( 32.50000000000000000, 67.50000000546238255, -3.980102097228898626E-15 ) ) ;
#5340 = CARTESIAN_POINT ( 'NONE',  ( -26.00068869287340334, 25.03385416666666785, 15.01150461594643382 ) ) ;
#5341 = EDGE_CURVE ( 'NONE', #5934, #8435, #14584, .T. ) ;
#5342 = CARTESIAN_POINT ( 'NONE',  ( -27.16883889988623935, 27.57500000273117990, 19.73931689729374739 ) ) ;
#5343 = CARTESIAN_POINT ( 'NONE',  ( 1.507698388325705758E-15, 11.62499999726880340, -24.62258325217400312 ) ) ;
#5344 = ORIENTED_EDGE ( 'NONE', *, *, #32784, .T. ) ;
#5345 = CARTESIAN_POINT ( 'NONE',  ( -14.97647472619946285, 44.51861083425730214, -26.02091320914851025 ) ) ;
#5346 = CARTESIAN_POINT ( 'NONE',  ( 10.04305231718578817, 15.90000000546236336, -30.90933677959249337 ) ) ;
#5347 = CARTESIAN_POINT ( 'NONE',  ( 15.01150461594596308, 53.96614583333333570, -26.00068869287367335 ) ) ;
#5348 = CARTESIAN_POINT ( 'NONE',  ( -26.00068869287368756, 66.85677083333334281, -15.01150461594595775 ) ) ;
#5349 = CARTESIAN_POINT ( 'NONE',  ( -20.75514604977248112, 53.67500000273119554, 28.56700777964554661 ) ) ;
#5350 = CARTESIAN_POINT ( 'NONE',  ( 6.277390505771533514E-15, 57.00000000546238965, 34.17252228774368916 ) ) ;
#5351 = DIRECTION ( 'NONE',  ( 0.000000000000000000, -1.000000000000000000, 0.000000000000000000 ) ) ;
#5352 = CARTESIAN_POINT ( 'NONE',  ( 20.75514604977249178, 39.82500000273116569, 28.56700777964553950 ) ) ;
#5353 = DIRECTION ( 'NONE',  ( 0.000000000000000000, -0.000000000000000000, -1.000000000000000000 ) ) ;
#5354 = CARTESIAN_POINT ( 'NONE',  ( -2.162160676586881955E-15, 68.87500000273118417, -35.31076352940723240 ) ) ;
#5355 = CYLINDRICAL_SURFACE ( 'NONE', #32079, 9.000000000000001776 ) ;
#5356 = CARTESIAN_POINT ( 'NONE',  ( 33.58253175000000113, 64.12500000273118417, -4.112674001490185761E-15 ) ) ;
#5357 = CARTESIAN_POINT ( 'NONE',  ( -20.50609665441004736, 22.31250000000000000, -20.50609665440969565 ) ) ;
#5358 = CARTESIAN_POINT ( 'NONE',  ( -20.08610463437157989, 43.69999999999998863, -27.64615127144129758 ) ) ;
#5359 = CARTESIAN_POINT ( 'NONE',  ( -7.236395654485757944, 3.224999997268801266, -22.27133577429736988 ) ) ;
#5360 = CARTESIAN_POINT ( 'NONE',  ( -33.58253175000000113, 9.475000002731201576, 10.91162601494193929 ) ) ;
#5361 = CARTESIAN_POINT ( 'NONE',  ( 7.570916362186207671, 19.34999999453762598, 23.30088464923126779 ) ) ;
#5362 = CARTESIAN_POINT ( 'NONE',  ( 0.04044903255044120238, 33.33555583240935505, 27.95245687107223276 ) ) ;
#5363 = CARTESIAN_POINT ( 'NONE',  ( 8.601468415847516980, 74.67500000273118133, -11.83890561707634781 ) ) ;
#5364 = CARTESIAN_POINT ( 'NONE',  ( 2.445080149700053643E-15, 74.75000000546236834, 15.00000000000000000 ) ) ;
#5365 = CYLINDRICAL_SURFACE ( 'NONE', #18325, 32.50000000000000000 ) ;
#5366 = CARTESIAN_POINT ( 'NONE',  ( -2.162160676586881955E-15, 74.87500000273116996, -35.31076352940723240 ) ) ;
#5367 = VERTEX_POINT ( 'NONE', #14694 ) ;
#5368 = CARTESIAN_POINT ( 'NONE',  ( 1.507698388325705758E-15, 17.62499999726881938, -24.62258325217400312 ) ) ;
#5369 = CARTESIAN_POINT ( 'NONE',  ( -26.07999730980490583, 63.27604166666667140, -6.988114217767815717 ) ) ;
#5370 = CARTESIAN_POINT ( 'NONE',  ( -2.162160676586881955E-15, 52.62500000273117706, -35.31076352940723240 ) ) ;
#5371 = CARTESIAN_POINT ( 'NONE',  ( -20.75514604977248823, 19.07500000273118701, -28.56700777964554305 ) ) ;
#5372 = CARTESIAN_POINT ( 'NONE',  ( 33.58253175000000113, 2.375000002731192161, -4.112674001490185761E-15 ) ) ;
#5373 = CARTESIAN_POINT ( 'NONE',  ( -13.97622843553588901, 38.49739583333332860, 24.20753774853756823 ) ) ;
#5374 =( BOUNDED_CURVE ( )  B_SPLINE_CURVE ( 2, ( #14802, #22866, #17040, #20129, #6729, #11881, #12568, #33323, #4160, #17726, #14974, #9821, #23039 ),
 .UNSPECIFIED., .F., .F. ) 
 B_SPLINE_CURVE_WITH_KNOTS ( ( 3, 2, 2, 2, 2, 2, 3 ),
 ( 0.9166666666666666297, 0.9179487179487179072, 0.9205128205128204621, 0.9230769230769231282, 0.9256410256410256832, 0.9282051282051282382, 0.9294871794871795156 ),
 .UNSPECIFIED. ) 
 CURVE ( )  GEOMETRIC_REPRESENTATION_ITEM ( )  RATIONAL_B_SPLINE_CURVE ( ( 0.9755282581475768211, 0.9755282581475768211, 1.000000000000000000, 0.9510565162951535312, 1.000000000000000000, 0.9510565162951535312, 1.000000000000000000, 0.9510565162951535312, 1.000000000000000000, 0.9510565162951535312, 1.000000000000000000, 0.9755282581475768211, 0.9755282581475768211 ) ) 
 REPRESENTATION_ITEM ( '' )  );
#5375 = CARTESIAN_POINT ( 'NONE',  ( 14.97647472619947351, 29.04986083425730570, 26.02091320914850314 ) ) ;
#5376 = EDGE_CURVE ( 'NONE', #33486, #12563, #28952, .T. ) ;
#5377 = CARTESIAN_POINT ( 'NONE',  ( 20.47846945139867003, 14.85899333240935505, -20.53372385742107653 ) ) ;
#5378 = CARTESIAN_POINT ( 'NONE',  ( 32.50000000000000711, 73.40000000546234560, 10.55989012756945122 ) ) ;
#5379 = CARTESIAN_POINT ( 'NONE',  ( 33.37605761044780905, 52.00000000000002132, 0.2721180500512087597 ) ) ;
#5380 = CARTESIAN_POINT ( 'NONE',  ( -27.16883889988624290, 40.92500000273119554, -19.73931689729374028 ) ) ;
#5381 = CARTESIAN_POINT ( 'NONE',  ( 19.06425588902558133, 49.23399333240936215, -19.11951029504797006 ) ) ;
#5382 = CARTESIAN_POINT ( 'NONE',  ( -23.41746825000000243, 7.524999997268816188, -7.608796670333730638 ) ) ;
#5383 = EDGE_CURVE ( 'NONE', #20887, #28718, #27305, .T. ) ;
#5384 = LINE ( 'NONE', #18773, #8985 ) ;
#5385 = VERTEX_POINT ( 'NONE', #27561 ) ;
#5386 = CARTESIAN_POINT ( 'NONE',  ( -33.58253175000000113, 51.47500000273118559, 10.91162601494193929 ) ) ;
#5387 = CARTESIAN_POINT ( 'NONE',  ( -32.50000000000000000, 2.000000000000001776, 0.000000000000000000 ) ) ;
#5388 = CARTESIAN_POINT ( 'NONE',  ( -0.04044903254992426173, 43.08631916759065916, 27.95245687107223276 ) ) ;
#5389 = CARTESIAN_POINT ( 'NONE',  ( 33.58253175000000113, 74.47500000273116427, -10.91162601494193751 ) ) ;
#5390 = ORIENTED_EDGE ( 'NONE', *, *, #32068, .F. ) ;
#5391 = CARTESIAN_POINT ( 'NONE',  ( 33.58253175000000113, 26.12500000273119838, -4.112674001490185761E-15 ) ) ;
#5392 = EDGE_CURVE ( 'NONE', #1605, #9595, #30811, .T. ) ;
#5393 = CARTESIAN_POINT ( 'NONE',  ( -7.505752307973343918, 15.72395833333332860, -28.01184896238290989 ) ) ;
#5394 = AXIS2_PLACEMENT_3D ( 'NONE', #7674, #20220, #14893 ) ;
#5395 = VERTEX_POINT ( 'NONE', #11941 ) ;
#5396 = CARTESIAN_POINT ( 'NONE',  ( 5.779280353836490358E-15, 29.00000000546237544, 32.49999999999999289 ) ) ;
#5397 = CARTESIAN_POINT ( 'NONE',  ( -27.16883889988624290, 62.92500000273118843, -19.73931689729374028 ) ) ;
#5398 = CARTESIAN_POINT ( 'NONE',  ( 2.740863092043355209E-13, 51.96093750000000000, 30.02300923189239512 ) ) ;
#5399 = CARTESIAN_POINT ( 'NONE',  ( 19.82091636218621389, 16.19999999999999218, -14.40073868116559197 ) ) ;
#5400 = CARTESIAN_POINT ( 'NONE',  ( 23.41746824999999887, 9.124999997268817609, 0.000000000000000000 ) ) ;
#5401 = CARTESIAN_POINT ( 'NONE',  ( 10.37757302488624767, 1.725000002731180704, 31.93888565452638417 ) ) ;
#5402 = CARTESIAN_POINT ( 'NONE',  ( -10.37757302488624411, 32.97500000273117848, -31.93888565452638417 ) ) ;
#5403 = CARTESIAN_POINT ( 'NONE',  ( 30.02300923189239867, 59.97618083240934794, -0.04044903255044467877 ) ) ;
#5404 = LINE ( 'NONE', #19125, #17160 ) ;
#5405 = CARTESIAN_POINT ( 'NONE',  ( -32.50000000000000000, 60.09999999999999432, 10.55989012756946366 ) ) ;
#5406 = CARTESIAN_POINT ( 'NONE',  ( 32.50000000000000000, 15.09999999999998899, -10.55989012756945833 ) ) ;
#5407 = CARTESIAN_POINT ( 'NONE',  ( -24.20753774853756823, 56.54427083333332860, -13.97622843553588723 ) ) ;
#5408 = CARTESIAN_POINT ( 'NONE',  ( -7.570916362186215665, 19.14999999453761959, 23.30088464923126423 ) ) ;
#5409 = CARTESIAN_POINT ( 'NONE',  ( 9.270509831248425314, 72.95000000546238539, 12.75976212528059683 ) ) ;
#5410 = CARTESIAN_POINT ( 'NONE',  ( -19.09188309203660694, 31.76562499999999289, 19.09188309203694800 ) ) ;
#5411 = CARTESIAN_POINT ( 'NONE',  ( -10.37757302488623701, 23.52500000273119340, 31.93888565452638417 ) ) ;
#5412 = CARTESIAN_POINT ( 'NONE',  ( 20.75514604977248467, 72.42500000273119554, -28.56700777964554305 ) ) ;
#5413 = CARTESIAN_POINT ( 'NONE',  ( 10.37757302488624767, 37.97500000273119980, 31.93888565452638417 ) ) ;
#5414 = CARTESIAN_POINT ( 'NONE',  ( -33.58253175000000113, 15.37500000273117706, 0.000000000000000000 ) ) ;
#5415 = CARTESIAN_POINT ( 'NONE',  ( -2.375766604868045029, 79.55125428154684641, -14.99999999999999822 ) ) ;
#5416 = CARTESIAN_POINT ( 'NONE',  ( -7.025853678916393008, 53.54204833425730925, 26.06988505166735592 ) ) ;
#5417 = CARTESIAN_POINT ( 'NONE',  ( -20.75514604977248823, 76.82500000273120122, -28.56700777964554305 ) ) ;
#5418 = CARTESIAN_POINT ( 'NONE',  ( 15.14183272437242067, 7.699999999999988631, 20.84094480462498211 ) ) ;
#5419 = CARTESIAN_POINT ( 'NONE',  ( 20.08610463437158344, 52.69999999999998863, 27.64615127144129403 ) ) ;
#5420 = CARTESIAN_POINT ( 'NONE',  ( 23.95873412499999944, 0.3124999986344190184, 0.000000000000000000 ) ) ;
#5421 = CARTESIAN_POINT ( 'NONE',  ( -10.37757302488624411, 60.72500000273117848, -31.93888565452638417 ) ) ;
#5422 = CARTESIAN_POINT ( 'NONE',  ( -14.47279130897152122, 8.424999997268816543, 19.92008829642072243 ) ) ;
#5423 = ORIENTED_EDGE ( 'NONE', *, *, #14557, .F. ) ;
#5424 = CARTESIAN_POINT ( 'NONE',  ( -27.16883889988623935, 75.57500000273118701, 19.73931689729374739 ) ) ;
#5425 = CARTESIAN_POINT ( 'NONE',  ( -20.08610463437156923, 62.29999999999998295, 27.64615127144130113 ) ) ;
#5426 = CARTESIAN_POINT ( 'NONE',  ( 23.41746825000000243, 17.22499999726880304, -7.608796670333727974 ) ) ;
#5427 = CARTESIAN_POINT ( 'NONE',  ( 14.01125832528286352, 17.59152750092397355, -24.18731323226246843 ) ) ;
#5428 = EDGE_LOOP ( 'NONE', ( #13998, #19602, #11131, #16509 ) ) ;
#5429 = CARTESIAN_POINT ( 'NONE',  ( 10.37757302488624056, 40.52500000273119696, -31.93888565452638417 ) ) ;
#5430 = CARTESIAN_POINT ( 'NONE',  ( 3.469446951953614189E-15, -45.00000000000000000, 0.000000000000000000 ) ) ;
#5431 = EDGE_LOOP ( 'NONE', ( #9267, #30782, #18319, #8412 ) ) ;
#5432 = CARTESIAN_POINT ( 'NONE',  ( -20.50609665441004736, 46.37500000000000000, -20.50609665440969565 ) ) ;
#5433 = LINE ( 'NONE', #13672, #1824 ) ;
#5434 = CARTESIAN_POINT ( 'NONE',  ( 32.50000000000000000, 3.500000005462383434, -3.980102097228898626E-15 ) ) ;
#5435 = DIRECTION ( 'NONE',  ( -0.7071067811865526798, 0.000000000000000000, -0.7071067811865423547 ) ) ;
#5436 = CARTESIAN_POINT ( 'NONE',  ( 15.01150461594643204, 24.17447916666666785, 26.00068869287340334 ) ) ;
#5437 = CARTESIAN_POINT ( 'NONE',  ( 23.41746824999999887, 16.62499999726882294, 0.000000000000000000 ) ) ;
#5438 = CARTESIAN_POINT ( 'NONE',  ( 20.75514604977249178, 6.075000002731190563, 28.56700777964553950 ) ) ;
#5439 = CARTESIAN_POINT ( 'NONE',  ( -26.29305231718578995, 62.20000000000000284, 19.10302069950538595 ) ) ;
#5440 = CARTESIAN_POINT ( 'NONE',  ( -11.25946833292375793, 79.07500000273121543, 8.180482586598737171 ) ) ;
#5441 = CARTESIAN_POINT ( 'NONE',  ( -20.08610463437156923, 30.30000000000000426, 27.64615127144130113 ) ) ;
#5442 = CARTESIAN_POINT ( 'NONE',  ( -14.97647472619899389, 37.05951416574268364, 26.02091320914878025 ) ) ;
#5443 = CARTESIAN_POINT ( 'NONE',  ( -8.601468415847518756, 73.07500000273115859, -11.83890561707634781 ) ) ;
#5444 = CARTESIAN_POINT ( 'NONE',  ( 26.00068869287341045, 40.50260416666666430, -15.01150461594642493 ) ) ;
#5445 = CONTEXT_DEPENDENT_SHAPE_REPRESENTATION ( #17, #25172 ) ;
#5446 = CARTESIAN_POINT ( 'NONE',  ( -33.58253175000000113, 1.250000002731177506, 0.000000000000000000 ) ) ;
#5447 = DIRECTION ( 'NONE',  ( 0.000000000000000000, 0.000000000000000000, 1.000000000000000000 ) ) ;
#5448 = CARTESIAN_POINT ( 'NONE',  ( 26.29305231718578995, 3.199999999999980638, -19.10302069950538240 ) ) ;
#5449 = CARTESIAN_POINT ( 'NONE',  ( 0.000000000000000000, 80.00000000000001421, 0.000000000000000000 ) ) ;
#5450 = CARTESIAN_POINT ( 'NONE',  ( -26.09010956794245217, 61.83815999907601935, -6.950374756619243755 ) ) ;
#5451 = CARTESIAN_POINT ( 'NONE',  ( 10.37757302488624056, 48.52500000273118985, -31.93888565452638417 ) ) ;
#5452 = CARTESIAN_POINT ( 'NONE',  ( -9.270509831248421762, 70.55000000546240813, 12.75976212528060039 ) ) ;
#5453 = CARTESIAN_POINT ( 'NONE',  ( -10.37757302488623701, 55.77500000273121117, 31.93888565452638417 ) ) ;
#5454 = CARTESIAN_POINT ( 'NONE',  ( -20.75514604977248112, 31.67500000273119909, 28.56700777964554661 ) ) ;
#5455 = CARTESIAN_POINT ( 'NONE',  ( 32.50000000000000000, 23.60000000546236976, -10.55989012756945833 ) ) ;
#5456 = CARTESIAN_POINT ( 'NONE',  ( 6.988114217768294445, 17.44270833333333215, 26.07999730980477437 ) ) ;
#5457 = CARTESIAN_POINT ( 'NONE',  ( 10.04305231718579705, 15.10000000546238219, 30.90933677959248982 ) ) ;
#5458 = CARTESIAN_POINT ( 'NONE',  ( 20.08610463437157279, 51.80000000546237970, -27.64615127144129758 ) ) ;
#5459 = CARTESIAN_POINT ( 'NONE',  ( 6.277390505771533514E-15, 74.50000000000000000, 34.17252228774368916 ) ) ;
#5460 = CARTESIAN_POINT ( 'NONE',  ( 27.16883889988623935, 16.32500000273116925, -19.73931689729374384 ) ) ;
#5461 = CARTESIAN_POINT ( 'NONE',  ( 1.507698388325705758E-15, 1.124999997268814722, -24.62258325217400312 ) ) ;
#5462 = CYLINDRICAL_SURFACE ( 'NONE', #31839, 32.50000000000000000 ) ;
#5463 = CARTESIAN_POINT ( 'NONE',  ( 19.06425588902558133, 21.73399333240935505, -19.11951029504797006 ) ) ;
#5464 = CARTESIAN_POINT ( 'NONE',  ( 20.08610463437158344, 37.20000000546237118, 27.64615127144129403 ) ) ;
#5465 = CARTESIAN_POINT ( 'NONE',  ( -26.29305231718578995, 12.19999999999998863, 19.10302069950538595 ) ) ;
#5466 = CARTESIAN_POINT ( 'NONE',  ( -10.37757302488624411, 26.72500000273120335, -31.93888565452638417 ) ) ;
#5467 = CARTESIAN_POINT ( 'NONE',  ( 13.97622843553589966, 40.21614583333332860, -24.20753774853756113 ) ) ;
#5468 = ORIENTED_EDGE ( 'NONE', *, *, #29543, .T. ) ;
#5469 = CARTESIAN_POINT ( 'NONE',  ( -10.37757302488623701, 63.52500000273118985, 31.93888565452638417 ) ) ;
#5470 = ADVANCED_FACE ( 'NONE', ( #33029 ), #30461, .T. ) ;
#5471 =( BOUNDED_CURVE ( )  B_SPLINE_CURVE ( 2, ( #16067, #26523, #3016, #13488, #23953, #422, #10909, #31826, #8319, #29920, #9801, #11729, #20277 ),
 .UNSPECIFIED., .F., .T. ) 
 B_SPLINE_CURVE_WITH_KNOTS ( ( 3, 2, 2, 2, 2, 2, 3 ),
 ( 0.9551282051282051766, 0.9564102564102564541, 0.9589743589743590091, 0.9615384615384615641, 0.9641025641025641191, 0.9666666666666666741, 0.9679487179487179516 ),
 .UNSPECIFIED. ) 
 CURVE ( )  GEOMETRIC_REPRESENTATION_ITEM ( )  RATIONAL_B_SPLINE_CURVE ( ( 0.9755282581475768211, 0.9755282581475768211, 1.000000000000000000, 0.9510565162951535312, 1.000000000000000000, 0.9510565162951535312, 1.000000000000000000, 0.9510565162951535312, 1.000000000000000000, 0.9510565162951535312, 1.000000000000000000, 0.9755282581475768211, 0.9755282581475768211 ) ) 
 REPRESENTATION_ITEM ( '' )  );
#5472 = EDGE_LOOP ( 'NONE', ( #1517, #25728 ) ) ;
#5473 = CARTESIAN_POINT ( 'NONE',  ( 7.505752307972854531, 12.57291666666666252, -28.01184896238303423 ) ) ;
#5474 = CARTESIAN_POINT ( 'NONE',  ( 25.98046417659858420, 11.57590250092397355, 15.04653450569292872 ) ) ;
#5475 = CARTESIAN_POINT ( 'NONE',  ( -33.58253175000000113, 5.125000002731180615, 0.000000000000000000 ) ) ;
#5476 = EDGE_CURVE ( 'NONE', #24093, #3731, #3853, .T. ) ;
#5477 = ORIENTED_EDGE ( 'NONE', *, *, #12464, .F. ) ;
#5478 = FACE_OUTER_BOUND ( 'NONE', #19566, .T. ) ;
#5479 = CARTESIAN_POINT ( 'NONE',  ( 27.16883889988623935, 36.57500000273117280, -19.73931689729374384 ) ) ;
#5480 = CARTESIAN_POINT ( 'NONE',  ( -20.08610463437157989, 40.20000000546235697, -27.64615127144129758 ) ) ;
#5481 = CARTESIAN_POINT ( 'NONE',  ( -20.08610463437157989, 77.70000000000003126, -27.64615127144129758 ) ) ;
#5482 = CARTESIAN_POINT ( 'NONE',  ( 32.50000000000000000, 53.09999999999998010, -10.55989012756945833 ) ) ;
#5483 = CARTESIAN_POINT ( 'NONE',  ( -12.13525491562421088, 81.79999999999998295, -8.816778784387096835 ) ) ;
#5484 = CARTESIAN_POINT ( 'NONE',  ( 33.58253175000000823, 42.27500000273118275, 10.91162601494192863 ) ) ;
#5485 =( LENGTH_UNIT ( ) NAMED_UNIT ( * ) SI_UNIT ( .MILLI., .METRE. ) );
#5486 = CARTESIAN_POINT ( 'NONE',  ( -26.29305231718578995, 24.19999999999998508, 19.10302069950538595 ) ) ;
#5487 = CARTESIAN_POINT ( 'NONE',  ( -2.092463501923844636E-15, 23.49999999999998934, -34.17252228774368916 ) ) ;
#5488 = CARTESIAN_POINT ( 'NONE',  ( 24.50000000000000355, 4.099999999999986322, -7.960532557706203605 ) ) ;
#5489 = CARTESIAN_POINT ( 'NONE',  ( -33.58253175000000113, 71.22500000273117848, 10.91162601494193929 ) ) ;
#5490 = CARTESIAN_POINT ( 'NONE',  ( -15.14183272437242600, 3.049999994537633263, 20.84094480462497856 ) ) ;
#5491 = CARTESIAN_POINT ( 'NONE',  ( -10.04305231718579172, 76.10000000546237686, -30.90933677959248982 ) ) ;
#5492 = CARTESIAN_POINT ( 'NONE',  ( -10.37757302488623701, 55.77500000273119696, 31.93888565452638417 ) ) ;
#5493 = CARTESIAN_POINT ( 'NONE',  ( 32.50000000000000000, 73.09999999999996589, -10.55989012756945833 ) ) ;
#5494 = CARTESIAN_POINT ( 'NONE',  ( -27.16883889988624290, 12.92500000273116889, -19.73931689729374028 ) ) ;
#5495 = CARTESIAN_POINT ( 'NONE',  ( -19.06425588902591173, 27.18788166759063785, -19.11951029504763611 ) ) ;
#5496 = CARTESIAN_POINT ( 'NONE',  ( 3.880418787951121828, 10.19874571299079413, -24.50000000000000355 ) ) ;
#5497 = CARTESIAN_POINT ( 'NONE',  ( -19.22940031075258105, 52.00000000000002132, 26.85591229561304161 ) ) ;
#5498 = CARTESIAN_POINT ( 'NONE',  ( -27.16883889988623935, 37.32500000273118701, 19.73931689729374739 ) ) ;
#5499 = CARTESIAN_POINT ( 'NONE',  ( -2.165007332552593587E-13, 45.00000000546237544, 32.50000000000000000 ) ) ;
#5500 = CARTESIAN_POINT ( 'NONE',  ( 31.04172217648528687, 52.00000000000000711, 12.81397374188273908 ) ) ;
#5501 = APPLICATION_CONTEXT ( 'automotive_design' ) ;
#5502 = CARTESIAN_POINT ( 'NONE',  ( 11.25946833292375793, 80.07500000273121543, -8.180482586598735395 ) ) ;
#5503 = CARTESIAN_POINT ( 'NONE',  ( 28.00173670424535644, 42.64545166574268364, -7.543491769121920321 ) ) ;
#5504 = CARTESIAN_POINT ( 'NONE',  ( 6.277390505771533514E-15, 55.00000000546239676, 34.17252228774368916 ) ) ;
#5505 = CARTESIAN_POINT ( 'NONE',  ( -4.300734207923759378, 76.97500000273122112, -13.23629886949340495 ) ) ;
#5506 = PRODUCT_DEFINITION_FORMATION_WITH_SPECIFIED_SOURCE ( 'ANY', '', #23326, .NOT_KNOWN. ) ;
#5507 = CARTESIAN_POINT ( 'NONE',  ( -26.07999730980490583, 15.15104166666666252, -6.988114217767815717 ) ) ;
#5508 = CARTESIAN_POINT ( 'NONE',  ( -2.092463501923844636E-15, 70.00000000546239676, -34.17252228774368916 ) ) ;
#5509 = CARTESIAN_POINT ( 'NONE',  ( 30.02300923189239512, 23.60156250000000000, -2.619432448724977703E-13 ) ) ;
#5510 = CARTESIAN_POINT ( 'NONE',  ( 10.37757302488624767, 29.97500000273119269, 31.93888565452638417 ) ) ;
#5511 = CARTESIAN_POINT ( 'NONE',  ( -18.94512977948576093, 16.32499999726880091, 13.76444248337722698 ) ) ;
#5512 = EDGE_LOOP ( 'NONE', ( #21967, #5316, #10409, #9993 ) ) ;
#5513 = CARTESIAN_POINT ( 'NONE',  ( 20.53372385742072481, 45.23475666759063785, -20.47846945139902175 ) ) ;
#5514 = CARTESIAN_POINT ( 'NONE',  ( 10.04305231718578817, 17.90000000546236691, -30.90933677959249337 ) ) ;
#5515 = CARTESIAN_POINT ( 'NONE',  ( 15.01150461594596308, 50.52864583333333570, -26.00068869287367335 ) ) ;
#5516 = CARTESIAN_POINT ( 'NONE',  ( -32.50000000000000000, 35.89999999999999858, -10.55989012756945300 ) ) ;
#5517 = EDGE_CURVE ( 'NONE', #11416, #30585, #12170, .T. ) ;
#5518 = CARTESIAN_POINT ( 'NONE',  ( -2.162160676586881955E-15, 56.87500000273117706, -35.31076352940723240 ) ) ;
#5519 = EDGE_CURVE ( 'NONE', #23148, #33131, #12379, .T. ) ;
#5520 = CARTESIAN_POINT ( 'NONE',  ( 26.29305231718578995, 53.70000000546237828, -19.10302069950538240 ) ) ;
#5521 = CARTESIAN_POINT ( 'NONE',  ( -4.300734207923755825, 79.77500000273118985, 13.23629886949340673 ) ) ;
#5522 = CARTESIAN_POINT ( 'NONE',  ( 10.37757302488624056, 44.52500000273118275, -31.93888565452638417 ) ) ;
#5523 = CARTESIAN_POINT ( 'NONE',  ( 15.00000000000000000, 73.25000000546239676, -1.836970198721029589E-15 ) ) ;
#5524 = CARTESIAN_POINT ( 'NONE',  ( -33.58253175000000113, 69.27500000273116143, -10.91162601494193218 ) ) ;
#5525 = CARTESIAN_POINT ( 'NONE',  ( 26.29305231718578995, 1.700000005462387609, -19.10302069950538240 ) ) ;
#5526 = CARTESIAN_POINT ( 'NONE',  ( -33.58253175000000113, 59.12500000273116996, 0.000000000000000000 ) ) ;
#5527 = CARTESIAN_POINT ( 'NONE',  ( -30.02300923189239867, 21.88281249999999289, 2.654126918244514854E-13 ) ) ;
#5528 = CARTESIAN_POINT ( 'NONE',  ( -26.29305231718579350, 41.80000000000000426, -19.10302069950537884 ) ) ;
#5529 = CARTESIAN_POINT ( 'NONE',  ( -7.236395654485757944, 7.224999997268804819, -22.27133577429736988 ) ) ;
#5530 = CARTESIAN_POINT ( 'NONE',  ( -20.75514604977248112, 11.67500000273118843, 28.56700777964554661 ) ) ;
#5531 = CARTESIAN_POINT ( 'NONE',  ( 0.000000000000000000, 0.000000000000000000, 0.000000000000000000 ) ) ;
#5532 = CARTESIAN_POINT ( 'NONE',  ( -27.95245687107223986, 37.63243083240935505, 0.04044903255043252877 ) ) ;
#5533 = CARTESIAN_POINT ( 'NONE',  ( 8.601468415847516980, 72.67500000273118133, -11.83890561707634781 ) ) ;
#5534 = CARTESIAN_POINT ( 'NONE',  ( 33.58253175000000113, 70.37500000273119838, -4.112674001490185761E-15 ) ) ;
#5535 = CARTESIAN_POINT ( 'NONE',  ( 0.000000000000000000, 0.000000000000000000, 0.000000000000000000 ) ) ;
#5536 = CARTESIAN_POINT ( 'NONE',  ( 20.75514604977248467, 74.67500000273118133, -28.56700777964554305 ) ) ;
#5537 = ORIENTED_EDGE ( 'NONE', *, *, #27607, .T. ) ;
#5538 = DIRECTION ( 'NONE',  ( 0.000000000000000000, 0.000000000000000000, -1.000000000000000000 ) ) ;
#5539 = CARTESIAN_POINT ( 'NONE',  ( 24.20753774853756113, 61.70052083333331439, 13.97622843553589789 ) ) ;
#5540 = CARTESIAN_POINT ( 'NONE',  ( -27.16883889988624290, 54.92500000273118843, -19.73931689729374028 ) ) ;
#5541 = CARTESIAN_POINT ( 'NONE',  ( -27.16883889988623935, 15.57500000273119589, 19.73931689729374739 ) ) ;
#5542 = CARTESIAN_POINT ( 'NONE',  ( -27.16883889988623935, 5.575000002731187010, 19.73931689729374739 ) ) ;
#5543 = CARTESIAN_POINT ( 'NONE',  ( 26.07999730980490227, 40.93229166666666430, 6.988114217767821046 ) ) ;
#5544 = CARTESIAN_POINT ( 'NONE',  ( 7.543491769121427382, 27.76079833425730925, -28.00173670424548433 ) ) ;
#5545 = CARTESIAN_POINT ( 'NONE',  ( 14.97647472619900455, 18.15326416574268720, -26.02091320914876960 ) ) ;
#5546 = CARTESIAN_POINT ( 'NONE',  ( -10.04305231718578462, 74.90000000546235981, 30.90933677959249337 ) ) ;
#5547 = CARTESIAN_POINT ( 'NONE',  ( 32.98389303421620866, 52.00000000000003553, 5.656568564006877686 ) ) ;
#5548 = CARTESIAN_POINT ( 'NONE',  ( -33.58253175000000113, 41.02500000273118985, -10.91162601494193041 ) ) ;
#5549 = CARTESIAN_POINT ( 'NONE',  ( -24.22776226481266448, 48.23138916574269786, -13.94119854578892514 ) ) ;
#5550 = CARTESIAN_POINT ( 'NONE',  ( -18.94512977948576093, 17.82499999726880446, 13.76444248337722698 ) ) ;
#5551 = CARTESIAN_POINT ( 'NONE',  ( 1.555960095263670572E-15, 6.499999999999994671, -24.50000000000000000 ) ) ;
#5552 = ORIENTED_EDGE ( 'NONE', *, *, #32298, .T. ) ;
#5553 = CARTESIAN_POINT ( 'NONE',  ( -33.58253175000000113, 47.47500000273119269, 10.91162601494193929 ) ) ;
#5554 = CARTESIAN_POINT ( 'NONE',  ( 0.000000000000000000, 0.000000000000000000, 0.000000000000000000 ) ) ;
#5555 = CIRCLE ( 'NONE', #8285, 16.50000000000002842 ) ;
#5556 = AXIS2_PLACEMENT_3D ( 'NONE', #9940, #2206, #12685 ) ;
#5557 = CARTESIAN_POINT ( 'NONE',  ( 13.94119854578937812, 49.67486083425730925, 24.22776226481240514 ) ) ;
#5558 = CARTESIAN_POINT ( 'NONE',  ( -20.75514604977248823, 69.07500000273115859, -28.56700777964554305 ) ) ;
#5559 = ORIENTED_EDGE ( 'NONE', *, *, #9068, .T. ) ;
#5560 = CARTESIAN_POINT ( 'NONE',  ( -27.16883889988623935, 15.32500000273116747, 19.73931689729374739 ) ) ;
#5561 = CARTESIAN_POINT ( 'NONE',  ( -15.01150461594595775, 21.30989583333331794, 26.00068869287368756 ) ) ;
#5562 = ORIENTED_EDGE ( 'NONE', *, *, #20203, .F. ) ;
#5563 = LINE ( 'NONE', #8794, #6171 ) ;
#5564 = CARTESIAN_POINT ( 'NONE',  ( 20.75514604977249178, 63.82500000273119412, 28.56700777964553950 ) ) ;
#5565 = CARTESIAN_POINT ( 'NONE',  ( -20.50609665440969209, 45.51562500000000000, 20.50609665441005092 ) ) ;
#5566 = DIRECTION ( 'NONE',  ( -0.000000000000000000, 1.000000000000000000, -0.000000000000000000 ) ) ;
#5567 = CARTESIAN_POINT ( 'NONE',  ( 23.41746824999999887, 9.224999997268820806, -7.608796670333727974 ) ) ;
#5568 = CARTESIAN_POINT ( 'NONE',  ( 10.37757302488624767, 5.725000002731183812, 31.93888565452638417 ) ) ;
#5569 = CARTESIAN_POINT ( 'NONE',  ( -33.58253175000000113, 29.47500000273117848, 10.91162601494193929 ) ) ;
#5570 = CARTESIAN_POINT ( 'NONE',  ( -5.147494310547478413, 64.44874571845313938, 32.49999999999998579 ) ) ;
#5571 = CARTESIAN_POINT ( 'NONE',  ( 28.00173670424535644, 63.27045166574269075, -7.543491769121920321 ) ) ;
#5572 = CARTESIAN_POINT ( 'NONE',  ( 10.37757302488624056, 78.77500000273118985, -31.93888565452638417 ) ) ;
#5573 = CARTESIAN_POINT ( 'NONE',  ( -11.25946833292375793, 80.67500000273119554, -8.180482586598733619 ) ) ;
#5574 = CARTESIAN_POINT ( 'NONE',  ( -32.50000000000000000, 4.099999999999986322, 10.55989012756946366 ) ) ;
#5575 = CARTESIAN_POINT ( 'NONE',  ( -32.50000000000000000, 16.00000000000000000, 0.000000000000000000 ) ) ;
#5576 = CARTESIAN_POINT ( 'NONE',  ( -2.428612866367529427E-13, 57.11718750000000711, -27.95245687107223276 ) ) ;
#5577 = CARTESIAN_POINT ( 'NONE',  ( -15.14183272437242600, 19.04999999453762172, 20.84094480462497856 ) ) ;
#5578 = CARTESIAN_POINT ( 'NONE',  ( -8.601468415847515203, 75.17500000273118133, 11.83890561707634959 ) ) ;
#5579 = CARTESIAN_POINT ( 'NONE',  ( 13.97622843553589966, 36.77864583333332860, -24.20753774853756113 ) ) ;
#5580 = CARTESIAN_POINT ( 'NONE',  ( 6.486482029760649416E-15, 21.62500000273119483, 35.31076352940723240 ) ) ;
#5581 = CARTESIAN_POINT ( 'NONE',  ( 27.16883889988624290, 73.92500000273120975, 19.73931689729373673 ) ) ;
#5582 = CIRCLE ( 'NONE', #9960, 26.50000000000000000 ) ;
#5583 = CARTESIAN_POINT ( 'NONE',  ( -27.16883889988624290, 39.17500000273120264, -19.73931689729374028 ) ) ;
#5584 = CARTESIAN_POINT ( 'NONE',  ( 20.75514604977248467, 12.67500000273118488, -28.56700777964554305 ) ) ;
#5585 = CARTESIAN_POINT ( 'NONE',  ( 0.04044903254993986036, 61.99256916759065206, -27.95245687107223986 ) ) ;
#5586 = CARTESIAN_POINT ( 'NONE',  ( -33.58253175000000113, 69.02500000273117564, -10.91162601494193041 ) ) ;
#5587 = CARTESIAN_POINT ( 'NONE',  ( 32.50000000000000711, 59.40000000546237402, 10.55989012756945122 ) ) ;
#5588 = CARTESIAN_POINT ( 'NONE',  ( -20.08610463437157989, 51.70000000000000284, -27.64615127144129758 ) ) ;
#5589 = CARTESIAN_POINT ( 'NONE',  ( 12.13525491562421088, 79.05000000546236549, 8.816778784387095058 ) ) ;
#5590 = CARTESIAN_POINT ( 'NONE',  ( 33.58253175000000823, 56.02500000273118275, 10.91162601494192685 ) ) ;
#5591 = CARTESIAN_POINT ( 'NONE',  ( 23.41746825000000243, 15.02499999726881086, 7.608796670333735079 ) ) ;
#5592 = VERTEX_POINT ( 'NONE', #26531 ) ;
#5593 = CARTESIAN_POINT ( 'NONE',  ( 27.16883889988624290, 68.17500000273118133, 19.73931689729373673 ) ) ;
#5594 = CARTESIAN_POINT ( 'NONE',  ( -10.04305231718579172, 15.60000000000000320, -30.90933677959248982 ) ) ;
#5595 = CARTESIAN_POINT ( 'NONE',  ( 14.47279130897151589, 18.82499999726881157, 19.92008829642072953 ) ) ;
#5596 = CARTESIAN_POINT ( 'NONE',  ( 24.18731323226247554, 15.01340250092397888, 14.01125832528285997 ) ) ;
#5597 = ORIENTED_EDGE ( 'NONE', *, *, #11873, .T. ) ;
#5598 = CARTESIAN_POINT ( 'NONE',  ( -2.162160676586881955E-15, 42.62500000273119838, -35.31076352940723240 ) ) ;
#5599 = FACE_OUTER_BOUND ( 'NONE', #812, .T. ) ;
#5600 = EDGE_CURVE ( 'NONE', #7743, #23590, #21725, .T. ) ;
#5601 = EDGE_LOOP ( 'NONE', ( #33660, #17420, #7311, #18188 ) ) ;
#5602 = CARTESIAN_POINT ( 'NONE',  ( -7.505752307972844761, 38.35416666666666430, 28.01184896238304134 ) ) ;
#5603 = CARTESIAN_POINT ( 'NONE',  ( 10.04305231718579705, 4.599999999999992539, 30.90933677959248982 ) ) ;
#5604 = CARTESIAN_POINT ( 'NONE',  ( 20.08610463437158344, 3.200000005462373398, 27.64615127144129403 ) ) ;
#5605 = CARTESIAN_POINT ( 'NONE',  ( -19.79898987322349768, 67.00000000000000000, -19.79898987322315307 ) ) ;
#5606 = CARTESIAN_POINT ( 'NONE',  ( 26.00068869287367335, 17.01302083333332504, 15.01150461594596308 ) ) ;
#5607 = CARTESIAN_POINT ( 'NONE',  ( -19.82091636218621034, 2.799999999999997158, -14.40073868116559552 ) ) ;
#5608 = CARTESIAN_POINT ( 'NONE',  ( -27.16883889988623935, 9.575000002731204773, 19.73931689729374739 ) ) ;
#5609 = CARTESIAN_POINT ( 'NONE',  ( -2.092463501923844636E-15, 57.49999999999999289, -34.17252228774368916 ) ) ;
#5610 = CARTESIAN_POINT ( 'NONE',  ( 5.147494310547434893, 57.05125428700922896, 32.49999999999999289 ) ) ;
#5611 = CARTESIAN_POINT ( 'NONE',  ( -4.000000000000003553, 0.000000000000000000, 0.000000000000000000 ) ) ;
#5612 = CARTESIAN_POINT ( 'NONE',  ( 15.04653450569339945, 33.04909749907601935, 25.98046417659831775 ) ) ;
#5613 = CARTESIAN_POINT ( 'NONE',  ( -8.601468415847515203, 77.67500000273119554, 11.83890561707634959 ) ) ;
#5614 = CARTESIAN_POINT ( 'NONE',  ( 26.00068869287367690, 47.95052083333332149, 15.01150461594596486 ) ) ;
#5615 = APPLICATION_PROTOCOL_DEFINITION ( 'draft international standard', 'automotive_design', 1998, #27843 ) ;
#5616 = CARTESIAN_POINT ( 'NONE',  ( 1.836970198721029589E-15, 82.00000000000001421, 15.00000000000000000 ) ) ;
#5617 = DIRECTION ( 'NONE',  ( -0.000000000000000000, 1.000000000000000000, -0.000000000000000000 ) ) ;
#5618 = CARTESIAN_POINT ( 'NONE',  ( -10.04305231718578462, 2.400000000000013234, 30.90933677959249337 ) ) ;
#5619 = DIRECTION ( 'NONE',  ( 0.000000000000000000, 1.000000000000000000, 0.000000000000000000 ) ) ;
#5620 = CARTESIAN_POINT ( 'NONE',  ( 19.06425588902558133, 66.42149333240935505, -19.11951029504797006 ) ) ;
#5621 = CARTESIAN_POINT ( 'NONE',  ( -27.16883889988624290, 42.92500000273119554, -19.73931689729374028 ) ) ;
#5622 = CARTESIAN_POINT ( 'NONE',  ( 4.635254915624212657, 72.85000000546237686, 14.26584774442730286 ) ) ;
#5623 = CARTESIAN_POINT ( 'NONE',  ( 20.75514604977249178, 58.07500000273117990, 28.56700777964553950 ) ) ;
#5624 = CARTESIAN_POINT ( 'NONE',  ( -33.58253175000000113, 37.47500000273118559, 10.91162601494193929 ) ) ;
#5625 = CARTESIAN_POINT ( 'NONE',  ( 26.29305231718579350, 23.30000000546236905, 19.10302069950537529 ) ) ;
#5626 = CARTESIAN_POINT ( 'NONE',  ( -13.97622843553632777, 25.89322916666666430, -24.20753774853731599 ) ) ;
#5627 = DIRECTION ( 'NONE',  ( 0.000000000000000000, -1.000000000000000000, 0.000000000000000000 ) ) ;
#5628 = CARTESIAN_POINT ( 'NONE',  ( -26.29305231718579350, 44.30000000546238681, -19.10302069950537884 ) ) ;
#5629 = CARTESIAN_POINT ( 'NONE',  ( 32.50000000000000000, 73.09999999999996589, -10.55989012756945833 ) ) ;
#5630 = CARTESIAN_POINT ( 'NONE',  ( 27.16883889988624290, 11.92500000273118133, 19.73931689729373673 ) ) ;
#5631 = CARTESIAN_POINT ( 'NONE',  ( -23.41746825000000243, 1.724999997268824581, 7.608796670333725309 ) ) ;
#5632 = DIRECTION ( 'NONE',  ( 0.000000000000000000, 1.000000000000000000, 0.000000000000000000 ) ) ;
#5633 = CARTESIAN_POINT ( 'NONE',  ( 24.22776226481265383, 32.76263916574268364, 13.94119854578893580 ) ) ;
#5634 = LINE ( 'NONE', #12851, #22193 ) ;
#5635 = CARTESIAN_POINT ( 'NONE',  ( -20.75514604977248823, 18.82500000273119056, -28.56700777964554305 ) ) ;
#5636 = CARTESIAN_POINT ( 'NONE',  ( -27.95245687107222921, 42.50781249999997868, 2.498001805406602216E-13 ) ) ;
#5637 = ORIENTED_EDGE ( 'NONE', *, *, #9027, .F. ) ;
#5638 = CARTESIAN_POINT ( 'NONE',  ( 33.58253175000000823, 60.02500000273116854, 10.91162601494192863 ) ) ;
#5639 = ORIENTED_EDGE ( 'NONE', *, *, #10703, .T. ) ;
#5640 = CARTESIAN_POINT ( 'NONE',  ( -15.01150461594642138, 15.58072916666666607, -26.00068869287340334 ) ) ;
#5641 = CARTESIAN_POINT ( 'NONE',  ( 15.04653450569292872, 14.15402750092397532, -25.98046417659857710 ) ) ;
#5642 = AXIS2_PLACEMENT_3D ( 'NONE', #7175, #27950, #9583 ) ;
#5643 = CARTESIAN_POINT ( 'NONE',  ( 20.75514604977249178, 3.825000002731188786, 28.56700777964553950 ) ) ;
#5644 = AXIS2_PLACEMENT_3D ( 'NONE', #13633, #565, #13957 ) ;
#5645 = ORIENTED_EDGE ( 'NONE', *, *, #12029, .F. ) ;
#5646 = CARTESIAN_POINT ( 'NONE',  ( -18.94512977948575738, 1.424999997268805441, -13.76444248337723231 ) ) ;
#5647 = CARTESIAN_POINT ( 'NONE',  ( -20.75514604977248112, 29.67500000273119909, 28.56700777964554661 ) ) ;
#5648 = CARTESIAN_POINT ( 'NONE',  ( 6.277390505771533514E-15, 39.00000000546236834, 34.17252228774368916 ) ) ;
#5649 = CARTESIAN_POINT ( 'NONE',  ( -32.50000000000000000, 76.00000000000001421, 0.000000000000000000 ) ) ;
#5650 = CARTESIAN_POINT ( 'NONE',  ( -32.50000000000000000, 54.50000000546237544, 0.000000000000000000 ) ) ;
#5651 = CARTESIAN_POINT ( 'NONE',  ( -32.50000000000000000, 52.50000000546238255, 0.000000000000000000 ) ) ;
#5652 = CARTESIAN_POINT ( 'NONE',  ( -33.58253175000000113, 45.37500000273120548, 0.000000000000000000 ) ) ;
#5653 = SURFACE_STYLE_FILL_AREA ( #29319 ) ;
#5654 = CARTESIAN_POINT ( 'NONE',  ( 26.29305231718579350, 24.80000000000000426, 19.10302069950537529 ) ) ;
#5655 = CARTESIAN_POINT ( 'NONE',  ( 10.04305231718579705, 22.60000000000000853, 30.90933677959248982 ) ) ;
#5656 = CARTESIAN_POINT ( 'NONE',  ( 15.14183272437242245, 6.300000000000004263, -20.84094480462497856 ) ) ;
#5657 = CARTESIAN_POINT ( 'NONE',  ( 20.75514604977249178, 63.82500000273119412, 28.56700777964553950 ) ) ;
#5658 = CARTESIAN_POINT ( 'NONE',  ( -33.25271216035369548, 66.99999999999997158, -3.649504031948202165 ) ) ;
#5659 = CARTESIAN_POINT ( 'NONE',  ( -20.08610463437156923, 76.80000000546239391, 27.64615127144130113 ) ) ;
#5660 = CARTESIAN_POINT ( 'NONE',  ( 27.16883889988623935, 52.57500000273118701, -19.73931689729374384 ) ) ;
#5661 = CARTESIAN_POINT ( 'NONE',  ( -23.41746824999999887, 3.624999997268813168, -2.867812753649727150E-15 ) ) ;
#5662 = CARTESIAN_POINT ( 'NONE',  ( 3.880418787951132042, 4.448745718453150033, -24.50000000000000355 ) ) ;
#5663 = CARTESIAN_POINT ( 'NONE',  ( 33.58253175000000823, 12.02500000273117742, 10.91162601494192863 ) ) ;
#5664 = CARTESIAN_POINT ( 'NONE',  ( -13.94119854578936923, 30.76861083425731280, -24.22776226481241224 ) ) ;
#5665 = EDGE_CURVE ( 'NONE', #13370, #11893, #26017, .T. ) ;
#5666 = CARTESIAN_POINT ( 'NONE',  ( 20.82183453687062169, 66.99999999999997158, -25.59657189324412485 ) ) ;
#5667 = CARTESIAN_POINT ( 'NONE',  ( -27.48632242023157701, 51.99999999999999289, 17.98641839608171011 ) ) ;
#5668 = CARTESIAN_POINT ( 'NONE',  ( 10.37757302488624767, 31.72500000273119269, 31.93888565452638417 ) ) ;
#5669 = CARTESIAN_POINT ( 'NONE',  ( -26.29305231718578995, 56.70000000546236407, 19.10302069950538595 ) ) ;
#5670 = CARTESIAN_POINT ( 'NONE',  ( 0.000000000000000000, 0.000000000000000000, 0.000000000000000000 ) ) ;
#5671 = ADVANCED_FACE ( 'NONE', ( #594 ), #13664, .T. ) ;
#5672 = AXIS2_PLACEMENT_3D ( 'NONE', #23110, #23461, #33923 ) ;
#5673 = CARTESIAN_POINT ( 'NONE',  ( 4.300734207923757602, 76.27500000273118985, -13.23629886949340673 ) ) ;
#5674 = CARTESIAN_POINT ( 'NONE',  ( -0.04044903255044120238, 45.36680583240934794, -30.02300923189239867 ) ) ;
#5675 = CARTESIAN_POINT ( 'NONE',  ( 20.08610463437157279, 55.80000000546236549, -27.64615127144129758 ) ) ;
#5676 = CARTESIAN_POINT ( 'NONE',  ( 4.300734207923757602, 72.77500000273118985, -13.23629886949340673 ) ) ;
#5677 =( BOUNDED_CURVE ( )  B_SPLINE_CURVE ( 2, ( #127, #28969, #28460, #8202, #5465, #21267, #15947, #20588, #26402, #2895, #18692, #33790, #29132 ),
 .UNSPECIFIED., .F., .T. ) 
 B_SPLINE_CURVE_WITH_KNOTS ( ( 3, 2, 2, 2, 2, 2, 3 ),
 ( 0.8653846153846154188, 0.8666666666666666963, 0.8692307692307692513, 0.8717948717948718063, 0.8743589743589743613, 0.8769230769230769162, 0.8782051282051281937 ),
 .UNSPECIFIED. ) 
 CURVE ( )  GEOMETRIC_REPRESENTATION_ITEM ( )  RATIONAL_B_SPLINE_CURVE ( ( 0.9755282581475768211, 0.9755282581475768211, 1.000000000000000000, 0.9510565162951535312, 1.000000000000000000, 0.9510565162951535312, 1.000000000000000000, 0.9510565162951535312, 1.000000000000000000, 0.9510565162951535312, 1.000000000000000000, 0.9755282581475768211, 0.9755282581475768211 ) ) 
 REPRESENTATION_ITEM ( '' )  );
#5678 = SURFACE_STYLE_FILL_AREA ( #15651 ) ;
#5679 = CARTESIAN_POINT ( 'NONE',  ( 2.584737979205441561E-13, 17.58593749999999645, 27.95245687107222921 ) ) ;
#5680 = CARTESIAN_POINT ( 'NONE',  ( 26.29305231718578995, 71.70000000546239960, -19.10302069950538240 ) ) ;
#5681 = CARTESIAN_POINT ( 'NONE',  ( 26.00068869287367335, 23.88802083333331794, 15.01150461594596308 ) ) ;
#5682 = CARTESIAN_POINT ( 'NONE',  ( -33.58253175000000113, 25.47500000273118914, 10.91162601494193929 ) ) ;
#5683 = CARTESIAN_POINT ( 'NONE',  ( -14.47279130897152299, 14.42499999726880056, 19.92008829642072243 ) ) ;
#5684 = VERTEX_POINT ( 'NONE', #432 ) ;
#5685 = CARTESIAN_POINT ( 'NONE',  ( -7.468012846824771955, 41.22434000092397355, -28.02196122052045624 ) ) ;
#5686 = CARTESIAN_POINT ( 'NONE',  ( -26.29305231718578995, 18.70000000546238894, 19.10302069950538595 ) ) ;
#5687 = CARTESIAN_POINT ( 'NONE',  ( 7.505752307972854531, 50.38541666666666430, -28.01184896238303423 ) ) ;
#5688 = CARTESIAN_POINT ( 'NONE',  ( 20.08610463437157279, 75.30000000000001137, -27.64615127144129758 ) ) ;
#5689 = CARTESIAN_POINT ( 'NONE',  ( -20.75514604977248823, 49.07500000273117280, -28.56700777964554305 ) ) ;
#5690 = CARTESIAN_POINT ( 'NONE',  ( 32.50000000000000000, 55.50000000546237544, -3.980102097228898626E-15 ) ) ;
#5691 = CARTESIAN_POINT ( 'NONE',  ( 4.300734207923757602, 80.77500000273118985, -13.23629886949340673 ) ) ;
#5692 = CARTESIAN_POINT ( 'NONE',  ( 20.75514604977248467, 36.42500000273118843, -28.56700777964554305 ) ) ;
#5693 = CARTESIAN_POINT ( 'NONE',  ( -2.375766604868048137, 76.69874572391550771, 14.99999999999999822 ) ) ;
#5694 = CARTESIAN_POINT ( 'NONE',  ( -27.16883889988624290, 59.17500000273118133, -19.73931689729374028 ) ) ;
#5695 = CARTESIAN_POINT ( 'NONE',  ( 10.04305231718579705, 1.100000005462370423, 30.90933677959248982 ) ) ;
#5696 = AXIS2_PLACEMENT_3D ( 'NONE', #28118, #27437, #33431 ) ;
#5697 = CARTESIAN_POINT ( 'NONE',  ( 33.58253175000000113, 54.12500000273119838, -4.112674001490185761E-15 ) ) ;
#5698 = CARTESIAN_POINT ( 'NONE',  ( 28.01184896238304134, 23.74479166666666430, 7.505752307972846538 ) ) ;
#5699 = CARTESIAN_POINT ( 'NONE',  ( -10.04305231718579172, 39.59999999999999432, -30.90933677959248982 ) ) ;
#5700 = CARTESIAN_POINT ( 'NONE',  ( -14.47279130897152122, 7.924999997268803220, 19.92008829642072243 ) ) ;
#5701 = CARTESIAN_POINT ( 'NONE',  ( 33.58253175000000113, 8.375000002731169957, -4.112674001490185761E-15 ) ) ;
#5702 = CARTESIAN_POINT ( 'NONE',  ( -5.147494310547377161, 66.05125428700924317, -32.50000000000002132 ) ) ;
#5703 = CARTESIAN_POINT ( 'NONE',  ( 0.000000000000000000, 52.00000000000000711, 32.50000000000000000 ) ) ;
#5704 = CARTESIAN_POINT ( 'NONE',  ( 6.486482029760648627E-15, 75.87500000273119838, 35.31076352940722529 ) ) ;
#5705 = CARTESIAN_POINT ( 'NONE',  ( 0.000000000000000000, 82.00000000000001421, 0.000000000000000000 ) ) ;
#5706 = APPLICATION_CONTEXT ( 'automotive_design' ) ;
#5707 = CARTESIAN_POINT ( 'NONE',  ( 33.58253175000000113, 68.47500000273119269, -10.91162601494193751 ) ) ;
#5708 = ORIENTED_EDGE ( 'NONE', *, *, #30107, .T. ) ;
#5709 = DIRECTION ( 'NONE',  ( -0.000000000000000000, -1.000000000000000000, -0.000000000000000000 ) ) ;
#5710 = CARTESIAN_POINT ( 'NONE',  ( -6.988114217768288228, 63.84895833333332860, -26.07999730980477437 ) ) ;
#5711 = EDGE_CURVE ( 'NONE', #31633, #32671, #22703, .T. ) ;
#5712 = CARTESIAN_POINT ( 'NONE',  ( 27.16883889988624290, 51.92500000273118843, 19.73931689729373673 ) ) ;
#5713 = CARTESIAN_POINT ( 'NONE',  ( -10.37757302488623701, 13.77500000273117209, 31.93888565452638417 ) ) ;
#5714 = CARTESIAN_POINT ( 'NONE',  ( -20.75514604977248112, 5.675000002731189319, 28.56700777964554661 ) ) ;
#5715 = CARTESIAN_POINT ( 'NONE',  ( 24.20753774853731244, 37.06510416666667140, -13.97622843553633132 ) ) ;
#5716 = CARTESIAN_POINT ( 'NONE',  ( 20.47846945139902530, 25.46913166759064140, 20.53372385742071771 ) ) ;
#5717 = CARTESIAN_POINT ( 'NONE',  ( -30.02300923189239867, 20.44493083240935150, 0.04044903255044988294 ) ) ;
#5718 = CARTESIAN_POINT ( 'NONE',  ( -2.092463501923844636E-15, 76.00000000546235412, -34.17252228774368916 ) ) ;
#5719 = CARTESIAN_POINT ( 'NONE',  ( 6.725304478054956903, 51.99999999999999289, -31.94333337441925025 ) ) ;
#5720 = CARTESIAN_POINT ( 'NONE',  ( 10.37757302488624767, 39.72500000273118559, 31.93888565452638417 ) ) ;
#5721 = CARTESIAN_POINT ( 'NONE',  ( 7.025853678916867295, 46.94232666574269075, 26.06988505166722803 ) ) ;
#5722 = CARTESIAN_POINT ( 'NONE',  ( -23.41746825000000598, 13.72499999726882258, 7.608796670333726198 ) ) ;
#5723 = CARTESIAN_POINT ( 'NONE',  ( 0.000000000000000000, 16.99999999999998579, 0.000000000000000000 ) ) ;
#5724 = ORIENTED_EDGE ( 'NONE', *, *, #19597, .T. ) ;
#5725 = CARTESIAN_POINT ( 'NONE',  ( 10.37757302488624767, 49.97500000273117848, 31.93888565452638417 ) ) ;
#5726 = CARTESIAN_POINT ( 'NONE',  ( 2.375766604868046361, 76.55125428154686062, 14.99999999999999822 ) ) ;
#5727 = CARTESIAN_POINT ( 'NONE',  ( 24.18731323226247554, 52.82590250092398065, 14.01125832528285997 ) ) ;
#5728 = CARTESIAN_POINT ( 'NONE',  ( 33.58253175000000113, 70.47500000273117848, -10.91162601494193751 ) ) ;
#5729 = ORIENTED_EDGE ( 'NONE', *, *, #26149, .T. ) ;
#5730 = CARTESIAN_POINT ( 'NONE',  ( -2.162160676586881955E-15, 16.62500000273120548, -35.31076352940723240 ) ) ;
#5731 = CARTESIAN_POINT ( 'NONE',  ( -20.50609665440969209, 28.32812499999999645, 20.50609665441005092 ) ) ;
#5732 = ORIENTED_EDGE ( 'NONE', *, *, #32911, .T. ) ;
#5733 = CARTESIAN_POINT ( 'NONE',  ( -10.04305231718579172, 48.10000000546238397, -30.90933677959248982 ) ) ;
#5734 = CARTESIAN_POINT ( 'NONE',  ( 20.75514604977249178, 55.82500000273119412, 28.56700777964553950 ) ) ;
#5735 = CARTESIAN_POINT ( 'NONE',  ( -20.50609665441004736, 49.81249999999999289, -20.50609665440969565 ) ) ;
#5736 = CARTESIAN_POINT ( 'NONE',  ( -20.08610463437157989, 16.20000000546237118, -27.64615127144129758 ) ) ;
#5737 = DIRECTION ( 'NONE',  ( 0.000000000000000000, 1.000000000000000000, 0.000000000000000000 ) ) ;
#5738 = CARTESIAN_POINT ( 'NONE',  ( -4.523095164977117273E-15, 6.624999997268815832, 24.62258325217400312 ) ) ;
#5739 = AXIS2_PLACEMENT_3D ( 'NONE', #33415, #17300, #20389 ) ;
#5740 = CARTESIAN_POINT ( 'NONE',  ( -20.75514604977248112, 27.67500000273118133, 28.56700777964554661 ) ) ;
#5741 = CARTESIAN_POINT ( 'NONE',  ( -20.53372385742107653, 65.56211833240934084, -20.47846945139867003 ) ) ;
#5742 = CARTESIAN_POINT ( 'NONE',  ( 8.601468415847516980, 80.17500000273116711, -11.83890561707634781 ) ) ;
#5743 = CARTESIAN_POINT ( 'NONE',  ( -5.147494310547430452, 3.551254281546844194, -32.49999999999999289 ) ) ;
#5744 = CARTESIAN_POINT ( 'NONE',  ( 20.08610463437157279, 7.300000000000001599, -27.64615127144129758 ) ) ;
#5745 = CARTESIAN_POINT ( 'NONE',  ( -13.97622843553632777, 60.26822916666665719, -24.20753774853731599 ) ) ;
#5746 = CARTESIAN_POINT ( 'NONE',  ( -15.14183272437241889, 16.44999999453761319, -20.84094480462497856 ) ) ;
#5747 = CARTESIAN_POINT ( 'NONE',  ( 4.300734207923757602, 72.27500000273117564, -13.23629886949340673 ) ) ;
#5748 = CARTESIAN_POINT ( 'NONE',  ( -13.97622843553632421, 32.76822916666666430, -24.20753774853731599 ) ) ;
#5749 = CARTESIAN_POINT ( 'NONE',  ( 20.75514604977248467, 26.42500000273118843, -28.56700777964554305 ) ) ;
#5750 = CARTESIAN_POINT ( 'NONE',  ( 10.37757302488624767, 71.72500000273117848, 31.93888565452638417 ) ) ;
#5751 = CARTESIAN_POINT ( 'NONE',  ( -10.37757302488623701, 37.77500000273118985, 31.93888565452638417 ) ) ;
#5752 = CARTESIAN_POINT ( 'NONE',  ( -20.75514604977248823, 13.07500000273120300, -28.56700777964554305 ) ) ;
#5753 = CARTESIAN_POINT ( 'NONE',  ( 6.950374756619721595, 53.25559000092396644, 26.09010956794232428 ) ) ;
#5754 = CARTESIAN_POINT ( 'NONE',  ( -33.58253175000000113, 69.12500000273119838, 0.000000000000000000 ) ) ;
#5755 = DIRECTION ( 'NONE',  ( 0.000000000000000000, -1.000000000000000000, 0.000000000000000000 ) ) ;
#5756 = CARTESIAN_POINT ( 'NONE',  ( 20.08610463437158344, 54.69999999999998863, 27.64615127144129403 ) ) ;
#5757 = CARTESIAN_POINT ( 'NONE',  ( -12.13525491562421088, 72.05000000546237970, -8.816778784387096835 ) ) ;
#5758 = CARTESIAN_POINT ( 'NONE',  ( -2.162160676586882350E-15, 56.62500000273116996, -35.31076352940722529 ) ) ;
#5759 = CARTESIAN_POINT ( 'NONE',  ( 18.94512977948575738, 12.92499999726881654, 13.76444248337723408 ) ) ;
#5760 = VECTOR ( 'NONE', #14913, 1000.000000000000000 ) ;
#5761 = ORIENTED_EDGE ( 'NONE', *, *, #25175, .T. ) ;
#5762 = CARTESIAN_POINT ( 'NONE',  ( 27.16883889988623935, 64.57500000273118701, -19.73931689729374384 ) ) ;
#5763 = CARTESIAN_POINT ( 'NONE',  ( -10.37757302488623701, 3.525000002731204507, 31.93888565452638417 ) ) ;
#5764 = CARTESIAN_POINT ( 'NONE',  ( 1.507698388325705758E-15, 7.124999997268799845, -24.62258325217400312 ) ) ;
#5765 = CARTESIAN_POINT ( 'NONE',  ( 24.18731323226247554, 25.32590250092397710, 14.01125832528285997 ) ) ;
#5766 = VERTEX_POINT ( 'NONE', #29754 ) ;
#5767 = CARTESIAN_POINT ( 'NONE',  ( -33.58253175000000113, 35.02500000273118275, -10.91162601494193218 ) ) ;
#5768 = CARTESIAN_POINT ( 'NONE',  ( -1.778240108872766143E-15, 42.00000000546236834, -32.49999999999999289 ) ) ;
#5769 = ORIENTED_EDGE ( 'NONE', *, *, #33051, .T. ) ;
#5770 = CARTESIAN_POINT ( 'NONE',  ( -20.50609665441004736, 53.25000000000000000, -20.50609665440969565 ) ) ;
#5771 = CARTESIAN_POINT ( 'NONE',  ( 20.08610463437158344, 4.699999999999996625, 27.64615127144129403 ) ) ;
#5772 = CARTESIAN_POINT ( 'NONE',  ( -24.50000000000000000, 3.000000000000002665, -3.000384657911015469E-15 ) ) ;
#5773 = CARTESIAN_POINT ( 'NONE',  ( -20.75514604977248112, 75.42500000273120975, 28.56700777964554661 ) ) ;
#5774 = CARTESIAN_POINT ( 'NONE',  ( 26.00068869287340334, 19.87760416666666430, -15.01150461594642316 ) ) ;
#5775 = CARTESIAN_POINT ( 'NONE',  ( 14.47279130897151589, 18.32499999726882578, 19.92008829642072953 ) ) ;
#5776 = CARTESIAN_POINT ( 'NONE',  ( 27.16883889988623935, 6.575000002731201221, -19.73931689729374384 ) ) ;
#5777 = CARTESIAN_POINT ( 'NONE',  ( 27.16883889988624290, 21.92500000273117777, 19.73931689729373673 ) ) ;
#5778 = CARTESIAN_POINT ( 'NONE',  ( 13.91746825000000065, 77.77500000273118985, 4.522059556121115875 ) ) ;
#5779 = CARTESIAN_POINT ( 'NONE',  ( 9.270509831248421762, 77.55000000546235128, -12.75976212528059861 ) ) ;
#5780 = CARTESIAN_POINT ( 'NONE',  ( -25.98046417659831420, 37.34597249907603356, 15.04653450569339945 ) ) ;
#5781 = CARTESIAN_POINT ( 'NONE',  ( 13.91746824999999532, 74.47500000273116427, -4.522059556121118540 ) ) ;
#5782 = CARTESIAN_POINT ( 'NONE',  ( 15.01150461594596486, 50.52864583333332149, -26.00068869287367690 ) ) ;
#5783 = CARTESIAN_POINT ( 'NONE',  ( -3.880418787951174675, 10.55125428154683931, -24.49999999999998579 ) ) ;
#5784 = CARTESIAN_POINT ( 'NONE',  ( 5.779280353836490358E-15, 55.00000000546238965, 32.49999999999999289 ) ) ;
#5785 = CARTESIAN_POINT ( 'NONE',  ( 13.94119854578893580, 62.84076416574269786, -24.22776226481265383 ) ) ;
#5786 = CARTESIAN_POINT ( 'NONE',  ( 33.58253175000000823, 44.02500000273118275, 10.91162601494192863 ) ) ;
#5787 = CARTESIAN_POINT ( 'NONE',  ( -9.270509831248425314, 73.95000000546235697, -12.75976212528059861 ) ) ;
#5788 = CARTESIAN_POINT ( 'NONE',  ( 33.58253175000000113, 54.37500000273119838, -4.112674001490185761E-15 ) ) ;
#5789 = CARTESIAN_POINT ( 'NONE',  ( -20.75514604977248112, 33.67500000273119554, 28.56700777964554661 ) ) ;
#5790 = CARTESIAN_POINT ( 'NONE',  ( 0.000000000000000000, 16.99999999999998579, 0.000000000000000000 ) ) ;
#5791 = CARTESIAN_POINT ( 'NONE',  ( -13.97622843553588901, 21.30989583333332504, 24.20753774853756823 ) ) ;
#5792 = DIRECTION ( 'NONE',  ( -0.000000000000000000, -1.000000000000000000, -0.000000000000000000 ) ) ;
#5793 = CARTESIAN_POINT ( 'NONE',  ( 20.08610463437158344, 30.69999999999999218, 27.64615127144129403 ) ) ;
#5794 = CARTESIAN_POINT ( 'NONE',  ( 32.50000000000000000, 71.00000000000000000, -3.980102097228898626E-15 ) ) ;
#5795 = CARTESIAN_POINT ( 'NONE',  ( 27.16883889988624290, 5.925000002731190207, 19.73931689729373673 ) ) ;
#5796 = CARTESIAN_POINT ( 'NONE',  ( -23.41746824999999887, 3.624999997268813168, -2.867812753649727150E-15 ) ) ;
#5797 = AXIS2_PLACEMENT_3D ( 'NONE', #26353, #33739, #21048 ) ;
#5798 = EDGE_CURVE ( 'NONE', #21432, #28216, #28339, .T. ) ;
#5799 = DIRECTION ( 'NONE',  ( 0.000000000000000000, 1.000000000000000000, 0.000000000000000000 ) ) ;
#5800 = CARTESIAN_POINT ( 'NONE',  ( -26.06988505166722803, 23.73920166574268364, 7.025853678916877953 ) ) ;
#5801 = CARTESIAN_POINT ( 'NONE',  ( -5.147494310547423346, 60.44874571845313938, 32.50000000000000000 ) ) ;
#5802 = CARTESIAN_POINT ( 'NONE',  ( -2.162160676586882350E-15, 22.62500000273119127, -35.31076352940722529 ) ) ;
#5803 = CARTESIAN_POINT ( 'NONE',  ( -26.07999730980490583, 49.52604166666666430, -6.988114217767815717 ) ) ;
#5804 = EDGE_CURVE ( 'NONE', #8435, #13370, #10887, .T. ) ;
#5805 = VERTEX_POINT ( 'NONE', #17240 ) ;
#5806 = CARTESIAN_POINT ( 'NONE',  ( 10.37757302488624767, 57.72500000273118559, 31.93888565452638417 ) ) ;
#5807 = EDGE_CURVE ( 'NONE', #27368, #25816, #24780, .T. ) ;
#5808 = ORIENTED_EDGE ( 'NONE', *, *, #29497, .F. ) ;
#5809 = CARTESIAN_POINT ( 'NONE',  ( -30.02300923189239512, 18.44531249999999645, 2.654126918244515359E-13 ) ) ;
#5810 = CARTESIAN_POINT ( 'NONE',  ( 28.02196122052045268, 11.14621500092397532, -7.468012846824774620 ) ) ;
#5811 = CARTESIAN_POINT ( 'NONE',  ( -27.16883889988623935, 5.325000002731187010, 19.73931689729374739 ) ) ;
#5812 = EDGE_CURVE ( 'NONE', #10957, #6411, #32116, .T. ) ;
#5813 = ORIENTED_EDGE ( 'NONE', *, *, #3983, .T. ) ;
#5814 = CYLINDRICAL_SURFACE ( 'NONE', #16323, 24.50000000000000000 ) ;
#5815 = CARTESIAN_POINT ( 'NONE',  ( 20.75514604977248467, 30.67500000273119909, -28.56700777964554305 ) ) ;
#5816 = CARTESIAN_POINT ( 'NONE',  ( 6.277390505771533514E-15, 33.00000000546238255, 34.17252228774368916 ) ) ;
#5817 = CIRCLE ( 'NONE', #7458, 10.17814985357208890 ) ;
#5818 = CARTESIAN_POINT ( 'NONE',  ( -32.50000000000000000, 78.10000000000000853, 10.55989012756946366 ) ) ;
#5819 = CARTESIAN_POINT ( 'NONE',  ( -23.09401076758502924, 86.00000000000001421, 5.354274672883389237E-15 ) ) ;
#5820 = CARTESIAN_POINT ( 'NONE',  ( -3.880418787951099180, 10.55125428154683753, -24.50000000000001421 ) ) ;
#5821 = CARTESIAN_POINT ( 'NONE',  ( -27.16883889988623935, 45.57500000273117990, 19.73931689729374739 ) ) ;
#5822 = CARTESIAN_POINT ( 'NONE',  ( 20.08610463437158344, 22.70000000000000995, 27.64615127144129403 ) ) ;
#5823 = CARTESIAN_POINT ( 'NONE',  ( 20.08610463437157279, 19.30000000000000426, -27.64615127144129758 ) ) ;
#5824 = CARTESIAN_POINT ( 'NONE',  ( -24.50000000000000355, 8.900000000000011013, -7.960532557706207157 ) ) ;
#5825 = CARTESIAN_POINT ( 'NONE',  ( 33.58253175000000113, 60.22500000273119980, -10.91162601494193751 ) ) ;
#5826 = CARTESIAN_POINT ( 'NONE',  ( -19.82091636218621034, 6.549999994537619941, -14.40073868116559552 ) ) ;
#5827 = CARTESIAN_POINT ( 'NONE',  ( 9.299350884854096222, 74.00000000000000000, -10.69806180658744310 ) ) ;
#5828 = CARTESIAN_POINT ( 'NONE',  ( 20.75514604977249178, 54.07500000273118701, 28.56700777964553950 ) ) ;
#5829 = CARTESIAN_POINT ( 'NONE',  ( 18.94512977948576093, 6.824999997268821339, -13.76444248337722875 ) ) ;
#5830 = CARTESIAN_POINT ( 'NONE',  ( 5.204170427930421283E-15, -70.99969134886156041, 0.000000000000000000 ) ) ;
#5831 = CARTESIAN_POINT ( 'NONE',  ( -33.58253175000000113, 3.025000002731199622, -10.91162601494193218 ) ) ;
#5832 = CARTESIAN_POINT ( 'NONE',  ( 13.94119854578937812, 42.79986083425731636, 24.22776226481240514 ) ) ;
#5833 = CARTESIAN_POINT ( 'NONE',  ( 22.22281446566211116, 16.99999999999998224, -7.541208221400177436 ) ) ;
#5834 = CARTESIAN_POINT ( 'NONE',  ( -20.82183453687059682, 52.00000000000002842, 25.59657189324412130 ) ) ;
#5835 = PRODUCT_DEFINITION_CONTEXT ( 'detailed design', #9647, 'design' ) ;
#5836 = CARTESIAN_POINT ( 'NONE',  ( 27.16883889988624290, 27.92500000273119554, 19.73931689729373673 ) ) ;
#5837 = CARTESIAN_POINT ( 'NONE',  ( 20.08610463437158344, 64.70000000000001705, 27.64615127144129403 ) ) ;
#5838 = DIRECTION ( 'NONE',  ( -0.7202789989107549751, -0.6936844842780617304, 8.820873705091161919E-17 ) ) ;
#5839 = CARTESIAN_POINT ( 'NONE',  ( 26.29305231718579350, 60.80000000000000426, 19.10302069950537529 ) ) ;
#5840 = CARTESIAN_POINT ( 'NONE',  ( -30.02300923189239867, 54.81993083240935505, 0.04044903255044988294 ) ) ;
#5841 = CARTESIAN_POINT ( 'NONE',  ( -10.04305231718578462, 56.90000000546240244, 30.90933677959249337 ) ) ;
#5842 = CARTESIAN_POINT ( 'NONE',  ( -8.960552108402742093E-16, 72.87500000273118417, -14.63369212191046387 ) ) ;
#5843 = CARTESIAN_POINT ( 'NONE',  ( 2.584737979205441561E-13, 14.14843749999999289, 27.95245687107222921 ) ) ;
#5844 = ORIENTED_EDGE ( 'NONE', *, *, #21954, .T. ) ;
#5845 = CARTESIAN_POINT ( 'NONE',  ( 32.50000000000000711, 69.40000000546235981, 10.55989012756945122 ) ) ;
#5846 = CARTESIAN_POINT ( 'NONE',  ( 30.02300923189239512, 33.91406249999997158, -2.619432448724977703E-13 ) ) ;
#5847 = CARTESIAN_POINT ( 'NONE',  ( 23.41746824999999887, 15.02499999726881086, 7.608796670333735079 ) ) ;
#5848 = ORIENTED_EDGE ( 'NONE', *, *, #27277, .T. ) ;
#5849 = CARTESIAN_POINT ( 'NONE',  ( -0.04044903254990864921, 39.64881916759063074, 30.02300923189239867 ) ) ;
#5850 = CARTESIAN_POINT ( 'NONE',  ( 20.08610463437158344, 17.20000000546236762, 27.64615127144129403 ) ) ;
#5851 = CARTESIAN_POINT ( 'NONE',  ( -26.00068869287340334, 52.53385416666666430, 15.01150461594643382 ) ) ;
#5852 = CARTESIAN_POINT ( 'NONE',  ( 32.50000000000000711, 74.89999999999999147, 10.55989012756945122 ) ) ;
#5853 = CARTESIAN_POINT ( 'NONE',  ( -33.58253175000000113, 45.37500000273120548, 0.000000000000000000 ) ) ;
#5854 = CARTESIAN_POINT ( 'NONE',  ( 20.08610463437157279, 49.80000000546238681, -27.64615127144129758 ) ) ;
#5855 = EDGE_CURVE ( 'NONE', #12435, #14813, #32666, .T. ) ;
#5856 = CARTESIAN_POINT ( 'NONE',  ( 13.91746824999999532, 80.47500000273119269, -4.522059556121118540 ) ) ;
#5857 = CARTESIAN_POINT ( 'NONE',  ( -20.75514604977248112, 33.42500000273120264, 28.56700777964554661 ) ) ;
#5858 = CYLINDRICAL_SURFACE ( 'NONE', #22003, 32.50000000000000000 ) ;
#5859 = CARTESIAN_POINT ( 'NONE',  ( 20.75514604977248467, 60.67500000273118133, -28.56700777964554305 ) ) ;
#5860 = CARTESIAN_POINT ( 'NONE',  ( 6.277390505771533514E-15, 1.000000005462384323, 34.17252228774368916 ) ) ;
#5861 = CARTESIAN_POINT ( 'NONE',  ( -27.16883889988623935, 53.32500000273120122, 19.73931689729374739 ) ) ;
#5862 = CARTESIAN_POINT ( 'NONE',  ( -10.04305231718579172, 41.60000000000000142, -30.90933677959248982 ) ) ;
#5863 = CARTESIAN_POINT ( 'NONE',  ( -4.523095164977116484E-15, 6.124999997268802510, 24.62258325217400312 ) ) ;
#5864 = CARTESIAN_POINT ( 'NONE',  ( 27.16883889988623935, 2.575000002731198112, -19.73931689729374384 ) ) ;
#5865 = CARTESIAN_POINT ( 'NONE',  ( -32.50000000000000000, 66.60000000546237686, 10.55989012756946366 ) ) ;
#5866 = CARTESIAN_POINT ( 'NONE',  ( -8.601468415847515203, 73.67500000273120975, 11.83890561707634959 ) ) ;
#5867 = CARTESIAN_POINT ( 'NONE',  ( 20.75514604977249178, 76.07500000273118701, 28.56700777964553950 ) ) ;
#5868 = CARTESIAN_POINT ( 'NONE',  ( -19.82091636218621389, 18.94999999453761319, 14.40073868116558842 ) ) ;
#5869 = CARTESIAN_POINT ( 'NONE',  ( -20.75514604977248112, 69.67500000273119554, 28.56700777964554661 ) ) ;
#5870 = ORIENTED_EDGE ( 'NONE', *, *, #30899, .F. ) ;
#5871 = CARTESIAN_POINT ( 'NONE',  ( 7.236395654485755280, 16.72499999726881370, 22.27133577429736988 ) ) ;
#5872 = CARTESIAN_POINT ( 'NONE',  ( -13.94119854578936923, 13.58111083425730925, -24.22776226481241224 ) ) ;
#5873 = SHAPE_REPRESENTATION ( 'BR-007', ( #10997, #15623, #11745, #5739, #24901, #33688, #18899, #4082, #798, #19990 ), #25216 ) ;
#5874 = DIRECTION ( 'NONE',  ( -0.000000000000000000, -1.000000000000000000, -0.000000000000000000 ) ) ;
#5875 = CARTESIAN_POINT ( 'NONE',  ( -33.58253175000000113, 45.02500000273117564, -10.91162601494193218 ) ) ;
#5876 = CARTESIAN_POINT ( 'NONE',  ( 33.58253175000000113, 8.475000002731185589, -10.91162601494193751 ) ) ;
#5877 = CARTESIAN_POINT ( 'NONE',  ( 20.75514604977248467, 64.67500000273116711, -28.56700777964554305 ) ) ;
#5878 = CARTESIAN_POINT ( 'NONE',  ( 27.95245687107223276, 51.10156249999998579, -2.463307335887066074E-13 ) ) ;
#5879 = CARTESIAN_POINT ( 'NONE',  ( -26.02091320914849959, 29.90923583425730925, 14.97647472619947528 ) ) ;
#5880 = VECTOR ( 'NONE', #24867, 1000.000000000000000 ) ;
#5881 = CARTESIAN_POINT ( 'NONE',  ( 28.00173670424535644, 32.33295166574267654, -7.543491769121920321 ) ) ;
#5882 = CARTESIAN_POINT ( 'NONE',  ( -20.08610463437157989, 72.20000000546237118, -27.64615127144129758 ) ) ;
#5883 = CARTESIAN_POINT ( 'NONE',  ( 11.25946833292375793, 76.07500000273120122, -8.180482586598735395 ) ) ;
#5884 = CARTESIAN_POINT ( 'NONE',  ( 10.37757302488624767, 35.72500000273118559, 31.93888565452638417 ) ) ;
#5885 = CARTESIAN_POINT ( 'NONE',  ( 24.18731323226221974, 42.50222249907603356, -14.01125832528328985 ) ) ;
#5886 = CARTESIAN_POINT ( 'NONE',  ( 7.236395654485760609, 17.02499999726880731, -22.27133577429736633 ) ) ;
#5887 = CYLINDRICAL_SURFACE ( 'NONE', #33662, 24.49999999999999645 ) ;
#5888 = ORIENTED_EDGE ( 'NONE', *, *, #24657, .F. ) ;
#5889 = CARTESIAN_POINT ( 'NONE',  ( -20.75514604977248112, 49.67500000273118133, 28.56700777964554661 ) ) ;
#5890 = CARTESIAN_POINT ( 'NONE',  ( -10.04305231718579172, 50.10000000546238397, -30.90933677959248982 ) ) ;
#5891 = CARTESIAN_POINT ( 'NONE',  ( -27.95245687107223986, 47.38319416759065206, -0.04044903254993292840 ) ) ;
#5892 = CARTESIAN_POINT ( 'NONE',  ( 6.486482029760649416E-15, 67.87500000273116996, 35.31076352940723240 ) ) ;
#5893 = VERTEX_POINT ( 'NONE', #3686 ) ;
#5894 = CARTESIAN_POINT ( 'NONE',  ( -10.37757302488624411, 20.72500000273118204, -31.93888565452638417 ) ) ;
#5895 = CARTESIAN_POINT ( 'NONE',  ( 20.50609665440969565, 23.17187499999999289, -20.50609665441004736 ) ) ;
#5896 = VERTEX_POINT ( 'NONE', #14834 ) ;
#5897 = CARTESIAN_POINT ( 'NONE',  ( -24.50000000000000711, 2.849999994537638859, 7.960532557706201828 ) ) ;
#5898 = CARTESIAN_POINT ( 'NONE',  ( 33.58253175000000113, 56.12500000273118417, -4.112674001490185761E-15 ) ) ;
#5899 = CARTESIAN_POINT ( 'NONE',  ( 30.02300923189239512, 51.10156249999998579, -2.619432448724977703E-13 ) ) ;
#5900 = EDGE_CURVE ( 'NONE', #1088, #9464, #33248, .T. ) ;
#5901 = VECTOR ( 'NONE', #855, 1000.000000000000000 ) ;
#5902 = CARTESIAN_POINT ( 'NONE',  ( -20.08610463437156923, 16.80000000546237970, 27.64615127144130113 ) ) ;
#5903 = CARTESIAN_POINT ( 'NONE',  ( 7.570916362186207671, 15.34999999453762243, 23.30088464923126779 ) ) ;
#5904 = CARTESIAN_POINT ( 'NONE',  ( -4.523095164977117273E-15, 10.62499999726880517, 24.62258325217400312 ) ) ;
#5905 = CARTESIAN_POINT ( 'NONE',  ( -33.58253175000000113, 25.47500000273118914, 10.91162601494193929 ) ) ;
#5906 = CARTESIAN_POINT ( 'NONE',  ( -26.29305231718579350, 63.80000000000001137, -19.10302069950537884 ) ) ;
#5907 = CARTESIAN_POINT ( 'NONE',  ( 28.00173670424535644, 66.70795166574268364, -7.543491769121920321 ) ) ;
#5908 = CARTESIAN_POINT ( 'NONE',  ( 13.91746824999999887, 79.87500000273118417, -1.704398294459741270E-15 ) ) ;
#5909 = CARTESIAN_POINT ( 'NONE',  ( -26.29305231718578995, 34.20000000000000995, 19.10302069950538595 ) ) ;
#5910 = CARTESIAN_POINT ( 'NONE',  ( 20.08610463437157279, 9.299999999999998934, -27.64615127144129758 ) ) ;
#5911 = ORIENTED_EDGE ( 'NONE', *, *, #26858, .T. ) ;
#5912 = CARTESIAN_POINT ( 'NONE',  ( -23.41746825000000598, 2.224999997268808816, 7.608796670333726198 ) ) ;
#5913 = CARTESIAN_POINT ( 'NONE',  ( 8.601468415847516980, 78.17500000273118133, -11.83890561707634781 ) ) ;
#5914 = CARTESIAN_POINT ( 'NONE',  ( -26.07999730980490583, 32.33854166666666430, -6.988114217767815717 ) ) ;
#5915 = CARTESIAN_POINT ( 'NONE',  ( -20.75514604977248823, 26.82500000273117280, -28.56700777964554305 ) ) ;
#5916 = CARTESIAN_POINT ( 'NONE',  ( -33.58253175000000113, 73.22500000273117848, 10.91162601494193929 ) ) ;
#5917 = CARTESIAN_POINT ( 'NONE',  ( -33.58253175000000113, 27.27500000273119340, -10.91162601494193218 ) ) ;
#5918 = CARTESIAN_POINT ( 'NONE',  ( 10.37757302488624056, 18.77500000273117564, -31.93888565452638417 ) ) ;
#5919 = CARTESIAN_POINT ( 'NONE',  ( 20.75514604977248467, 14.67500000273117955, -28.56700777964554305 ) ) ;
#5920 = CARTESIAN_POINT ( 'NONE',  ( -14.01125832528285109, 60.56027750092398065, 24.18731323226248264 ) ) ;
#5921 = CARTESIAN_POINT ( 'NONE',  ( 27.16883889988624290, 69.92500000273119554, 19.73931689729373673 ) ) ;
#5922 = FACE_OUTER_BOUND ( 'NONE', #29848, .T. ) ;
#5923 = CARTESIAN_POINT ( 'NONE',  ( -4.300734207923759378, 76.97500000273119269, -13.23629886949340495 ) ) ;
#5924 = CARTESIAN_POINT ( 'NONE',  ( -26.29305231718579350, 55.80000000000000426, -19.10302069950537884 ) ) ;
#5925 = CARTESIAN_POINT ( 'NONE',  ( 3.980102097228898626E-15, 80.00000000000001421, 32.50000000000000000 ) ) ;
#5926 = CARTESIAN_POINT ( 'NONE',  ( -27.16883889988624290, 54.92500000273120264, -19.73931689729374028 ) ) ;
#5927 = CARTESIAN_POINT ( 'NONE',  ( -23.41746825000000598, 12.22499999726881370, 7.608796670333726198 ) ) ;
#5928 = CIRCLE ( 'NONE', #25094, 13.38432950954957157 ) ;
#5929 = ORIENTED_EDGE ( 'NONE', *, *, #25577, .T. ) ;
#5930 = CARTESIAN_POINT ( 'NONE',  ( 6.486482029760649416E-15, 63.87500000273119127, 35.31076352940723240 ) ) ;
#5931 = CARTESIAN_POINT ( 'NONE',  ( -10.04305231718579172, 61.60000000000000142, -30.90933677959248982 ) ) ;
#5932 = CARTESIAN_POINT ( 'NONE',  ( 18.94512977948576093, 6.824999997268821339, -13.76444248337722875 ) ) ;
#5933 = CARTESIAN_POINT ( 'NONE',  ( -19.11951029504763611, 19.45350666759063785, 19.06425588902592239 ) ) ;
#5934 = VERTEX_POINT ( 'NONE', #32831 ) ;
#5935 = CARTESIAN_POINT ( 'NONE',  ( 6.486482029760649416E-15, 39.62500000273117706, 35.31076352940723240 ) ) ;
#5936 = VERTEX_POINT ( 'NONE', #27875 ) ;
#5937 = CARTESIAN_POINT ( 'NONE',  ( 7.505752307972854531, 53.82291666666666430, -28.01184896238303423 ) ) ;
#5938 = CARTESIAN_POINT ( 'NONE',  ( 15.00000000000000000, 75.25000000546239676, -1.836970198721029589E-15 ) ) ;
#5939 = CARTESIAN_POINT ( 'NONE',  ( 10.37757302488624056, 76.52500000273118985, -31.93888565452638417 ) ) ;
#5940 = CARTESIAN_POINT ( 'NONE',  ( -30.02300923189239512, 21.88281249999999645, 2.654126918244515359E-13 ) ) ;
#5941 = CARTESIAN_POINT ( 'NONE',  ( 1.577395562988744260E-15, 6.499999999999998224, -25.76082449383753925 ) ) ;
#5942 = ADVANCED_FACE ( 'NONE', ( #14160 ), #9321, .T. ) ;
#5943 = CARTESIAN_POINT ( 'NONE',  ( -20.75514604977248823, 9.075000002731183457, -28.56700777964554305 ) ) ;
#5944 = ADVANCED_FACE ( 'NONE', ( #9161 ), #1769, .T. ) ;
#5945 = CARTESIAN_POINT ( 'NONE',  ( 6.486482029760649416E-15, 13.62500000273118417, 35.31076352940723240 ) ) ;
#5946 = CARTESIAN_POINT ( 'NONE',  ( -8.960552108402744065E-16, 80.37500000273116996, -14.63369212191046209 ) ) ;
#5947 = CARTESIAN_POINT ( 'NONE',  ( 0.000000000000000000, 80.00000000000001421, 0.000000000000000000 ) ) ;
#5948 = CARTESIAN_POINT ( 'NONE',  ( -28.00173670424535644, 30.61420166574267654, 7.543491769121936308 ) ) ;
#5949 = CARTESIAN_POINT ( 'NONE',  ( -4.635254915624208216, 78.39999999999999147, 14.26584774442730463 ) ) ;
#5950 = CARTESIAN_POINT ( 'NONE',  ( -20.50609665440969209, 45.51562500000000000, 20.50609665441005092 ) ) ;
#5951 = CARTESIAN_POINT ( 'NONE',  ( 10.04305231718579705, 53.10000000546237686, 30.90933677959248982 ) ) ;
#5952 = CARTESIAN_POINT ( 'NONE',  ( -24.22776226481266448, 65.41888916574268364, -13.94119854578892514 ) ) ;
#5953 = CARTESIAN_POINT ( 'NONE',  ( -20.75514604977248823, 44.82500000273117990, -28.56700777964554305 ) ) ;
#5954 = CARTESIAN_POINT ( 'NONE',  ( 11.25946833292375793, 79.67500000273119554, 8.180482586598731842 ) ) ;
#5955 = CARTESIAN_POINT ( 'NONE',  ( 10.37757302488624056, 50.77500000273120406, -31.93888565452638417 ) ) ;
#5956 = CARTESIAN_POINT ( 'NONE',  ( 10.37757302488624056, 32.77500000273120406, -31.93888565452638417 ) ) ;
#5957 = DIRECTION ( 'NONE',  ( 0.000000000000000000, 0.000000000000000000, -1.000000000000000000 ) ) ;
#5958 = CARTESIAN_POINT ( 'NONE',  ( 6.988114217767829928, 19.44791666666666075, -26.07999730980489872 ) ) ;
#5959 = CARTESIAN_POINT ( 'NONE',  ( 0.000000000000000000, 16.99999999999998579, -24.50000000000000000 ) ) ;
#5960 = ADVANCED_FACE ( 'NONE', ( #22727 ), #11573, .T. ) ;
#5961 = CARTESIAN_POINT ( 'NONE',  ( 0.000000000000000000, 102.0000000000000284, -9.000000000000001776 ) ) ;
#5962 = CARTESIAN_POINT ( 'NONE',  ( -32.50000000000000000, 76.10000000000002274, 10.55989012756946366 ) ) ;
#5963 = CARTESIAN_POINT ( 'NONE',  ( -27.16883889988624290, 8.925000002731206195, -19.73931689729374028 ) ) ;
#5964 = CARTESIAN_POINT ( 'NONE',  ( 14.47279130897151767, 4.324999997268800911, 19.92008829642072953 ) ) ;
#5965 = LINE ( 'NONE', #1124, #25328 ) ;
#5966 = CARTESIAN_POINT ( 'NONE',  ( 13.94119854578893580, 31.90326416574268364, -24.22776226481265383 ) ) ;
#5967 =( BOUNDED_CURVE ( )  B_SPLINE_CURVE ( 2, ( #14739, #15255, #9403, #19719, #30166, #6670, #27608, #30339, #11985, #17317, #1678, #25200, #22627 ),
 .UNSPECIFIED., .F., .T. ) 
 B_SPLINE_CURVE_WITH_KNOTS ( ( 3, 2, 2, 2, 2, 2, 3 ),
 ( 0.4679487179487179516, 0.4692307692307692291, 0.4717948717948717841, 0.4743589743589743390, 0.4769230769230769496, 0.4794871794871795045, 0.4807692307692307820 ),
 .UNSPECIFIED. ) 
 CURVE ( )  GEOMETRIC_REPRESENTATION_ITEM ( )  RATIONAL_B_SPLINE_CURVE ( ( 0.9755282581475768211, 0.9755282581475768211, 1.000000000000000000, 0.9510565162951535312, 1.000000000000000000, 0.9510565162951535312, 1.000000000000000000, 0.9510565162951535312, 1.000000000000000000, 0.9510565162951535312, 1.000000000000000000, 0.9755282581475768211, 0.9755282581475768211 ) ) 
 REPRESENTATION_ITEM ( '' )  );
#5968 = CARTESIAN_POINT ( 'NONE',  ( -24.50000000000000000, 13.00000000000001066, -3.000384657911015469E-15 ) ) ;
#5969 = CARTESIAN_POINT ( 'NONE',  ( 27.16883889988623935, 18.32500000273118346, -19.73931689729374384 ) ) ;
#5970 = CARTESIAN_POINT ( 'NONE',  ( -18.94512977948576093, 8.324999997268822227, 13.76444248337722698 ) ) ;
#5971 = CARTESIAN_POINT ( 'NONE',  ( -19.09188309203694445, 49.81249999999999289, -19.09188309203661049 ) ) ;
#5972 = ORIENTED_EDGE ( 'NONE', *, *, #30747, .F. ) ;
#5973 = CARTESIAN_POINT ( 'NONE',  ( 20.75514604977249178, 55.82500000273119412, 28.56700777964553950 ) ) ;
#5974 = ORIENTED_EDGE ( 'NONE', *, *, #8471, .T. ) ;
#5975 = CARTESIAN_POINT ( 'NONE',  ( -7.505752307973343918, 22.59895833333332860, -28.01184896238290989 ) ) ;
#5976 = CARTESIAN_POINT ( 'NONE',  ( 26.02091320914851025, 24.75298583425730925, -14.97647472619946463 ) ) ;
#5977 = CARTESIAN_POINT ( 'NONE',  ( -27.16883889988623935, 1.325000002731183013, 19.73931689729374739 ) ) ;
#5978 = CARTESIAN_POINT ( 'NONE',  ( -23.41746825000000243, 7.524999997268816188, -7.608796670333730638 ) ) ;
#5979 = CARTESIAN_POINT ( 'NONE',  ( -10.37757302488623701, 29.77500000273120051, 31.93888565452638417 ) ) ;
#5980 = CARTESIAN_POINT ( 'NONE',  ( -20.08610463437156923, 28.80000000546238326, 27.64615127144130113 ) ) ;
#5981 = CARTESIAN_POINT ( 'NONE',  ( 32.50000000000000000, 77.09999999999998010, -10.55989012756945833 ) ) ;
#5982 = CARTESIAN_POINT ( 'NONE',  ( 20.08610463437158344, 52.69999999999998863, 27.64615127144129403 ) ) ;
#5983 = DIRECTION ( 'NONE',  ( -0.000000000000000000, -1.000000000000000000, -0.000000000000000000 ) ) ;
#5984 = CARTESIAN_POINT ( 'NONE',  ( -33.58253175000000113, 43.27500000273117564, -10.91162601494193218 ) ) ;
#5985 = CARTESIAN_POINT ( 'NONE',  ( -32.50000000000000000, 21.90000000000000924, -10.55989012756945478 ) ) ;
#5986 = CARTESIAN_POINT ( 'NONE',  ( 20.08610463437158344, 18.69999999999998863, 27.64615127144129403 ) ) ;
#5987 = CARTESIAN_POINT ( 'NONE',  ( 1.577395562988744260E-15, 14.50000000000000888, -25.76082449383753925 ) ) ;
#5988 = CARTESIAN_POINT ( 'NONE',  ( 33.58253175000000823, 66.02500000273118985, 10.91162601494192863 ) ) ;
#5989 = CARTESIAN_POINT ( 'NONE',  ( -33.58253175000000113, 55.37500000273118417, 0.000000000000000000 ) ) ;
#5990 = CARTESIAN_POINT ( 'NONE',  ( -4.523095164977117273E-15, 10.12499999726882116, 24.62258325217400312 ) ) ;
#5991 = ADVANCED_FACE ( 'NONE', ( #33176 ), #1090, .T. ) ;
#5992 = CARTESIAN_POINT ( 'NONE',  ( 26.29305231718579350, 39.30000000546237970, 19.10302069950537529 ) ) ;
#5993 = CARTESIAN_POINT ( 'NONE',  ( -2.162160676586881955E-15, 8.625000002731169957, -35.31076352940723240 ) ) ;
#5994 = CARTESIAN_POINT ( 'NONE',  ( 26.09010956794232428, 35.20871500092396644, -6.950374756619718042 ) ) ;
#5995 = CARTESIAN_POINT ( 'NONE',  ( 23.41787895562451638, 16.99999999999998224, 0.7516208871782403822 ) ) ;
#5996 = CARTESIAN_POINT ( 'NONE',  ( 12.90513655866702081, 52.00000000000000711, 31.00393344628893288 ) ) ;
#5997 = CARTESIAN_POINT ( 'NONE',  ( 33.58253175000000823, 30.02500000273118985, 10.91162601494192863 ) ) ;
#5998 = CARTESIAN_POINT ( 'NONE',  ( -10.04305231718579172, 18.10000000546238397, -30.90933677959248982 ) ) ;
#5999 = CARTESIAN_POINT ( 'NONE',  ( -1.778240108872766143E-15, 39.50000000000000000, -32.49999999999999289 ) ) ;
#6000 = EDGE_CURVE ( 'NONE', #16286, #19940, #15709, .T. ) ;
#6001 = CARTESIAN_POINT ( 'NONE',  ( -26.29305231718578995, 30.70000000546238539, 19.10302069950538595 ) ) ;
#6002 = CARTESIAN_POINT ( 'NONE',  ( 7.468012846824281681, 55.82253499907601935, -28.02196122052058058 ) ) ;
#6003 = CARTESIAN_POINT ( 'NONE',  ( -10.04305231718579172, 46.10000000546236976, -30.90933677959248982 ) ) ;
#6004 = CARTESIAN_POINT ( 'NONE',  ( 13.91746824999999532, 72.47500000273116427, -4.522059556121118540 ) ) ;
#6005 = FACE_OUTER_BOUND ( 'NONE', #24619, .T. ) ;
#6006 = CARTESIAN_POINT ( 'NONE',  ( 2.584737979205441561E-13, 27.89843750000000000, 27.95245687107222921 ) ) ;
#6007 = ORIENTED_EDGE ( 'NONE', *, *, #23213, .T. ) ;
#6008 = CARTESIAN_POINT ( 'NONE',  ( -20.75514604977248823, 74.82500000273115859, -28.56700777964554305 ) ) ;
#6009 = CARTESIAN_POINT ( 'NONE',  ( 20.50609665441005092, 27.46875000000000000, 20.50609665440969209 ) ) ;
#6010 = CARTESIAN_POINT ( 'NONE',  ( 0.000000000000000000, 86.00000000000001421, 15.00000000000000000 ) ) ;
#6011 = ORIENTED_EDGE ( 'NONE', *, *, #25422, .F. ) ;
#6012 = CARTESIAN_POINT ( 'NONE',  ( 0.04044903254992426173, 48.24256916759064495, -30.02300923189239867 ) ) ;
#6013 = CARTESIAN_POINT ( 'NONE',  ( 32.50000000000000000, 15.60000000546238930, -10.55989012756945833 ) ) ;
#6014 = CARTESIAN_POINT ( 'NONE',  ( 15.01150461594643204, 51.67447916666665719, 26.00068869287340334 ) ) ;
#6015 = CARTESIAN_POINT ( 'NONE',  ( 0.000000000000000000, 82.00000000000001421, -15.00000000000000000 ) ) ;
#6016 = CARTESIAN_POINT ( 'NONE',  ( 33.58253175000000113, 44.47500000273119269, -10.91162601494193751 ) ) ;
#6017 = CARTESIAN_POINT ( 'NONE',  ( 20.08610463437157279, 51.80000000546238681, -27.64615127144129758 ) ) ;
#6018 = FACE_OUTER_BOUND ( 'NONE', #20548, .T. ) ;
#6019 = CARTESIAN_POINT ( 'NONE',  ( 27.16883889988624290, 33.92500000273118843, 19.73931689729373673 ) ) ;
#6020 = CARTESIAN_POINT ( 'NONE',  ( 3.880418787951140036, 12.44874571845315714, -24.49999999999999645 ) ) ;
#6021 = CARTESIAN_POINT ( 'NONE',  ( -27.16883889988624290, 61.17500000273118133, -19.73931689729374028 ) ) ;
#6022 = CARTESIAN_POINT ( 'NONE',  ( -2.092463501923844636E-15, 41.49999999999999289, -34.17252228774368916 ) ) ;
#6023 = CARTESIAN_POINT ( 'NONE',  ( 7.236395654485760609, 11.02499999726880375, -22.27133577429736633 ) ) ;
#6024 = CARTESIAN_POINT ( 'NONE',  ( -27.16883889988624290, 7.175000002731191096, -19.73931689729374028 ) ) ;
#6025 = CARTESIAN_POINT ( 'NONE',  ( -1.778240108872766143E-15, 13.50000000000000355, -32.49999999999999289 ) ) ;
#6026 = CARTESIAN_POINT ( 'NONE',  ( -11.25946833292375793, 73.17500000273119554, -8.180482586598733619 ) ) ;
#6027 = CARTESIAN_POINT ( 'NONE',  ( -2.162160676586882350E-15, 70.87500000273118417, -35.31076352940722529 ) ) ;
#6028 = PLANE ( 'NONE',  #24267 ) ;
#6029 = CARTESIAN_POINT ( 'NONE',  ( 20.75514604977248467, 68.67500000273119554, -28.56700777964554305 ) ) ;
#6030 = EDGE_LOOP ( 'NONE', ( #6257, #20026, #21017, #16041 ) ) ;
#6031 = CARTESIAN_POINT ( 'NONE',  ( -19.82091636218621389, 6.949999994537630954, 14.40073868116558842 ) ) ;
#6032 = CARTESIAN_POINT ( 'NONE',  ( 27.95245687107223986, 11.28944416759064140, 0.04044903254993640479 ) ) ;
#6033 = DIRECTION ( 'NONE',  ( 0.000000000000000000, -1.000000000000000000, 0.000000000000000000 ) ) ;
#6034 = CARTESIAN_POINT ( 'NONE',  ( -27.16883889988624290, 44.92500000273118133, -19.73931689729374028 ) ) ;
#6035 = CARTESIAN_POINT ( 'NONE',  ( 10.37757302488624767, 9.975000002731201576, 31.93888565452638417 ) ) ;
#6036 = CARTESIAN_POINT ( 'NONE',  ( -33.58253175000000113, 65.27500000273117564, -10.91162601494193041 ) ) ;
#6037 = CARTESIAN_POINT ( 'NONE',  ( 13.97622843553633842, 48.23697916666665009, 24.20753774853730889 ) ) ;
#6038 = CARTESIAN_POINT ( 'NONE',  ( -7.543491769121417612, 43.22954833425730925, 28.00173670424549499 ) ) ;
#6039 = CARTESIAN_POINT ( 'NONE',  ( 20.47846945139867003, 25.17149333240934439, -20.53372385742107653 ) ) ;
#6040 = CARTESIAN_POINT ( 'NONE',  ( 32.50000000000000000, 65.50000000546239676, -3.980102097228898626E-15 ) ) ;
#6041 = CARTESIAN_POINT ( 'NONE',  ( -19.11951029504797006, 55.24961833240936926, -19.06425588902558133 ) ) ;
#6042 = CARTESIAN_POINT ( 'NONE',  ( -23.41746825000000598, 15.72499999726882081, 7.608796670333726198 ) ) ;
#6043 = CARTESIAN_POINT ( 'NONE',  ( 5.779280353836490358E-15, 58.49999999999999289, 32.49999999999999289 ) ) ;
#6044 = VERTEX_POINT ( 'NONE', #15005 ) ;
#6045 = CARTESIAN_POINT ( 'NONE',  ( 27.16883889988624290, 48.17500000273118843, 19.73931689729373673 ) ) ;
#6046 = LINE ( 'NONE', #10537, #22310 ) ;
#6047 = CARTESIAN_POINT ( 'NONE',  ( -19.06425588902591173, 47.81288166759064495, -19.11951029504763611 ) ) ;
#6048 = CARTESIAN_POINT ( 'NONE',  ( 20.75514604977248467, 66.67500000273119554, -28.56700777964554305 ) ) ;
#6049 = VERTEX_POINT ( 'NONE', #17755 ) ;
#6050 = CARTESIAN_POINT ( 'NONE',  ( -33.58253175000000113, 15.02500000273120051, -10.91162601494193218 ) ) ;
#6051 = CARTESIAN_POINT ( 'NONE',  ( 2.740863092043355209E-13, 27.89843750000000000, 30.02300923189239512 ) ) ;
#6052 = EDGE_LOOP ( 'NONE', ( #5813, #19315, #32477, #20167 ) ) ;
#6053 = CARTESIAN_POINT ( 'NONE',  ( -24.50000000000000000, 2.649999994537616477, -7.960532557706207157 ) ) ;
#6054 = CARTESIAN_POINT ( 'NONE',  ( 33.58253175000000823, 54.02500000273118275, 10.91162601494192863 ) ) ;
#6055 = CARTESIAN_POINT ( 'NONE',  ( -7.505752307973343918, 56.97395833333333570, -28.01184896238290989 ) ) ;
#6056 = CARTESIAN_POINT ( 'NONE',  ( -26.29305231718578995, 12.70000000546239782, 19.10302069950538595 ) ) ;
#6057 = CARTESIAN_POINT ( 'NONE',  ( -10.04305231718579172, 66.10000000546237686, -30.90933677959248982 ) ) ;
#6058 = CARTESIAN_POINT ( 'NONE',  ( -7.236395654485757944, 11.72499999726880837, -22.27133577429736988 ) ) ;
#6059 =( BOUNDED_CURVE ( )  B_SPLINE_CURVE ( 2, ( #21452, #13048, #26426, #5659, #10473, #10978, #16142, #20951, #29153, #23860, #5491, #8223, #2919 ),
 .UNSPECIFIED., .F., .T. ) 
 B_SPLINE_CURVE_WITH_KNOTS ( ( 3, 2, 2, 2, 2, 2, 3 ),
 ( 0.01923076923076923184, 0.02051282051282051280, 0.02307692307692307820, 0.02564102564102564014, 0.02820512820512820554, 0.03076923076923077094, 0.03205128205128205537 ),
 .UNSPECIFIED. ) 
 CURVE ( )  GEOMETRIC_REPRESENTATION_ITEM ( )  RATIONAL_B_SPLINE_CURVE ( ( 0.9755282581475768211, 0.9755282581475768211, 1.000000000000000000, 0.9510565162951535312, 1.000000000000000000, 0.9510565162951535312, 1.000000000000000000, 0.9510565162951535312, 1.000000000000000000, 0.9510565162951535312, 1.000000000000000000, 0.9755282581475767101, 0.9755282581475768211 ) ) 
 REPRESENTATION_ITEM ( '' )  );
#6060 = CARTESIAN_POINT ( 'NONE',  ( 20.75514604977248467, 20.67500000273119909, -28.56700777964554305 ) ) ;
#6061 = CARTESIAN_POINT ( 'NONE',  ( 9.270509831248421762, 77.30000000000001137, -12.75976212528059861 ) ) ;
#6062 = CARTESIAN_POINT ( 'NONE',  ( -28.00173670424535644, 68.42670166574269786, 7.543491769121936308 ) ) ;
#6063 = CARTESIAN_POINT ( 'NONE',  ( -32.50000000000000000, 31.90000000000001279, -10.55989012756945300 ) ) ;
#6064 = CARTESIAN_POINT ( 'NONE',  ( 32.50000000000000000, 15.00000000000001421, -3.980102097228898626E-15 ) ) ;
#6065 = CARTESIAN_POINT ( 'NONE',  ( 32.50000000000000000, 11.09999999999999964, -10.55989012756945833 ) ) ;
#6066 = EDGE_LOOP ( 'NONE', ( #24212, #28178, #1818, #30429 ) ) ;
#6067 = CARTESIAN_POINT ( 'NONE',  ( -23.41746825000000243, 2.024999997268815299, -7.608796670333730638 ) ) ;
#6068 = CARTESIAN_POINT ( 'NONE',  ( 11.25946833292375793, 76.07500000273120122, -8.180482586598735395 ) ) ;
#6069 = CARTESIAN_POINT ( 'NONE',  ( -19.09188309203660694, 38.64062500000000000, 19.09188309203694800 ) ) ;
#6070 = CARTESIAN_POINT ( 'NONE',  ( 33.58253175000000823, 26.02500000273120406, 10.91162601494192863 ) ) ;
#6071 = CARTESIAN_POINT ( 'NONE',  ( 10.37757302488624767, 69.72500000273117848, 31.93888565452638417 ) ) ;
#6072 = CARTESIAN_POINT ( 'NONE',  ( 33.58253175000000823, 32.27500000273117564, 10.91162601494192863 ) ) ;
#6073 = CARTESIAN_POINT ( 'NONE',  ( 33.58253175000000113, 14.37500000273118950, -4.112674001490185761E-15 ) ) ;
#6074 = CARTESIAN_POINT ( 'NONE',  ( -20.75514604977248823, 9.075000002731183457, -28.56700777964554305 ) ) ;
#6075 = CARTESIAN_POINT ( 'NONE',  ( -26.02091320914849959, 16.15923583425731636, 14.97647472619947528 ) ) ;
#6076 = CARTESIAN_POINT ( 'NONE',  ( -33.58253175000000113, 71.12500000273119838, 0.000000000000000000 ) ) ;
#6077 = CARTESIAN_POINT ( 'NONE',  ( 28.01184896238290278, 54.39583333333332860, -7.505752307973347470 ) ) ;
#6078 = DIRECTION ( 'NONE',  ( 0.000000000000000000, 1.000000000000000000, 0.000000000000000000 ) ) ;
#6079 = ADVANCED_FACE ( 'NONE', ( #20329 ), #33529, .T. ) ;
#6080 = CARTESIAN_POINT ( 'NONE',  ( -8.601468415847515203, 77.67500000273119554, 11.83890561707634959 ) ) ;
#6081 = CARTESIAN_POINT ( 'NONE',  ( 20.08610463437157279, 45.29999999999999005, -27.64615127144129758 ) ) ;
#6082 = CARTESIAN_POINT ( 'NONE',  ( 5.779280353836490358E-15, 62.50000000000000000, 32.49999999999999289 ) ) ;
#6083 = CARTESIAN_POINT ( 'NONE',  ( 20.75514604977249178, 57.82500000273119412, 28.56700777964553950 ) ) ;
#6084 = EDGE_CURVE ( 'NONE', #22217, #28718, #4700, .T. ) ;
#6085 = CARTESIAN_POINT ( 'NONE',  ( -23.41746825000000243, 16.02499999726881086, -7.608796670333730638 ) ) ;
#6086 = ORIENTED_EDGE ( 'NONE', *, *, #3699, .T. ) ;
#6087 = CARTESIAN_POINT ( 'NONE',  ( 20.75514604977248467, 66.67500000273119554, -28.56700777964554305 ) ) ;
#6088 = CARTESIAN_POINT ( 'NONE',  ( 6.486482029760648627E-15, 3.625000002731181059, 35.31076352940722529 ) ) ;
#6089 = CARTESIAN_POINT ( 'NONE',  ( -23.41746824999999887, 5.624999997268814944, -2.867812753649727150E-15 ) ) ;
#6090 = CARTESIAN_POINT ( 'NONE',  ( -26.06988505166735237, 23.46392333425730570, -7.025853678916388567 ) ) ;
#6091 = EDGE_LOOP ( 'NONE', ( #31801, #8832, #9717, #730 ) ) ;
#6092 = CARTESIAN_POINT ( 'NONE',  ( -27.16883889988623935, 35.32500000273118701, 19.73931689729374739 ) ) ;
#6093 = CARTESIAN_POINT ( 'NONE',  ( -1.778240108872766143E-15, 55.49999999999999289, -32.49999999999999289 ) ) ;
#6094 = VECTOR ( 'NONE', #20087, 1000.000000000000000 ) ;
#6095 = ORIENTED_EDGE ( 'NONE', *, *, #9343, .T. ) ;
#6096 = CARTESIAN_POINT ( 'NONE',  ( 2.740863092043355209E-13, 51.96093750000000000, 30.02300923189239512 ) ) ;
#6097 = CARTESIAN_POINT ( 'NONE',  ( -20.08610463437156923, 60.80000000546238681, 27.64615127144130113 ) ) ;
#6098 = DIRECTION ( 'NONE',  ( 0.000000000000000000, 1.000000000000000000, 0.000000000000000000 ) ) ;
#6099 = CARTESIAN_POINT ( 'NONE',  ( 33.58253175000000823, 72.02500000273118985, 10.91162601494192863 ) ) ;
#6100 = CARTESIAN_POINT ( 'NONE',  ( 28.01184896238290278, 30.33333333333332860, -7.505752307973347470 ) ) ;
#6101 = CARTESIAN_POINT ( 'NONE',  ( 7.570916362186213000, 8.399999999999991473, -23.30088464923126423 ) ) ;
#6102 = CARTESIAN_POINT ( 'NONE',  ( 6.486482029760649416E-15, 11.87500000273118062, 35.31076352940723240 ) ) ;
#6103 = CARTESIAN_POINT ( 'NONE',  ( -33.58253175000000113, 17.02500000273118985, -10.91162601494193218 ) ) ;
#6104 = CARTESIAN_POINT ( 'NONE',  ( 8.601468415847520532, 75.57500000273120122, 11.83890561707634603 ) ) ;
#6105 = CARTESIAN_POINT ( 'NONE',  ( -4.223320258572819786E-15, 9.499999999999992895, 24.50000000000000000 ) ) ;
#6106 = CARTESIAN_POINT ( 'NONE',  ( 14.97647472619900455, 45.65326416574269786, -26.02091320914876960 ) ) ;
#6107 = AXIS2_PLACEMENT_3D ( 'NONE', #21939, #32227, #8716 ) ;
#6108 = CARTESIAN_POINT ( 'NONE',  ( 8.601468415847516980, 72.67500000273118133, -11.83890561707634781 ) ) ;
#6109 = CARTESIAN_POINT ( 'NONE',  ( 30.02300923189239867, 51.10156249999998579, -2.619432448724978208E-13 ) ) ;
#6110 = DIRECTION ( 'NONE',  ( 0.000000000000000000, -1.000000000000000000, 0.000000000000000000 ) ) ;
#6111 = CARTESIAN_POINT ( 'NONE',  ( -26.06988505166722803, 68.42670166574269786, 7.025853678916877953 ) ) ;
#6112 = CARTESIAN_POINT ( 'NONE',  ( -2.162160676586881955E-15, 46.62500000273119127, -35.31076352940723240 ) ) ;
#6113 = CARTESIAN_POINT ( 'NONE',  ( 13.91746824999999532, 77.97500000273122112, -4.522059556121118540 ) ) ;
#6114 = CARTESIAN_POINT ( 'NONE',  ( 33.58253175000000113, 46.47500000273118559, -10.91162601494193751 ) ) ;
#6115 = CARTESIAN_POINT ( 'NONE',  ( -33.58253175000000113, 31.37500000273119127, 0.000000000000000000 ) ) ;
#6116 = LINE ( 'NONE', #11767, #18567 ) ;
#6117 = CARTESIAN_POINT ( 'NONE',  ( -24.20753774853730889, 25.03385416666666430, 13.97622843553634020 ) ) ;
#6118 = CARTESIAN_POINT ( 'NONE',  ( 6.001560367445586717E-15, 1.500000000000005995, 24.50000000000000000 ) ) ;
#6119 = EDGE_CURVE ( 'NONE', #6044, #5934, #12427, .T. ) ;
#6120 = CARTESIAN_POINT ( 'NONE',  ( -4.635254915624208216, 76.40000000000001990, 14.26584774442730463 ) ) ;
#6121 = CARTESIAN_POINT ( 'NONE',  ( 26.29305231718579350, 70.80000000000001137, 19.10302069950537529 ) ) ;
#6122 = CARTESIAN_POINT ( 'NONE',  ( -33.58253175000000113, 9.125000002731184168, 0.000000000000000000 ) ) ;
#6123 = CARTESIAN_POINT ( 'NONE',  ( -18.94512977948576093, 5.824999997268820451, 13.76444248337722698 ) ) ;
#6124 = DIRECTION ( 'NONE',  ( 0.000000000000000000, 0.000000000000000000, 1.000000000000000000 ) ) ;
#6125 = CARTESIAN_POINT ( 'NONE',  ( -24.22776226481266448, 31.04388916574268364, -13.94119854578892514 ) ) ;
#6126 = CARTESIAN_POINT ( 'NONE',  ( -32.50000000000000000, 59.89999999999999147, -10.55989012756945300 ) ) ;
#6127 = CARTESIAN_POINT ( 'NONE',  ( -10.37757302488623701, 19.52500000273118985, 31.93888565452638417 ) ) ;
#6128 = CARTESIAN_POINT ( 'NONE',  ( -23.41746825000000243, 4.024999997268810858, -7.608796670333730638 ) ) ;
#6129 = CARTESIAN_POINT ( 'NONE',  ( 19.09188309203661049, 54.10937499999999289, -19.09188309203694445 ) ) ;
#6130 = VERTEX_POINT ( 'NONE', #33876 ) ;
#6131 = CARTESIAN_POINT ( 'NONE',  ( 10.37757302488624056, 54.52500000273118275, -31.93888565452638417 ) ) ;
#6132 = ORIENTED_EDGE ( 'NONE', *, *, #19308, .T. ) ;
#6133 = CARTESIAN_POINT ( 'NONE',  ( 28.01184896238304134, 27.18229166666666430, 7.505752307972846538 ) ) ;
#6134 = CARTESIAN_POINT ( 'NONE',  ( -20.47846945139902175, 20.31288166759063785, -20.53372385742072481 ) ) ;
#6135 = CARTESIAN_POINT ( 'NONE',  ( 24.50000000000000000, 15.74999999453763344, 0.000000000000000000 ) ) ;
#6136 = APPLICATION_CONTEXT ( 'automotive_design' ) ;
#6137 = CARTESIAN_POINT ( 'NONE',  ( 1.507698388325705758E-15, 3.124999997268809615, -24.62258325217400312 ) ) ;
#6138 = CARTESIAN_POINT ( 'NONE',  ( 6.486482029760649416E-15, 29.87500000273119838, 35.31076352940723240 ) ) ;
#6139 = CARTESIAN_POINT ( 'NONE',  ( -10.04305231718579172, 32.10000000546236976, -30.90933677959248982 ) ) ;
#6140 = CARTESIAN_POINT ( 'NONE',  ( -26.29305231718579350, 71.79999999999999716, -19.10302069950537884 ) ) ;
#6141 = DIRECTION ( 'NONE',  ( 1.224646799147353454E-16, -1.000000000000000000, 0.000000000000000000 ) ) ;
#6142 = CYLINDRICAL_SURFACE ( 'NONE', #32382, 32.50000000000000000 ) ;
#6143 = CARTESIAN_POINT ( 'NONE',  ( -20.53372385742071771, 57.26600666759063785, 20.47846945139902530 ) ) ;
#6144 = CARTESIAN_POINT ( 'NONE',  ( -20.75514604977248112, 41.67500000273117422, 28.56700777964554661 ) ) ;
#6145 = CARTESIAN_POINT ( 'NONE',  ( 1.507698388325705758E-15, 11.62499999726880340, -24.62258325217400312 ) ) ;
#6146 = CARTESIAN_POINT ( 'NONE',  ( -26.29305231718578995, 18.19999999999999574, 19.10302069950538595 ) ) ;
#6147 = CARTESIAN_POINT ( 'NONE',  ( -19.82091636218621034, 8.800000000000002487, -14.40073868116559552 ) ) ;
#6148 = CARTESIAN_POINT ( 'NONE',  ( 19.06425588902558133, 35.48399333240935505, -19.11951029504797006 ) ) ;
#6149 = CARTESIAN_POINT ( 'NONE',  ( -20.75514604977248112, 65.42500000273118133, 28.56700777964554661 ) ) ;
#6150 = CARTESIAN_POINT ( 'NONE',  ( 10.37757302488624767, 53.97500000273119980, 31.93888565452638417 ) ) ;
#6151 = VECTOR ( 'NONE', #5983, 1000.000000000000000 ) ;
#6152 = CARTESIAN_POINT ( 'NONE',  ( 7.236395654485760609, 11.02499999726880375, -22.27133577429736633 ) ) ;
#6153 = CARTESIAN_POINT ( 'NONE',  ( 5.779280353836490358E-15, 39.00000000546237544, 32.49999999999999289 ) ) ;
#6154 = CARTESIAN_POINT ( 'NONE',  ( -20.75514604977248823, 6.825000002731195892, -28.56700777964554305 ) ) ;
#6155 = CARTESIAN_POINT ( 'NONE',  ( 14.01125832528286352, 41.65402750092398065, -24.18731323226246843 ) ) ;
#6156 =( BOUNDED_CURVE ( )  B_SPLINE_CURVE ( 2, ( #5168, #10153, #15478, #10489, #17709, #20635, #33479, #9980, #2425, #23368, #18394, #25763, #13062 ),
 .UNSPECIFIED., .F., .T. ) 
 B_SPLINE_CURVE_WITH_KNOTS ( ( 3, 2, 2, 2, 2, 2, 3 ),
 ( 0.1858974358974359031, 0.1871794871794871806, 0.1897435897435897356, 0.1923076923076923184, 0.1948717948717948734, 0.1974358974358974284, 0.1987179487179487336 ),
 .UNSPECIFIED. ) 
 CURVE ( )  GEOMETRIC_REPRESENTATION_ITEM ( )  RATIONAL_B_SPLINE_CURVE ( ( 0.9755282581475768211, 0.9755282581475768211, 1.000000000000000000, 0.9510565162951535312, 1.000000000000000000, 0.9510565162951535312, 1.000000000000000000, 0.9510565162951535312, 1.000000000000000000, 0.9510565162951535312, 1.000000000000000000, 0.9755282581475764880, 0.9755282581475768211 ) ) 
 REPRESENTATION_ITEM ( '' )  );
#6157 = FACE_OUTER_BOUND ( 'NONE', #6091, .T. ) ;
#6158 = CYLINDRICAL_SURFACE ( 'NONE', #30257, 32.50000000000000000 ) ;
#6159 = UNCERTAINTY_MEASURE_WITH_UNIT (LENGTH_MEASURE( 1.000000000000000082E-05 ), #146, 'distance_accuracy_value', 'NONE');
#6160 = CARTESIAN_POINT ( 'NONE',  ( 27.16883889988623935, 26.32500000273117635, -19.73931689729374384 ) ) ;
#6161 = CARTESIAN_POINT ( 'NONE',  ( 26.29305231718579350, 56.80000000000000426, 19.10302069950537529 ) ) ;
#6162 = CARTESIAN_POINT ( 'NONE',  ( 10.04305231718578817, 61.90000000546237402, -30.90933677959249337 ) ) ;
#6163 = PRODUCT_DEFINITION ( 'UNKNOWN', '', #13174, #6504 ) ;
#6164 = CARTESIAN_POINT ( 'NONE',  ( -1.778240108872766143E-15, 2.000000005462374997, -32.49999999999999289 ) ) ;
#6165 = CARTESIAN_POINT ( 'NONE',  ( 26.02091320914876960, 60.26263916574269786, 14.97647472619900455 ) ) ;
#6166 = CARTESIAN_POINT ( 'NONE',  ( 26.29305231718579350, 49.30000000546237970, 19.10302069950537529 ) ) ;
#6167 = CARTESIAN_POINT ( 'NONE',  ( -32.50000000000000000, 79.25000000273118417, 0.000000000000000000 ) ) ;
#6168 = LINE ( 'NONE', #16819, #1348 ) ;
#6169 = AXIS2_PLACEMENT_3D ( 'NONE', #11647, #32574, #17149 ) ;
#6170 = CARTESIAN_POINT ( 'NONE',  ( -26.07999730980490583, 25.46354166666666430, -6.988114217767815717 ) ) ;
#6171 = VECTOR ( 'NONE', #16704, 1000.000000000000114 ) ;
#6172 = CARTESIAN_POINT ( 'NONE',  ( 20.75514604977248467, 74.42500000273119554, -28.56700777964554305 ) ) ;
#6173 = CARTESIAN_POINT ( 'NONE',  ( 26.00068869287340334, 30.19010416666665719, -15.01150461594642316 ) ) ;
#6174 = DIRECTION ( 'NONE',  ( 0.000000000000000000, 0.000000000000000000, -1.000000000000000000 ) ) ;
#6175 = ORIENTED_EDGE ( 'NONE', *, *, #30303, .T. ) ;
#6176 = CARTESIAN_POINT ( 'NONE',  ( -28.00173670424549499, 47.52642333425731636, -7.543491769121417612 ) ) ;
#6177 = CARTESIAN_POINT ( 'NONE',  ( 32.50000000000000000, 7.600000005462379526, -10.55989012756945833 ) ) ;
#6178 = CARTESIAN_POINT ( 'NONE',  ( 28.01184896238290278, 61.27083333333332860, -7.505752307973347470 ) ) ;
#6179 = CARTESIAN_POINT ( 'NONE',  ( -10.04305231718578462, 46.90000000546238113, 30.90933677959249337 ) ) ;
#6180 = CARTESIAN_POINT ( 'NONE',  ( 27.16883889988623935, 46.57500000273117990, -19.73931689729374384 ) ) ;
#6181 = CARTESIAN_POINT ( 'NONE',  ( -20.08610463437157989, 48.20000000546237828, -27.64615127144129758 ) ) ;
#6182 = CARTESIAN_POINT ( 'NONE',  ( 13.91746824999999887, 78.37500000273116996, -1.704398294459741270E-15 ) ) ;
#6183 = CARTESIAN_POINT ( 'NONE',  ( -33.58253175000000113, 35.12500000273119127, 0.000000000000000000 ) ) ;
#6184 = CARTESIAN_POINT ( 'NONE',  ( 24.50000000000000000, 12.00000000000001066, 0.000000000000000000 ) ) ;
#6185 = CARTESIAN_POINT ( 'NONE',  ( 27.16883889988624290, 62.17500000273118133, 19.73931689729373673 ) ) ;
#6186 = CARTESIAN_POINT ( 'NONE',  ( 0.000000000000000000, 0.000000000000000000, 0.000000000000000000 ) ) ;
#6187 = CARTESIAN_POINT ( 'NONE',  ( -32.50000000000000000, 38.09999999999999432, 10.55989012756946366 ) ) ;
#6188 = CARTESIAN_POINT ( 'NONE',  ( 1.507698388325705758E-15, 11.12499999726881761, -24.62258325217400312 ) ) ;
#6189 = CARTESIAN_POINT ( 'NONE',  ( -27.16883889988624290, 3.175000002731187543, -19.73931689729374028 ) ) ;
#6190 = AXIS2_PLACEMENT_3D ( 'NONE', #32901, #9400, #19883 ) ;
#6191 = CARTESIAN_POINT ( 'NONE',  ( 32.50000000000000000, 13.09999999999999432, -10.55989012756945833 ) ) ;
#6192 = CARTESIAN_POINT ( 'NONE',  ( 8.601468415847516980, 78.67500000273119554, -11.83890561707634603 ) ) ;
#6193 = CARTESIAN_POINT ( 'NONE',  ( 33.58253175000000823, 76.27500000273118985, 10.91162601494192685 ) ) ;
#6194 = CARTESIAN_POINT ( 'NONE',  ( -15.14183272437242067, 4.699999999999996625, -20.84094480462497856 ) ) ;
#6195 = AXIS2_PLACEMENT_3D ( 'NONE', #6607, #11753, #9516 ) ;
#6196 = CARTESIAN_POINT ( 'NONE',  ( 20.75514604977248467, 66.67500000273119554, -28.56700777964554305 ) ) ;
#6197 = ORIENTED_EDGE ( 'NONE', *, *, #27503, .F. ) ;
#6198 = CARTESIAN_POINT ( 'NONE',  ( 15.14183272437241889, 3.449999994537620296, 20.84094480462498211 ) ) ;
#6199 = CARTESIAN_POINT ( 'NONE',  ( 26.07999730980490227, 64.99479166666665719, 6.988114217767821046 ) ) ;
#6200 = DIRECTION ( 'NONE',  ( 0.000000000000000000, 1.000000000000000000, 0.000000000000000000 ) ) ;
#6201 = CARTESIAN_POINT ( 'NONE',  ( 33.58253175000000113, 46.22500000273119269, -10.91162601494193751 ) ) ;
#6202 = CARTESIAN_POINT ( 'NONE',  ( 27.16883889988623935, 10.57500000273119056, -19.73931689729374384 ) ) ;
#6203 = CARTESIAN_POINT ( 'NONE',  ( -33.58253175000000113, 63.47500000273117848, 10.91162601494193929 ) ) ;
#6204 = CARTESIAN_POINT ( 'NONE',  ( -13.97622843553588901, 45.37239583333332860, 24.20753774853756823 ) ) ;
#6205 = CARTESIAN_POINT ( 'NONE',  ( 30.02300923189239867, 38.78944416759064495, 0.04044903254992252006 ) ) ;
#6206 = CARTESIAN_POINT ( 'NONE',  ( -28.02196122052058413, 24.02565999907602290, -7.468012846824272799 ) ) ;
#6207 = CARTESIAN_POINT ( 'NONE',  ( 26.29305231718578995, 67.70000000546237118, -19.10302069950538240 ) ) ;
#6208 = CARTESIAN_POINT ( 'NONE',  ( -4.300734207923759378, 78.47500000273116427, -13.23629886949340495 ) ) ;
#6209 = CARTESIAN_POINT ( 'NONE',  ( 24.18731323226221974, 59.68972249907602645, -14.01125832528328985 ) ) ;
#6210 = CARTESIAN_POINT ( 'NONE',  ( 23.41746825000000243, 16.72499999726881725, -7.608796670333727974 ) ) ;
#6211 = EDGE_CURVE ( 'NONE', #19609, #9681, #19401, .T. ) ;
#6212 = CARTESIAN_POINT ( 'NONE',  ( -3.880418787951099180, 16.55125428154684286, -24.50000000000001421 ) ) ;
#6213 = ORIENTED_EDGE ( 'NONE', *, *, #15322, .T. ) ;
#6214 = CARTESIAN_POINT ( 'NONE',  ( -33.58253175000000113, 49.37500000273119127, 0.000000000000000000 ) ) ;
#6215 = CARTESIAN_POINT ( 'NONE',  ( 1.507698388325705758E-15, 1.624999997268827823, -24.62258325217400312 ) ) ;
#6216 = CARTESIAN_POINT ( 'NONE',  ( -13.94119854578936923, 54.83111083425730214, -24.22776226481241224 ) ) ;
#6217 = CARTESIAN_POINT ( 'NONE',  ( 32.50000000000000711, 31.40000000546238823, 10.55989012756945122 ) ) ;
#6218 = VERTEX_POINT ( 'NONE', #20507 ) ;
#6219 = CARTESIAN_POINT ( 'NONE',  ( 33.58253175000000113, 18.12500000273119127, -4.112674001490185761E-15 ) ) ;
#6220 = AXIS2_PLACEMENT_3D ( 'NONE', #24367, #19056, #14067 ) ;
#6221 = EDGE_CURVE ( 'NONE', #15956, #21689, #28417, .T. ) ;
#6222 = CARTESIAN_POINT ( 'NONE',  ( -15.01150461594595775, 28.18489583333332860, 26.00068869287368756 ) ) ;
#6223 = ORIENTED_EDGE ( 'NONE', *, *, #19302, .T. ) ;
#6224 = VERTEX_POINT ( 'NONE', #5044 ) ;
#6225 = CARTESIAN_POINT ( 'NONE',  ( -32.50000000000000000, 48.60000000546235555, 10.55989012756946366 ) ) ;
#6226 = CARTESIAN_POINT ( 'NONE',  ( -20.75514604977248112, 53.42500000273117422, 28.56700777964554661 ) ) ;
#6227 = CARTESIAN_POINT ( 'NONE',  ( -7.505752307972844761, 62.41666666666666430, 28.01184896238304134 ) ) ;
#6228 = CARTESIAN_POINT ( 'NONE',  ( 6.277390505771533514E-15, 9.000000005462364783, 34.17252228774368916 ) ) ;
#6229 = CARTESIAN_POINT ( 'NONE',  ( 3.880418787951134707, 15.30125427608446742, 24.50000000000000000 ) ) ;
#6230 = CARTESIAN_POINT ( 'NONE',  ( -4.523095164977117273E-15, 14.62499999726882649, 24.62258325217400312 ) ) ;
#6231 = CARTESIAN_POINT ( 'NONE',  ( -32.50000000000000000, 57.89999999999999858, -10.55989012756945478 ) ) ;
#6232 = CARTESIAN_POINT ( 'NONE',  ( -2.162160676586881955E-15, 22.87500000273118062, -35.31076352940723240 ) ) ;
#6233 = CARTESIAN_POINT ( 'NONE',  ( -26.09010956794245217, 20.58815999907601935, -6.950374756619243755 ) ) ;
#6234 = CARTESIAN_POINT ( 'NONE',  ( -13.91746824999999532, 76.77500000273117564, -4.522059556121115875 ) ) ;
#6235 = CARTESIAN_POINT ( 'NONE',  ( 19.82091636218621389, 16.19999999999999218, -14.40073868116559197 ) ) ;
#6236 = CARTESIAN_POINT ( 'NONE',  ( 5.779280353836490358E-15, 14.50000000000000178, 32.49999999999999289 ) ) ;
#6237 = CARTESIAN_POINT ( 'NONE',  ( -10.04305231718579172, 9.599999999999983658, -30.90933677959248982 ) ) ;
#6238 = ORIENTED_EDGE ( 'NONE', *, *, #25807, .T. ) ;
#6239 = CARTESIAN_POINT ( 'NONE',  ( -14.47279130897151589, 5.824999997268811569, -19.92008829642072598 ) ) ;
#6240 = CARTESIAN_POINT ( 'NONE',  ( 13.91746825000000065, 75.77500000273120406, 4.522059556121114987 ) ) ;
#6241 = CARTESIAN_POINT ( 'NONE',  ( 6.988114217768294445, 44.94270833333332860, 26.07999730980477437 ) ) ;
#6242 = CARTESIAN_POINT ( 'NONE',  ( -20.75514604977248823, 18.82500000273119767, -28.56700777964554305 ) ) ;
#6243 = CARTESIAN_POINT ( 'NONE',  ( -10.37757302488624411, 68.72500000273116427, -31.93888565452638417 ) ) ;
#6244 = CARTESIAN_POINT ( 'NONE',  ( 20.75514604977248467, 30.67500000273119909, -28.56700777964554305 ) ) ;
#6245 = AXIS2_PLACEMENT_3D ( 'NONE', #6662, #25544, #4088 ) ;
#6246 = CARTESIAN_POINT ( 'NONE',  ( 27.16883889988623935, 18.57500000273119767, -19.73931689729374384 ) ) ;
#6247 = CARTESIAN_POINT ( 'NONE',  ( 33.58253175000000113, 10.37500000273117173, -4.112674001490185761E-15 ) ) ;
#6248 = CARTESIAN_POINT ( 'NONE',  ( 19.11951029504763611, 62.42225666759065206, -19.06425588902591173 ) ) ;
#6249 = CIRCLE ( 'NONE', #27606, 30.00000000000000000 ) ;
#6250 = CARTESIAN_POINT ( 'NONE',  ( 28.01184896238290278, 57.83333333333333570, -7.505752307973347470 ) ) ;
#6251 = CARTESIAN_POINT ( 'NONE',  ( 3.735172737399427541E-15, 80.00000000000001421, 30.50000000000000000 ) ) ;
#6252 = CARTESIAN_POINT ( 'NONE',  ( -4.300734207923759378, 74.97500000273119269, -13.23629886949340495 ) ) ;
#6253 = CARTESIAN_POINT ( 'NONE',  ( -32.50000000000000000, 50.09999999999998721, 10.55989012756946366 ) ) ;
#6254 = CARTESIAN_POINT ( 'NONE',  ( 8.891200544363830713E-16, 79.75000000546236834, -15.00000000000000000 ) ) ;
#6255 = CARTESIAN_POINT ( 'NONE',  ( 20.75514604977249178, 53.82500000273119412, 28.56700777964553950 ) ) ;
#6256 = CARTESIAN_POINT ( 'NONE',  ( -4.523095164977116484E-15, 12.62499999726879985, 24.62258325217400312 ) ) ;
#6257 = ORIENTED_EDGE ( 'NONE', *, *, #9555, .F. ) ;
#6258 = CARTESIAN_POINT ( 'NONE',  ( -10.37757302488623701, 69.77500000273118985, 31.93888565452638417 ) ) ;
#6259 = CARTESIAN_POINT ( 'NONE',  ( 0.000000000000000000, 0.000000000000000000, 0.000000000000000000 ) ) ;
#6260 = CARTESIAN_POINT ( 'NONE',  ( 7.236395654485755280, 4.224999997268802154, 22.27133577429736988 ) ) ;
#6261 = CARTESIAN_POINT ( 'NONE',  ( -24.22776226481240514, 26.47173583425730925, 13.94119854578937812 ) ) ;
#6262 =( BOUNDED_CURVE ( )  B_SPLINE_CURVE ( 2, ( #23922, #558, #32128, #24090, #7957, #19107, #18444, #8125, #13625, #8456, #5890, #16204, #31794 ),
 .UNSPECIFIED., .F., .T. ) 
 B_SPLINE_CURVE_WITH_KNOTS ( ( 3, 2, 2, 2, 2, 2, 3 ),
 ( 0.3525641025641025883, 0.3538461538461538658, 0.3564102564102564208, 0.3589743589743589758, 0.3615384615384615308, 0.3641025641025640858, 0.3653846153846153633 ),
 .UNSPECIFIED. ) 
 CURVE ( )  GEOMETRIC_REPRESENTATION_ITEM ( )  RATIONAL_B_SPLINE_CURVE ( ( 0.9755282581475768211, 0.9755282581475772652, 1.000000000000000000, 0.9510565162951535312, 1.000000000000000000, 0.9510565162951535312, 1.000000000000000000, 0.9510565162951535312, 1.000000000000000000, 0.9510565162951535312, 1.000000000000000000, 0.9755282581475768211, 0.9755282581475768211 ) ) 
 REPRESENTATION_ITEM ( '' )  );
#6263 = ORIENTED_EDGE ( 'NONE', *, *, #33483, .F. ) ;
#6264 = CARTESIAN_POINT ( 'NONE',  ( 27.16883889988624290, 33.92500000273117422, 19.73931689729373673 ) ) ;
#6265 = CARTESIAN_POINT ( 'NONE',  ( 6.001560367445586717E-15, 1.500000000000005995, 24.50000000000000000 ) ) ;
#6266 = VERTEX_POINT ( 'NONE', #25981 ) ;
#6268 = CARTESIAN_POINT ( 'NONE',  ( 20.50609665440969565, 50.67187500000000000, -20.50609665441004736 ) ) ;
#6267 =( BOUNDED_CURVE ( )  B_SPLINE_CURVE ( 2, ( #22391, #19993, #25483, #12086, #1962, #14671, #24790, #11749, #30441, #32674, #1269, #32840, #17080 ),
 .UNSPECIFIED., .F., .T. ) 
 B_SPLINE_CURVE_WITH_KNOTS ( ( 3, 2, 2, 2, 2, 2, 3 ),
 ( 0.5500000000000000444, 0.5600000000000000533, 0.5799999999999999600, 0.5999999999999999778, 0.6199999999999999956, 0.6400000000000000133, 0.6500000000000000222 ),
 .UNSPECIFIED. ) 
 CURVE ( )  GEOMETRIC_REPRESENTATION_ITEM ( )  RATIONAL_B_SPLINE_CURVE ( ( 0.9755282581475768211, 0.9755282581475768211, 1.000000000000000000, 0.9510565162951535312, 1.000000000000000000, 0.9510565162951535312, 1.000000000000000000, 0.9510565162951535312, 1.000000000000000000, 0.9510565162951535312, 1.000000000000000000, 0.9755282581475768211, 0.9755282581475768211 ) ) 
 REPRESENTATION_ITEM ( '' )  );
#6269 = CARTESIAN_POINT ( 'NONE',  ( -33.58253175000000113, 59.37500000273118417, 0.000000000000000000 ) ) ;
#6270 = CARTESIAN_POINT ( 'NONE',  ( 2.067204126564591252E-14, 4.499999999999996447, -24.50000000000000000 ) ) ;
#6271 = CARTESIAN_POINT ( 'NONE',  ( -33.58253175000000113, 71.12500000273119838, 0.000000000000000000 ) ) ;
#6272 = CARTESIAN_POINT ( 'NONE',  ( -15.01150461594642138, 29.33072916666665719, -26.00068869287340334 ) ) ;
#6273 = CARTESIAN_POINT ( 'NONE',  ( 19.82091636218621389, 4.200000000000009059, -14.40073868116559197 ) ) ;
#6274 = CARTESIAN_POINT ( 'NONE',  ( -33.58253175000000113, 3.475000002731185589, 10.91162601494193929 ) ) ;
#6275 = EDGE_CURVE ( 'NONE', #29257, #31380, #12941, .T. ) ;
#6276 = CARTESIAN_POINT ( 'NONE',  ( 6.486482029760649416E-15, 19.62500000273116996, 35.31076352940723240 ) ) ;
#6277 = CARTESIAN_POINT ( 'NONE',  ( -13.91746824999999532, 74.77500000273117564, -4.522059556121115875 ) ) ;
#6278 = CARTESIAN_POINT ( 'NONE',  ( -30.02300923189239867, 47.94493083240935505, 0.04044903255044988294 ) ) ;
#6279 = CARTESIAN_POINT ( 'NONE',  ( 9.270509831248423538, 79.30000000000003979, -12.75976212528059861 ) ) ;
#6280 = CARTESIAN_POINT ( 'NONE',  ( -28.01184896238290278, 52.67708333333333570, 7.505752307973363457 ) ) ;
#6281 = CARTESIAN_POINT ( 'NONE',  ( -24.50000000000000711, 16.84999999453763309, 7.960532557706201828 ) ) ;
#6282 = CARTESIAN_POINT ( 'NONE',  ( 5.147494310547426899, 71.44874571845316780, -32.50000000000000000 ) ) ;
#6283 = CARTESIAN_POINT ( 'NONE',  ( -6.988114217767819270, 14.29166666666666430, 26.07999730980490583 ) ) ;
#6284 = CARTESIAN_POINT ( 'NONE',  ( -10.37757302488624411, 42.72500000273119269, -31.93888565452638417 ) ) ;
#6285 = CARTESIAN_POINT ( 'NONE',  ( -13.91746824999999887, 74.87500000273116996, 0.000000000000000000 ) ) ;
#6286 = CARTESIAN_POINT ( 'NONE',  ( 33.58253175000000113, 52.37500000273119838, -4.112674001490185761E-15 ) ) ;
#6287 = CARTESIAN_POINT ( 'NONE',  ( 33.58253175000000823, 30.27500000273118275, 10.91162601494192685 ) ) ;
#6288 = CARTESIAN_POINT ( 'NONE',  ( 19.42321331973577969, 16.99999999999997868, 13.32227027544421638 ) ) ;
#6289 = CARTESIAN_POINT ( 'NONE',  ( -13.97622843553588901, 24.74739583333332860, 24.20753774853756823 ) ) ;
#6290 = CARTESIAN_POINT ( 'NONE',  ( 24.50000000000000000, 18.00000000000001421, 0.000000000000000000 ) ) ;
#6291 = CARTESIAN_POINT ( 'NONE',  ( -9.270509831248423538, 75.69999999999998863, -12.75976212528059861 ) ) ;
#6292 = CARTESIAN_POINT ( 'NONE',  ( -10.04305231718579172, 67.59999999999998010, -30.90933677959248982 ) ) ;
#6293 = CARTESIAN_POINT ( 'NONE',  ( -27.16883889988624290, 6.925000002731204418, -19.73931689729374028 ) ) ;
#6294 = CARTESIAN_POINT ( 'NONE',  ( 23.41746824999999887, 6.724999997268811924, -7.608796670333727974 ) ) ;
#6295 = CARTESIAN_POINT ( 'NONE',  ( -7.468012846824272799, 23.16628499907601579, 28.02196122052058413 ) ) ;
#6296 = CARTESIAN_POINT ( 'NONE',  ( -24.50000000000000711, 10.84999999453761887, 7.960532557706201828 ) ) ;
#6297 = CARTESIAN_POINT ( 'NONE',  ( -14.01125832528328985, 27.89284749907601935, -24.18731323226223040 ) ) ;
#6298 = CARTESIAN_POINT ( 'NONE',  ( -12.13525491562420910, 76.45000000546237118, 8.816778784387098611 ) ) ;
#6299 = CARTESIAN_POINT ( 'NONE',  ( 33.58253175000000113, 22.22500000273117493, -10.91162601494193574 ) ) ;
#6300 = CARTESIAN_POINT ( 'NONE',  ( -4.523095164977116484E-15, 6.624999997268815832, 24.62258325217400312 ) ) ;
#6301 = CARTESIAN_POINT ( 'NONE',  ( 13.97622843553633665, 55.11197916666664298, 24.20753774853730889 ) ) ;
#6302 = ORIENTED_EDGE ( 'NONE', *, *, #8037, .F. ) ;
#6303 = CARTESIAN_POINT ( 'NONE',  ( -33.58253175000000113, 57.12500000273116996, 0.000000000000000000 ) ) ;
#6304 = CARTESIAN_POINT ( 'NONE',  ( 10.37757302488624767, 27.97500000273118914, 31.93888565452638417 ) ) ;
#6305 = ORIENTED_EDGE ( 'NONE', *, *, #26712, .F. ) ;
#6306 = CARTESIAN_POINT ( 'NONE',  ( 20.50609665440969565, 23.17187499999999289, -20.50609665441004736 ) ) ;
#6307 = CARTESIAN_POINT ( 'NONE',  ( 20.47846945139902530, 22.03163166759064495, 20.53372385742071771 ) ) ;
#6308 = CARTESIAN_POINT ( 'NONE',  ( 5.147494310547426899, 39.44874571845314648, -32.50000000000000000 ) ) ;
#6309 = CARTESIAN_POINT ( 'NONE',  ( -19.82091636218621389, 14.94999999453763806, 14.40073868116558842 ) ) ;
#6310 = CARTESIAN_POINT ( 'NONE',  ( -23.41746824999999887, 3.624999997268813168, -2.867812753649727150E-15 ) ) ;
#6311 = CARTESIAN_POINT ( 'NONE',  ( 27.16883889988623935, 28.57500000273119412, -19.73931689729374384 ) ) ;
#6312 = MECHANICAL_DESIGN_GEOMETRIC_PRESENTATION_REPRESENTATION (  '', ( #28758 ), #28244 ) ;
#6313 = CARTESIAN_POINT ( 'NONE',  ( 26.29305231718579350, 33.30000000546237970, 19.10302069950537529 ) ) ;
#6314 = EDGE_CURVE ( 'NONE', #13788, #969, #1633, .T. ) ;
#6315 = CARTESIAN_POINT ( 'NONE',  ( -32.50000000000000000, 74.00000000000001421, 0.000000000000000000 ) ) ;
#6316 = LINE ( 'NONE', #19698, #10504 ) ;
#6317 = CARTESIAN_POINT ( 'NONE',  ( -1.778240108872766143E-15, 38.00000000546237544, -32.49999999999999289 ) ) ;
#6318 = CARTESIAN_POINT ( 'NONE',  ( 7.543491769121427382, 58.69829833425730925, -28.00173670424548433 ) ) ;
#6319 = CARTESIAN_POINT ( 'NONE',  ( -33.58253175000000113, 39.27500000273118275, -10.91162601494193218 ) ) ;
#6320 = CARTESIAN_POINT ( 'NONE',  ( 15.01150461594596486, 19.59114583333332504, -26.00068869287367690 ) ) ;
#6321 =( LENGTH_UNIT ( ) NAMED_UNIT ( * ) SI_UNIT ( .MILLI., .METRE. ) );
#6322 = EDGE_CURVE ( 'NONE', #28763, #17393, #3154, .T. ) ;
#6323 = CARTESIAN_POINT ( 'NONE',  ( -14.47279130897152122, 10.42499999726881299, 19.92008829642072243 ) ) ;
#6324 = CARTESIAN_POINT ( 'NONE',  ( -10.04305231718578462, 12.39999999999999503, 30.90933677959249337 ) ) ;
#6325 = CARTESIAN_POINT ( 'NONE',  ( 1.577395562988744260E-15, 12.50000000000001243, -25.76082449383753925 ) ) ;
#6326 = CARTESIAN_POINT ( 'NONE',  ( -27.95245687107223986, 44.50743083240935505, 0.04044903255043252877 ) ) ;
#6327 = CARTESIAN_POINT ( 'NONE',  ( -10.37757302488623701, 63.52500000273120406, 31.93888565452638417 ) ) ;
#6328 = CARTESIAN_POINT ( 'NONE',  ( -33.58253175000000113, 45.37500000273120548, 0.000000000000000000 ) ) ;
#6329 = CARTESIAN_POINT ( 'NONE',  ( -23.41746824999999887, 9.624999997268817609, -2.867812753649727150E-15 ) ) ;
#6330 = CARTESIAN_POINT ( 'NONE',  ( 24.50000000000000000, 3.649999994537613812, 7.960532557706212486 ) ) ;
#6331 = CARTESIAN_POINT ( 'NONE',  ( 6.486482029760649416E-15, 5.625000002731175286, 35.31076352940723240 ) ) ;
#6332 = CARTESIAN_POINT ( 'NONE',  ( -6.950374756619716266, 41.22434000092397355, -26.09010956794232428 ) ) ;
#6333 = CARTESIAN_POINT ( 'NONE',  ( 19.90391271886689495, 16.99999999999998579, -12.36117064040718461 ) ) ;
#6334 = DIRECTION ( 'NONE',  ( -0.000000000000000000, -1.000000000000000000, -0.000000000000000000 ) ) ;
#6335 = CARTESIAN_POINT ( 'NONE',  ( -27.16883889988624290, 28.92500000273119554, -19.73931689729374028 ) ) ;
#6336 = CARTESIAN_POINT ( 'NONE',  ( 10.18398033115918189, -70.48295565631028126, 1.443142760386851780E-15 ) ) ;
#6337 = CARTESIAN_POINT ( 'NONE',  ( 0.000000000000000000, 16.99999999999998579, 0.000000000000000000 ) ) ;
#6338 = CARTESIAN_POINT ( 'NONE',  ( 5.147494310547481966, 61.44874571845315359, -32.49999999999998579 ) ) ;
#6339 = CARTESIAN_POINT ( 'NONE',  ( 0.04044903255045854962, 57.39805583240935505, 30.02300923189239867 ) ) ;
#6340 = CARTESIAN_POINT ( 'NONE',  ( -32.50000000000000000, 46.50000000546238255, 0.000000000000000000 ) ) ;
#6341 = PRESENTATION_STYLE_ASSIGNMENT (( #8406 ) ) ;
#6342 = CARTESIAN_POINT ( 'NONE',  ( -26.07999730980490583, 28.90104166666666785, -6.988114217767815717 ) ) ;
#6343 = EDGE_LOOP ( 'NONE', ( #17736, #26529, #28727, #8040 ) ) ;
#6344 = CARTESIAN_POINT ( 'NONE',  ( -27.16883889988623935, 75.32500000273118701, 19.73931689729374739 ) ) ;
#6345 = CARTESIAN_POINT ( 'NONE',  ( -15.01150461594595775, 35.05989583333332860, 26.00068869287368756 ) ) ;
#6346 = CARTESIAN_POINT ( 'NONE',  ( -10.11607355459419644, -70.99969134886156041, 0.000000000000000000 ) ) ;
#6347 = ORIENTED_EDGE ( 'NONE', *, *, #29971, .T. ) ;
#6348 = CARTESIAN_POINT ( 'NONE',  ( -20.53372385742071771, 50.39100666759063785, 20.47846945139902530 ) ) ;
#6349 = AXIS2_PLACEMENT_3D ( 'NONE', #10680, #31603, #30030 ) ;
#6350 = CARTESIAN_POINT ( 'NONE',  ( -10.04305231718579172, 12.10000000546239463, -30.90933677959248982 ) ) ;
#6351 = CARTESIAN_POINT ( 'NONE',  ( 20.50609665440969565, 57.54687500000000000, -20.50609665441004736 ) ) ;
#6352 = CARTESIAN_POINT ( 'NONE',  ( -20.08610463437157989, 46.20000000546237828, -27.64615127144129758 ) ) ;
#6353 = CARTESIAN_POINT ( 'NONE',  ( -33.58253175000000113, 47.37500000273120548, 0.000000000000000000 ) ) ;
#6354 = CARTESIAN_POINT ( 'NONE',  ( 26.29305231718579350, 49.30000000546236549, 19.10302069950537529 ) ) ;
#6355 = CARTESIAN_POINT ( 'NONE',  ( -8.601468415847518756, 73.07500000273118701, -11.83890561707634781 ) ) ;
#6356 = CARTESIAN_POINT ( 'NONE',  ( -20.75514604977248823, 28.82500000273116569, -28.56700777964554305 ) ) ;
#6357 = CARTESIAN_POINT ( 'NONE',  ( 32.50000000000000000, 77.60000000546237686, -10.55989012756945833 ) ) ;
#6358 = CARTESIAN_POINT ( 'NONE',  ( 6.486482029760649416E-15, 61.87500000273117706, 35.31076352940723240 ) ) ;
#6359 = CARTESIAN_POINT ( 'NONE',  ( 32.50000000000000000, 35.10000000000000142, -10.55989012756945833 ) ) ;
#6360 = CARTESIAN_POINT ( 'NONE',  ( 32.50000000000000000, 35.10000000000000142, -10.55989012756945833 ) ) ;
#6361 = CARTESIAN_POINT ( 'NONE',  ( 14.47279130897151589, 14.32499999726880624, 19.92008829642072953 ) ) ;
#6362 =( BOUNDED_CURVE ( )  B_SPLINE_CURVE ( 2, ( #27434, #3925, #14399, #25370, #25196, #12149, #30504, #14232, #9581, #3760, #1506, #1849, #22293 ),
 .UNSPECIFIED., .F., .T. ) 
 B_SPLINE_CURVE_WITH_KNOTS ( ( 3, 2, 2, 2, 2, 2, 3 ),
 ( 0.4807692307692307820, 0.4820512820512820595, 0.4846153846153846145, 0.4871794871794871695, 0.4897435897435897245, 0.4923076923076923350, 0.4935897435897436125 ),
 .UNSPECIFIED. ) 
 CURVE ( )  GEOMETRIC_REPRESENTATION_ITEM ( )  RATIONAL_B_SPLINE_CURVE ( ( 0.9755282581475768211, 0.9755282581475768211, 1.000000000000000000, 0.9510565162951535312, 1.000000000000000000, 0.9510565162951535312, 1.000000000000000000, 0.9510565162951535312, 1.000000000000000000, 0.9510565162951535312, 1.000000000000000000, 0.9755282581475768211, 0.9755282581475768211 ) ) 
 REPRESENTATION_ITEM ( '' )  );
#6363 = CARTESIAN_POINT ( 'NONE',  ( -27.16883889988623935, 7.575000002731202997, 19.73931689729374739 ) ) ;
#6364 = CYLINDRICAL_SURFACE ( 'NONE', #17306, 32.50000000000000000 ) ;
#6365 = CARTESIAN_POINT ( 'NONE',  ( 13.91746825000000065, 80.27500000273120406, 4.522059556121115875 ) ) ;
#6366 = CARTESIAN_POINT ( 'NONE',  ( -33.58253175000000113, 65.27500000273117564, -10.91162601494193041 ) ) ;
#6367 = CARTESIAN_POINT ( 'NONE',  ( 19.82091636218621034, 3.549999994537617276, 14.40073868116559730 ) ) ;
#6368 = CARTESIAN_POINT ( 'NONE',  ( -27.16883889988623935, 61.57500000273117990, 19.73931689729374739 ) ) ;
#6369 = VERTEX_POINT ( 'NONE', #18613 ) ;
#6370 = CARTESIAN_POINT ( 'NONE',  ( 24.50000000000000000, 1.749999994537621006, 0.000000000000000000 ) ) ;
#6371 = CARTESIAN_POINT ( 'NONE',  ( 24.20753774853731244, 64.56510416666667140, -13.97622843553632599 ) ) ;
#6372 = CARTESIAN_POINT ( 'NONE',  ( 2.375766604868046361, 74.55125428154683220, 14.99999999999999822 ) ) ;
#6373 = CARTESIAN_POINT ( 'NONE',  ( 27.16883889988624290, 49.92500000273118843, 19.73931689729373673 ) ) ;
#6374 = CARTESIAN_POINT ( 'NONE',  ( -10.37757302488624411, 12.97500000273120513, -31.93888565452638417 ) ) ;
#6375 = CARTESIAN_POINT ( 'NONE',  ( -27.16883889988623935, 63.57500000273117990, 19.73931689729374739 ) ) ;
#6376 = CARTESIAN_POINT ( 'NONE',  ( -19.09188309203694445, 49.81249999999999289, -19.09188309203661049 ) ) ;
#6377 = CARTESIAN_POINT ( 'NONE',  ( 28.02196122052045268, 35.20871500092396644, -7.468012846824774620 ) ) ;
#6378 = CARTESIAN_POINT ( 'NONE',  ( -20.53372385742107653, 27.74961833240935505, -20.47846945139867003 ) ) ;
#6379 = CARTESIAN_POINT ( 'NONE',  ( -10.04305231718579172, 66.10000000546239107, -30.90933677959248982 ) ) ;
#6380 = EDGE_CURVE ( 'NONE', #7743, #14916, #15865, .T. ) ;
#6381 = FACE_BOUND ( 'NONE', #19606, .T. ) ;
#6382 = CARTESIAN_POINT ( 'NONE',  ( 6.950374756619257965, 52.38503499907601224, -26.09010956794244507 ) ) ;
#6383 = DIRECTION ( 'NONE',  ( -0.8660254037844385966, 0.000000000000000000, 0.5000000000000000000 ) ) ;
#6384 = CARTESIAN_POINT ( 'NONE',  ( -19.82091636218621034, 16.80000000000000782, -14.40073868116559552 ) ) ;
#6385 = ORIENTED_EDGE ( 'NONE', *, *, #30392, .F. ) ;
#6386 = CARTESIAN_POINT ( 'NONE',  ( -33.58253175000000113, 43.47500000273117138, 10.91162601494193929 ) ) ;
#6387 = DIRECTION ( 'NONE',  ( 0.000000000000000000, -1.000000000000000000, 0.000000000000000000 ) ) ;
#6388 = CARTESIAN_POINT ( 'NONE',  ( 6.277390505771533514E-15, 27.00000000546237899, 34.17252228774368916 ) ) ;
#6389 = ORIENTED_EDGE ( 'NONE', *, *, #19964, .T. ) ;
#6390 = CARTESIAN_POINT ( 'NONE',  ( -26.00068869287368756, 32.48177083333332860, -15.01150461594595775 ) ) ;
#6391 = VERTEX_POINT ( 'NONE', #3318 ) ;
#6392 = EDGE_LOOP ( 'NONE', ( #9816, #1930, #20649, #13067 ) ) ;
#6393 = CARTESIAN_POINT ( 'NONE',  ( 24.49999999999999645, -22.99999999999999645, 3.000384657911015074E-15 ) ) ;
#6394 = CARTESIAN_POINT ( 'NONE',  ( 20.75514604977248467, 56.42500000273120264, -28.56700777964554305 ) ) ;
#6395 = CARTESIAN_POINT ( 'NONE',  ( 30.02300923189239512, 57.97656249999997868, -2.619432448724977703E-13 ) ) ;
#6396 = CARTESIAN_POINT ( 'NONE',  ( -32.50000000000000000, 12.50000000546236478, 0.000000000000000000 ) ) ;
#6397 = DIRECTION ( 'NONE',  ( 0.000000000000000000, 0.000000000000000000, -1.000000000000000000 ) ) ;
#6398 = CIRCLE ( 'NONE', #1465, 30.00000000000000711 ) ;
#6399 = CARTESIAN_POINT ( 'NONE',  ( -23.41746825000000243, 12.22499999726881370, 7.608796670333725309 ) ) ;
#6400 =( BOUNDED_SURFACE ( )  B_SPLINE_SURFACE ( 3, 2, ( 
 ( #33481, #14619, #27656, #9983, #19937, #28341, #22502, #27829, #1556, #4826, #32953, #20114, #25251, #9455, #14787, #2250, #30559, #2080, #15306, #23195, #33657, #30732, #6885, #27998, #4485, #25427, #12382, #22851, #7225, #17711, #17366, #10155, #1726, #12206, #22677, #33128, #31749, #2603, #25933, #24045, #26613, #514, #23705, #29176, #15655, #13064, #2766, #11000, #10491, #33831, #18055, #8081, #20804, #171, #18566, #3111, #29009, #31248, #2937, #13407, #23876, #10661, #31419, #15822, #346, #4997, #28500, #10830, #10328, #21309, #2427, #18229, #7575, #8241, #15480, #1, #26105, #12895, #28675, #16159, #20968, #5509, #18734, #5681, #13583, #21140, #23370, #7912, #18396, #28842, #13230, #5340, #31581, #26276, #7740, #31080, #15990, #5170, #23540, #26446, #22139, #26939, #16325, #14413, #16988, #24866, #14077, #19564, #6009, #3439, #27110, #1347, #848, #24209, #8410, #32417, #11168, #24536, #8913, #27446, #19396, #21639, #27279, #3772, #14243, #1007, #21804, #6173, #32085, #19230, #16483, #3603, #30011, #6517, #13909, #9082, #11328, #29844, #18898, #16655, #32253, #24700, #8581, #21471, #3938, #682, #32583, #24375, #31917, #21969, #19065, #29504, #29345, #5846, #8746, #26781, #11490, #3272, #1177, #29667, #13740, #6345, #16823, #11658, #17498, #12515, #12164, #14748, #25726, #25560, #2040, #4442, #1519, #20074, #30689, #17162, #22982, #20247, #22462, #14918, #27619, #9592, #7015, #11994, #32913, #25386, #33090, #30517, #27960, #22305, #1863, #9412, #25210, #30346, #6678, #19896, #30865, #1688, #33269, #33441, #9939, #28128, #12340, #30175, #22638, #22810, #9762, #7186, #17667, #4616, #15092, #9243, #20414, #7357, #6847, #17844, #28298, #4785, #17325, #4105, #15264, #11828, #32750, #19730, #14578, #27789, #4274, #25039, #7869, #2386, #20594, #12683, #18190, #31040, #31211, #28631, #20932, #5130, #7535, #15616, #26068, #2561, #7703, #12856, #33795, #18019, #23331, #28465, #20767, #33959, #10453, #4958, #23502, #25890, #13028, #23150, #10289, #31379, #2205, #15438, #33615, #10115, #24607, #32822, #21715, #11399, #11728, #21876, #1081, #22210, #27356, #32657, #8654, #1249, #19798, #9313, #30247, #9152, #16561, #4181, #3677, #6751, #17231, #19139, #19635, #24286, #3841, #19300, #22043, #758, #11561, #30079, #27691, #11239, #27522, #29576, #6077, #32161, #920, #27014, #6422, #16893, #29744, #32326, #14316, #32487, #6585, #4009, #14483, #8989, #24771, #3511, #17061, #24939, #19470, #29919, #13982, #24444, #8817, #1424, #6250, #11902, #22374, #16729, #27185, #14151, #25288, #17745, #19975, #12418, #9842, #14824, #1760, #28205, #1941, #22888, #33345, #25115, #20320, #12240, #30944, #22538, #1590, #7441, #27866, #17925, #30421, #22717, #12068, #28376, #32988, #17574, #33166, #9493, #9669, #33696, #28033, #2115, #25799, #4864, #15345, #4691, #6920, #25465, #4520, #30769, #7259, #15170, #25636, #12588, #17402, #2289, #23058, #20150, #10197, #31117, #12763, #30594, #4348, #7610, #20677, #18091, #33518, #23236, #7090 ),
 ( #10022, #14995, #20495, #28538, #14655, #18603, #5377, #23743, #28710, #2801, #23574, #21176, #13616, #24081, #39, #26649, #18435, #13444, #25971, #207, #28879, #10868, #5208, #26142, #13268, #13101, #20839, #31454, #547, #5545, #18264, #15692, #3144, #11034, #15856, #2464, #8115, #10361, #18767, #2638, #12931, #23407, #31284, #10528, #10695, #5717, #26312, #7947, #18936, #29211, #16195, #31618, #21005, #15519, #31784, #33868, #29042, #16026, #7777, #26481, #21503, #2975, #23911, #31952, #8444, #21342, #383, #8275, #5034, #8777, #6206, #1041, #27143, #8950, #16686, #26813, #11689, #16856, #6039, #14443, #11859, #30043, #881, #24243, #22337, #24899, #32782, #22001, #27481, #13941, #11363, #11521, #9276, #19260, #32119, #16358, #6378, #19098, #32449, #27314, #1385, #3805, #29536, #1208, #22173, #32617, #19428, #29702, #14111, #16518, #3637, #24405, #29878, #3971, #29381, #21839, #17022, #24569, #14276, #3309, #24733, #9114, #19595, #26970, #3471, #6548, #32284, #11200, #5881, #13773, #714, #8616, #21671, #7394, #17879, #9625, #6712, #22843, #25070, #33474, #32946, #17193, #27651, #1551, #19931, #25420, #20450, #20107, #22671, #33650, #9974, #30901, #12374, #9449, #27992, #4649, #12027, #28333, #28163, #30377, #33302, #22496, #17531, #14955, #6878, #17359, #9802, #7049, #4479, #1899, #30210, #20278, #27823, #2072, #4139, #14614, #12548, #4305, #23019, #14780, #25245, #30725, #1720, #7219, #12199, #4819, #33122, #17704, #30553, #15130, #25593, #15298, #25758, #2243, #12717, #23188, #19760, #23871, #28669, #21304, #5503, #339, #28494, #23698, #26607, #10824, #5333, #31744, #26269, #2757, #8235, #10654, #18050, #28835, #18729, #29166, #10484, #13576, #21132, #5674, #16154, #8072, #25926, #23531, #31574, #3105, #4991, #24039, #7567, #15814, #10147, #2595, #18558, #20962, #23363, #13401, #20629, #18389, #31072, #24675, #29002, #7733, #164, #2931, #13223, #15473, #2420, #15983, #31412, #12887, #7905, #20797, #26439, #33824, #10318, #31241, #18223, #5162, #15647, #26098, #13058, #32410, #18891, #11485, #30004, #19557, #9076, #21962, #26776, #14406, #13903, #6509, #16982, #29338, #8905, #508, #14069, #29498, #32248, #10993, #839, #19390, #27439, #3931, #3766, #5840, #16318, #21466, #11161, #3265, #16649, #27103, #6002, #21631, #24530, #21797, #29837, #14237, #24694, #8740, #3595, #31908, #1001, #6339, #11321, #19224, #8403, #13734, #26932, #24203, #16817, #672, #32077, #22134, #32577, #24369, #8575, #27272, #19058, #1171, #16476, #3430, #29661, #6165, #11650, #30509, #25552, #25201, #27780, #4778, #4607, #15084, #17491, #14571, #33082, #9754, #30167, #2032, #33260, #1511, #27953, #6671, #22628, #20065, #25031, #11986, #4435, #12154, #9585, #7008, #1340, #14911, #22455, #7178, #32743, #11821, #17659, #4097, #28120, #17152, #32904, #22298, #12507, #9236, #4266, #9404, #19720, #19886, #9930, #14740, #12333, #22974, #33433, #20406, #25375, #27610, #1679, #1856, #22803, #20240, #30680, #30857, #7350, #30340, #17834 ),
 ( #28290, #6838, #17318, #24860, #18691, #28624, #18011, #2198, #26233, #4949, #18353, #2722, #10786, #13185, #15430, #21095, #31540, #8034, #28796, #15606, #33952, #25883, #13021, #33788, #31371, #23834, #299, #10280, #2893, #5122, #23662, #12673, #10445, #26061, #18521, #2376, #12849, #23493, #23323, #31031, #23141, #5295, #20586, #28967, #28458, #33607, #10107, #7528, #20760, #20922, #15944, #2554, #18181, #29130, #5463, #26400, #7862, #31204, #15777, #125, #7695, #13360, #10616, #21263, #31708, #8200, #15256, #25718, #5800, #26738, #8701, #26896, #3395, #13865, #16116, #24330, #16280, #21921, #13536, #26570, #32371, #18852, #8867, #10953, #3231, #3066, #19351, #23999, #8537, #24164, #470, #13700, #24652, #19023, #27062, #16773, #29793, #6297, #19184, #21429, #16444, #29463, #804, #11286, #21765, #29622, #32208, #31869, #27233, #3555, #634, #1125, #22092, #3726, #11124, #8364, #32536, #11610, #9036, #6125, #14196, #21592, #32038, #16609, #19515, #5966, #29300, #14028, #24491, #964, #11445, #5633, #25508, #6966, #19680, #1810, #12286, #22760, #9539, #30295, #14700, #30126, #27737, #14528, #12112, #4566, #15044, #24989, #17615, #9361, #4394, #16942, #25158, #19842, #33211, #6629, #17108, #4227, #4054, #11778, #22416, #1988, #30467, #9195, #27567, #28077, #12463, #6796, #1472, #9713, #22933, #1635, #6469, #17275, #14867, #11947, #20021, #20195, #22584, #33389, #9888, #25332, #33035, #22258, #17451, #32864, #27911, #29963, #27399, #30639, #7135, #3889, #14361, #24819, #1296, #32701, #4733, #31788, #16362, #5885, #29385, #8279, #13105, #718, #212, #26817, #3313, #15214, #29215, #20365, #387, #15860, #18607, #30813, #21180, #18771, #13779, #24247, #24085, #26146, #2642, #7306, #31459, #23578, #2980, #13448, #26316, #7952, #10872, #8120, #5721, #553, #11039, #29046, #23915, #17790, #21347, #16199, #31622, #5549, #28250, #44, #18439, #26653, #10532, #3148, #5381, #21507, #2805, #13620, #21009, #31956, #16030, #8449, #28883, #18940, #13272, #23747, #10699, #26485, #29706, #22340, #6551, #1389, #29539, #24736, #27654, #11862, #6382, #32786, #27318, #3808, #9279, #11692, #19101, #29881, #19763, #24904, #11524, #14617, #22176, #30213, #6715, #9117, #26974, #24572, #32621, #17196, #6041, #4143, #8619, #16859, #25073, #3640, #19599, #22005, #16522, #11204, #30046, #21842, #14279, #3474, #8953, #1211, #11366, #32287, #17025, #32452, #19432, #27484, #21675, #3974, #8780, #14446, #13945, #32123, #24408, #884, #19264, #6209, #16690, #27147, #14114, #1044, #4482, #20111, #30381, #33125, #20634, #14958, #23023, #12721, #15303, #17885, #15134, #19934, #12378, #25424, #22847, #7222, #33306, #25597, #9805, #32949, #28337, #33478, #12203, #31076, #18053, #2247, #7052, #6882, #28498, #7571, #4994, #28167, #33654, #30556, #17534, #17708, #15477, #1902, #4308, #22500, #12552, #25248, #4654, #9978, #1554, #20454, #1723, #7399, #4823, #25762, #2077, #20281, #30728, #22674, #30905, #27995, #23192, #10152, #12031, #9452, #17362 ),
 ( #27826, #9629, #14783, #23536, #26273, #13405, #29006, #23874, #10324, #2935, #21469, #10998, #512, #343, #18226, #5843, #5336, #31913, #8407, #20801, #10827, #25930, #5507, #20965, #23702, #2424, #2761, #15987, #18895, #16157, #21137, #3109, #8077, #18563, #26611, #26444, #33827, #10658, #13580, #5679, #13227, #29343, #21307, #12892, #24043, #31747, #7737, #15819, #8239, #23367, #31245, #28672, #5166, #31578, #15652, #18393, #18732, #168, #26102, #29172, #2599, #13061, #4392, #10488, #31416, #7909, #28839, #9079, #24534, #1344, #11825, #24697, #29665, #8579, #27107, #26936, #16653, #24863, #13737, #3435, #3769, #13907, #3600, #14240, #19394, #1174, #678, #27276, #22302, #32747, #9240, #11654, #19061, #30172, #6170, #19725, #16322, #11165, #22137, #26779, #29840, #11324, #14074, #3269, #1005, #32580, #24206, #21636, #19561, #32082, #29501, #6006, #24373, #16480, #32415, #8909, #21801, #845, #6342, #11488, #30009, #6514, #16986, #21966, #16820, #32251, #27443, #3935, #14409, #8744, #19227, #14575, #27785, #33265, #1516, #28124, #25207, #9936, #1685, #9759, #6843, #17663, #1861, #22979, #4102, #7183, #17322, #32910, #2202, #20411, #12160, #17840, #2037, #30861, #25036, #7354, #11991, #20244, #23147, #33611, #28294, #22634, #22459, #10112, #12679, #20591, #30685, #4782, #33087, #9589, #12337, #6675, #20070, #9409, #27615, #4612, #30343, #15088, #25556, #17158, #12511, #4271, #33438, #15261, #25722, #19892, #7012, #25381, #14745, #4439, #30514, #22807, #17495, #27957, #14915, #18694, #10450, #5467, #18016, #15781, #20928, #2897, #31208, #18186, #5299, #5126, #12853, #23498, #26572, #31543, #10285, #7699, #29134, #5636, #31375, #28462, #129, #2382, #10791, #20764, #4954, #15435, #23328, #28628, #2726, #31712, #7866, #33956, #10956, #21269, #8204, #23667, #15613, #26237, #15949, #33792, #16119, #26405, #26065, #10620, #2558, #28802, #13190, #13025, #18357, #21099, #8039, #18525, #28971, #7532, #13364, #23838, #303, #25887, #3069, #13539, #24002, #473, #31036, #8541, #31873, #14201, #5803, #24335, #5971, #16283, #19025, #6474, #809, #8871, #32541, #1129, #3730, #968, #26741, #32212, #11290, #8705, #27067, #19188, #11449, #29626, #18855, #24495, #3234, #11614, #638, #8369, #29303, #13702, #21597, #3560, #22096, #21769, #6129, #1301, #9040, #19519, #14033, #11127, #16613, #6301, #24167, #29967, #29798, #32041, #21925, #29466, #32375, #19355, #16448, #26900, #16777, #27237, #24656, #16946, #3399, #27404, #13869, #3893, #14365, #24822, #21431, #24993, #15048, #17112, #32868, #22262, #4570, #30130, #14704, #30299, #6633, #9365, #30818, #25162, #33217, #22937, #25512, #28081, #25336, #27571, #22588, #1640, #33040, #17455, #9544, #1814, #20025, #9199, #4060, #1992, #12116, #1476, #28254, #12467, #17279, #14532, #4737, #7310, #15218, #4398, #9892, #6800, #27740, #27915, #25681, #30471, #11950, #32704, #22764, #22419, #14872, #9716, #17795, #20199, #19847, #17620, #33393, #20369, #12291, #6970, #30642, #4230, #7139 ),
 ( #11782, #19684, #23283, #10407, #10244, #17972, #28587, #31670, #2689, #15392, #2338, #23796, #262, #26024, #23105, #15907, #20724, #13323, #31507, #26363, #10749, #18144, #28762, #21057, #31335, #21226, #18316, #5258, #2852, #13149, #10067, #20886, #8164, #18654, #2516, #5596, #23623, #29092, #16078, #91, #28423, #15570, #10579, #2161, #20547, #12635, #33569, #7827, #30993, #5085, #8000, #12982, #25848, #5427, #7492, #15739, #4912, #23456, #18484, #33749, #26194, #28928, #12811, #31165, #7657, #33918, #5933, #18818, #3359, #3197, #26864, #1092, #23964, #13666, #13995, #24130, #13829, #24456, #29588, #931, #10918, #3522, #22055, #11575, #32500, #11411, #29261, #6433, #16411, #9000, #19481, #21390, #21887, #26533, #6090, #21558, #24298, #3027, #770, #32337, #29930, #13498, #29756, #31835, #8329, #434, #596, #5765, #8666, #19150, #32002, #11087, #16572, #11251, #8830, #6261, #16740, #21728, #27027, #16245, #19314, #27198, #32173, #3688, #26700, #8498, #18986, #14162, #29430, #24618, #1433, #20162, #11912, #9505, #17072, #27877, #12079, #33178, #14327, #17415, #27532, #9163, #12429, #25302, #30260, #19647, #27702, #4020, #17242, #25476, #24783, #14494, #4361, #24952, #4192, #14836, #19986, #1772, #1261, #12252, #22898, #1955, #33356, #22729, #30089, #30780, #6763, #9853, #20330, #11741, #9680, #16905, #30433, #22384, #14664, #27367, #25124, #30606, #3852, #22221, #7102, #32668, #6595, #32833, #9323, #19810, #32998, #6932, #1602, #22547, #17585, #28046, #4533, #15007, #31466, #5045, #23415, #21186, #7786, #33877, #18100, #25982, #15866, #15181, #28386, #10370, #2124, #28722, #25810, #10538, #2301, #20848, #7451, #18275, #2475, #23585, #4701, #5217, #17936, #33530, #2811, #21015, #12773, #18445, #2648, #7958, #28888, #23247, #31294, #26154, #12942, #5388, #15700, #13111, #26323, #50, #25646, #13278, #23753, #218, #7620, #10705, #7273, #17756, #28214, #12599, #23069, #20687, #10033, #20508, #30954, #4875, #15356, #33708, #10206, #31128, #28548, #15529, #10878, #891, #24578, #5891, #8126, #21514, #6047, #29221, #21683, #24414, #16369, #16697, #27153, #18614, #724, #2986, #11372, #21353, #29052, #5557, #13455, #31795, #3319, #32293, #31962, #559, #11998, #21848, #8787, #24254, #8287, #26823, #16530, #23923, #19271, #26981, #18777, #11210, #393, #29391, #13786, #5727, #16205, #32130, #18946, #8625, #19108, #16036, #29546, #26659, #13951, #26491, #3155, #29712, #13627, #6216, #24091, #11049, #8457, #3645, #3480, #14121, #1524, #31628, #20078, #7538, #25390, #9943, #33619, #2209, #4789, #2044, #6852, #33273, #1867, #9767, #28133, #20251, #12519, #30693, #19901, #17329, #25730, #12345, #12168, #4961, #23154, #27964, #27793, #15441, #18022, #25893, #15098, #20598, #7020, #4446, #4620, #2389, #22814, #25214, #9416, #33445, #22642, #25564, #20418, #28468, #30869, #33094, #28302, #15268, #12688, #22986, #7190, #17671, #9597, #7362, #17502, #17848, #31044, #22467, #14923, #10119, #32917, #30350, #4278, #14752, #1692 ),
 ( #30521, #10961, #2731, #2564, #29308, #13544, #18363, #7706, #5810, #8374, #16288, #5474, #21436, #31382, #28808, #18530, #26746, #26243, #15619, #33798, #23843, #13032, #15954, #308, #18861, #10796, #23505, #18700, #29139, #5641, #26410, #13195, #31548, #33962, #10627, #7873, #28976, #31879, #12859, #5304, #478, #23672, #21274, #10293, #8044, #135, #16125, #10456, #20935, #21104, #15786, #28634, #2902, #23335, #13372, #26071, #31717, #20770, #31214, #8209, #18193, #26579, #5133, #3075, #24007, #24172, #644, #19032, #3404, #8877, #3900, #3567, #6134, #17119, #16952, #27411, #29806, #26905, #11457, #22102, #8546, #14371, #11620, #13874, #6307, #29471, #974, #32381, #24342, #814, #16784, #24501, #21931, #19361, #13707, #27243, #11295, #19525, #11133, #21603, #29974, #16453, #6480, #5976, #21774, #32046, #24828, #32220, #16618, #8710, #19193, #29631, #22268, #27073, #24663, #1307, #11788, #32710, #3736, #14039, #14207, #1135, #32547, #9046, #9206, #19690, #30136, #6639, #3239, #15054, #9551, #22943, #33401, #20031, #14540, #1820, #22426, #25519, #19853, #25000, #1482, #32874, #6806, #14879, #12473, #30477, #33047, #4743, #1998, #9898, #25343, #30307, #17461, #7145, #9371, #20375, #30648, #17285, #12298, #27748, #27921, #4404, #4236, #14710, #22770, #6978, #33223, #9722, #27577, #20208, #25168, #30823, #11956, #1647, #7316, #12122, #17801, #22595, #17626, #4066, #28088, #28259, #4576, #26617, #13412, #18572, #26280, #351, #7916, #18738, #2941, #24048, #5176, #8245, #18400, #5, #3275, #21474, #2771, #18902, #3114, #31921, #29348, #23709, #10834, #13586, #23880, #5849, #21313, #31754, #8413, #29180, #15659, #26450, #16328, #26784, #8085, #11171, #5685, #13743, #24213, #16163, #23544, #21144, #517, #685, #26109, #21642, #2607, #11004, #7744, #175, #18233, #29013, #20972, #28679, #13068, #15994, #10495, #31585, #31423, #5345, #28846, #15826, #13235, #10665, #5513, #6520, #11493, #24379, #8916, #8749, #32420, #6681, #29508, #19233, #19567, #29670, #24869, #11331, #1351, #3442, #6176, #8584, #11831, #16486, #22308, #6012, #17165, #27622, #4109, #1010, #30016, #9247, #32754, #14416, #11661, #26942, #19399, #21972, #29849, #3775, #6348, #22142, #16827, #13912, #851, #19733, #27283, #21807, #14581, #30178, #3607, #32256, #25042, #1523, #11997, #24703, #32088, #16658, #14080, #14246, #19068, #1180, #27115, #24539, #9085, #32587, #16991, #27450, #3941, #33444, #12167, #28301, #4788, #15267, #2043, #22813, #7189, #22641, #20250, #7019, #4619, #31043, #7537, #17501, #10118, #1866, #30868, #9415, #17670, #12344, #25729, #33093, #9596, #30692, #30520, #4277, #14922, #18021, #22985, #1691, #20077, #20597, #28467, #33272, #19900, #25563, #27792, #2208, #27963, #30349, #6851, #14751, #4445, #28132, #23153, #9766, #25389, #2388, #12687, #33618, #15097, #12518, #9942, #7361, #25213, #4960, #17847, #20417, #15440, #25892, #22466, #32916, #17328, #33961, #15953, #134, #10626, #21103, #23334, #31547, #23504, #29138, #20769 ),
 ( #15785, #26745, #26578, #3074, #5473, #2563, #8043, #31716, #18192, #13543, #21273, #10455, #26409, #28633, #18529, #28975, #13031, #20934, #2901, #13371, #23842, #307, #33797, #10795, #31381, #5640, #31213, #10292, #16124, #26070, #24006, #5132, #7872, #7705, #477, #15618, #10960, #18362, #31878, #8373, #18860, #26242, #8208, #21435, #29307, #5809, #18699, #28807, #23671, #2730, #16287, #12858, #5303, #13194, #24500, #643, #21602, #6479, #27072, #26904, #19689, #3899, #8709, #32045, #30135, #32709, #6638, #29805, #1306, #21773, #19192, #8876, #17118, #16617, #5975, #24171, #14206, #3403, #6306, #24662, #9205, #1134, #13873, #9045, #19524, #29973, #16783, #3566, #21930, #24341, #973, #32219, #19360, #11787, #22267, #29630, #24827, #14038, #11619, #11132, #32380, #11456, #16951, #813, #11294, #27242, #6133, #19031, #3735, #3238, #22101, #16452, #32546, #13706, #8545, #27410, #29470, #14370, #11955, #4403, #6977, #14878, #33222, #25342, #7144, #1819, #24999, #22425, #30822, #17460, #17284, #10071, #28258, #33046, #32873, #20552, #23109, #30998, #20207, #25685, #12121, #9550, #9721, #7496, #27920, #30306, #14539, #4575, #27747, #30647, #15053, #33573, #25518, #4235, #33400, #9897, #20374, #17625, #12297, #22769, #14709, #28087, #22594, #1997, #2165, #12639, #20030, #15222, #12472, #22942, #1481, #7315, #17800, #4742, #25167, #1646, #27576, #30476, #9370, #4065, #19852, #6805, #31170, #18148, #5602, #16084, #7831, #4917, #21061, #23288, #31675, #7661, #15397, #25852, #33756, #28591, #23628, #18659, #18320, #20890, #31841, #8169, #29097, #10584, #5089, #26199, #2858, #10248, #26538, #26369, #15574, #31511, #20729, #15744, #13153, #26028, #2520, #8005, #5262, #2693, #95, #28427, #18490, #12989, #267, #2343, #12815, #10754, #23460, #21232, #33922, #10412, #31339, #3032, #28766, #13505, #28933, #23969, #439, #10923, #5432, #15913, #21395, #17977, #13328, #23801, #11580, #32178, #32008, #24788, #9006, #13834, #3203, #1267, #3860, #11747, #937, #6439, #26869, #24302, #13999, #22226, #21733, #11094, #29267, #19319, #8503, #11417, #29761, #14332, #6268, #18991, #14167, #24624, #1097, #21892, #8673, #27032, #29435, #6096, #3364, #24461, #16910, #27372, #775, #29935, #19155, #16745, #5770, #3527, #29594, #22061, #5937, #16417, #16577, #11257, #24135, #32342, #8334, #8836, #21563, #27203, #18824, #16250, #3694, #26706, #32505, #13671, #19486, #602, #19652, #30094, #14500, #32838, #4833, #33838, #33005, #1606, #13071, #12902, #23377, #25772, #22389, #6938, #18062, #4025, #10335, #7584, #9329, #2258, #24957, #30439, #27882, #19815, #30267, #12732, #19992, #17421, #15313, #9168, #23203, #6767, #15487, #6601, #17078, #25941, #11918, #2435, #1441, #17248, #27538, #20811, #27708, #31255, #4198, #18236, #28682, #5180, #12084, #20644, #7747, #15663, #26112, #33665, #14669, #9510, #22552, #10162, #31087, #28507, #5004, #2610, #25129, #32672, #8248, #688, #3279, #23883, #26945, #520, #8587, #11174, #21477, #5348, #2944 ) ),
 .UNSPECIFIED., .T., .F., .T. ) 
 B_SPLINE_SURFACE_WITH_KNOTS ( ( 4, 3, 4 ),
 ( 3, 2, 2, 2, 2, 2, 2, 2, 2, 2, 2, 2, 2, 2, 2, 2, 2, 2, 2, 2, 2, 2, 2, 2, 2, 2, 2, 2, 2, 2, 2, 2, 2, 2, 2, 2, 2, 2, 2, 2, 2, 2, 2, 2, 2, 2, 2, 2, 2, 2, 2, 2, 2, 2, 2, 2, 2, 2, 2, 2, 2, 2, 2, 2, 2, 2, 2, 2, 2, 2, 2, 2, 2, 2, 2, 2, 2, 2, 2, 2, 2, 2, 2, 2, 2, 2, 2, 2, 2, 2, 2, 2, 2, 2, 2, 2, 2, 2, 2, 2, 2, 2, 2, 2, 2, 2, 2, 2, 2, 2, 2, 2, 2, 2, 2, 2, 2, 2, 2, 2, 2, 2, 2, 2, 2, 2, 2, 2, 2, 2, 2, 2, 2, 2, 2, 2, 2, 2, 2, 2, 2, 2, 2, 2, 2, 2, 2, 2, 2, 2, 2, 2, 2, 2, 2, 2, 2, 2, 2, 2, 2, 2, 2, 2, 2, 2, 2, 2, 2, 2, 2, 2, 2, 2, 2, 2, 2, 2, 2, 2, 2, 2, 2, 2, 2, 2, 2, 2, 2, 2, 2, 2, 3 ),
 ( 0.000000000000000000, 0.5000000000000000000, 1.000000000000000000 ),
 ( 0.000000000000000000, 0.005208333333333333044, 0.01041666666666666609, 0.01562500000000000000, 0.02083333333333333218, 0.02604166666666666782, 0.03125000000000000000, 0.03645833333333333565, 0.04166666666666666435, 0.04687500000000000000, 0.05208333333333333565, 0.05729166666666666435, 0.06250000000000000000, 0.06770833333333332871, 0.07291666666666667129, 0.07812500000000000000, 0.08333333333333332871, 0.08854166666666667129, 0.09375000000000000000, 0.09895833333333332871, 0.1041666666666666713, 0.1093750000000000000, 0.1145833333333333287, 0.1197916666666666713, 0.1250000000000000000, 0.1302083333333333426, 0.1354166666666666574, 0.1406250000000000000, 0.1458333333333333426, 0.1510416666666666574, 0.1562500000000000000, 0.1614583333333333426, 0.1666666666666666574, 0.1718750000000000000, 0.1770833333333333426, 0.1822916666666666574, 0.1875000000000000000, 0.1927083333333333426, 0.1979166666666666574, 0.2031250000000000000, 0.2083333333333333426, 0.2135416666666666574, 0.2187500000000000000, 0.2239583333333333426, 0.2291666666666666574, 0.2343750000000000000, 0.2395833333333333426, 0.2447916666666666574, 0.2500000000000000000, 0.2552083333333333148, 0.2604166666666666852, 0.2656250000000000000, 0.2708333333333333148, 0.2760416666666666852, 0.2812500000000000000, 0.2864583333333333148, 0.2916666666666666852, 0.2968750000000000000, 0.3020833333333333148, 0.3072916666666666852, 0.3125000000000000000, 0.3177083333333333148, 0.3229166666666666852, 0.3281250000000000000, 0.3333333333333333148, 0.3385416666666666852, 0.3437500000000000000, 0.3489583333333333148, 0.3541666666666666852, 0.3593750000000000000, 0.3645833333333333148, 0.3697916666666666852, 0.3750000000000000000, 0.3802083333333333148, 0.3854166666666666852, 0.3906250000000000000, 0.3958333333333333148, 0.4010416666666666852, 0.4062500000000000000, 0.4114583333333333148, 0.4166666666666666852, 0.4218750000000000000, 0.4270833333333333148, 0.4322916666666666852, 0.4375000000000000000, 0.4427083333333333148, 0.4479166666666666852, 0.4531250000000000000, 0.4583333333333333148, 0.4635416666666666852, 0.4687500000000000000, 0.4739583333333333148, 0.4791666666666666852, 0.4843750000000000000, 0.4895833333333333148, 0.4947916666666666852, 0.5000000000000000000, 0.5052083333333333703, 0.5104166666666666297, 0.5156250000000000000, 0.5208333333333333703, 0.5260416666666666297, 0.5312500000000000000, 0.5364583333333333703, 0.5416666666666666297, 0.5468750000000000000, 0.5520833333333333703, 0.5572916666666666297, 0.5625000000000000000, 0.5677083333333333703, 0.5729166666666666297, 0.5781250000000000000, 0.5833333333333333703, 0.5885416666666666297, 0.5937500000000000000, 0.5989583333333333703, 0.6041666666666666297, 0.6093750000000000000, 0.6145833333333333703, 0.6197916666666666297, 0.6250000000000000000, 0.6302083333333333703, 0.6354166666666666297, 0.6406250000000000000, 0.6458333333333333703, 0.6510416666666666297, 0.6562500000000000000, 0.6614583333333333703, 0.6666666666666666297, 0.6718750000000000000, 0.6770833333333333703, 0.6822916666666666297, 0.6875000000000000000, 0.6927083333333333703, 0.6979166666666666297, 0.7031250000000000000, 0.7083333333333333703, 0.7135416666666666297, 0.7187500000000000000, 0.7239583333333333703, 0.7291666666666666297, 0.7343750000000000000, 0.7395833333333333703, 0.7447916666666666297, 0.7500000000000000000, 0.7552083333333333703, 0.7604166666666666297, 0.7656250000000000000, 0.7708333333333333703, 0.7760416666666666297, 0.7812500000000000000, 0.7864583333333333703, 0.7916666666666666297, 0.7968750000000000000, 0.8020833333333333703, 0.8072916666666666297, 0.8125000000000000000, 0.8177083333333333703, 0.8229166666666666297, 0.8281250000000000000, 0.8333333333333333703, 0.8385416666666666297, 0.8437500000000000000, 0.8489583333333333703, 0.8541666666666666297, 0.8593750000000000000, 0.8645833333333333703, 0.8697916666666666297, 0.8750000000000000000, 0.8802083333333333703, 0.8854166666666666297, 0.8906250000000000000, 0.8958333333333333703, 0.9010416666666666297, 0.9062500000000000000, 0.9114583333333333703, 0.9166666666666666297, 0.9218750000000000000, 0.9270833333333333703, 0.9322916666666666297, 0.9375000000000000000, 0.9427083333333333703, 0.9479166666666666297, 0.9531250000000000000, 0.9583333333333333703, 0.9635416666666666297, 0.9687500000000000000, 0.9739583333333333703, 0.9791666666666666297, 0.9843750000000000000, 0.9895833333333333703, 0.9947916666666666297, 1.000000000000000000 ),
 .UNSPECIFIED. ) 
 GEOMETRIC_REPRESENTATION_ITEM ( )  RATIONAL_B_SPLINE_SURFACE ( (
 ( 1.000000000000000000, 0.9659258262890683122, 1.000000000000000000, 0.9659258262890683122, 1.000000000000000000, 0.9659258262890683122, 1.000000000000000000, 0.9659258262890683122, 1.000000000000000000, 0.9659258262890683122, 1.000000000000000000, 0.9659258262890683122, 1.000000000000000000, 0.9659258262890683122, 1.000000000000000000, 0.9659258262890683122, 1.000000000000000000, 0.9659258262890683122, 1.000000000000000000, 0.9659258262890683122, 1.000000000000000000, 0.9659258262890683122, 1.000000000000000000, 0.9659258262890683122, 1.000000000000000000, 0.9659258262890683122, 1.000000000000000000, 0.9659258262890683122, 1.000000000000000000, 0.9659258262890683122, 1.000000000000000000, 0.9659258262890683122, 1.000000000000000000, 0.9659258262890683122, 1.000000000000000000, 0.9659258262890683122, 1.000000000000000000, 0.9659258262890683122, 1.000000000000000000, 0.9659258262890683122, 1.000000000000000000, 0.9659258262890683122, 1.000000000000000000, 0.9659258262890683122, 1.000000000000000000, 0.9659258262890683122, 1.000000000000000000, 0.9659258262890683122, 1.000000000000000000, 0.9659258262890683122, 1.000000000000000000, 0.9659258262890683122, 1.000000000000000000, 0.9659258262890683122, 1.000000000000000000, 0.9659258262890683122, 1.000000000000000000, 0.9659258262890683122, 1.000000000000000000, 0.9659258262890683122, 1.000000000000000000, 0.9659258262890683122, 1.000000000000000000, 0.9659258262890683122, 1.000000000000000000, 0.9659258262890683122, 1.000000000000000000, 0.9659258262890683122, 1.000000000000000000, 0.9659258262890683122, 1.000000000000000000, 0.9659258262890683122, 1.000000000000000000, 0.9659258262890683122, 1.000000000000000000, 0.9659258262890683122, 1.000000000000000000, 0.9659258262890683122, 1.000000000000000000, 0.9659258262890683122, 1.000000000000000000, 0.9659258262890683122, 1.000000000000000000, 0.9659258262890683122, 1.000000000000000000, 0.9659258262890683122, 1.000000000000000000, 0.9659258262890683122, 1.000000000000000000, 0.9659258262890683122, 1.000000000000000000, 0.9659258262890683122, 1.000000000000000000, 0.9659258262890683122, 1.000000000000000000, 0.9659258262890683122, 1.000000000000000000, 0.9659258262890683122, 1.000000000000000000, 0.9659258262890683122, 1.000000000000000000, 0.9659258262890683122, 1.000000000000000000, 0.9659258262890683122, 1.000000000000000000, 0.9659258262890683122, 1.000000000000000000, 0.9659258262890683122, 1.000000000000000000, 0.9659258262890683122, 1.000000000000000000, 0.9659258262890683122, 1.000000000000000000, 0.9659258262890683122, 1.000000000000000000, 0.9659258262890683122, 1.000000000000000000, 0.9659258262890683122, 1.000000000000000000, 0.9659258262890683122, 1.000000000000000000, 0.9659258262890683122, 1.000000000000000000, 0.9659258262890683122, 1.000000000000000000, 0.9659258262890683122, 1.000000000000000000, 0.9659258262890683122, 1.000000000000000000, 0.9659258262890683122, 1.000000000000000000, 0.9659258262890683122, 1.000000000000000000, 0.9659258262890683122, 1.000000000000000000, 0.9659258262890683122, 1.000000000000000000, 0.9659258262890683122, 1.000000000000000000, 0.9659258262890683122, 1.000000000000000000, 0.9659258262890683122, 1.000000000000000000, 0.9659258262890683122, 1.000000000000000000, 0.9659258262890683122, 1.000000000000000000, 0.9659258262890683122, 1.000000000000000000, 0.9659258262890683122, 1.000000000000000000, 0.9659258262890683122, 1.000000000000000000, 0.9659258262890683122, 1.000000000000000000, 0.9659258262890683122, 1.000000000000000000, 0.9659258262890683122, 1.000000000000000000, 0.9659258262890683122, 1.000000000000000000, 0.9659258262890683122, 1.000000000000000000, 0.9659258262890683122, 1.000000000000000000, 0.9659258262890683122, 1.000000000000000000, 0.9659258262890683122, 1.000000000000000000, 0.9659258262890683122, 1.000000000000000000, 0.9659258262890683122, 1.000000000000000000, 0.9659258262890683122, 1.000000000000000000, 0.9659258262890683122, 1.000000000000000000, 0.9659258262890683122, 1.000000000000000000, 0.9659258262890683122, 1.000000000000000000, 0.9659258262890683122, 1.000000000000000000, 0.9659258262890683122, 1.000000000000000000, 0.9659258262890683122, 1.000000000000000000, 0.9659258262890683122, 1.000000000000000000, 0.9659258262890683122, 1.000000000000000000, 0.9659258262890683122, 1.000000000000000000, 0.9659258262890683122, 1.000000000000000000, 0.9659258262890683122, 1.000000000000000000, 0.9659258262890683122, 1.000000000000000000, 0.9659258262890683122, 1.000000000000000000, 0.9659258262890683122, 1.000000000000000000, 0.9659258262890683122, 1.000000000000000000, 0.9659258262890683122, 1.000000000000000000, 0.9659258262890683122, 1.000000000000000000, 0.9659258262890683122, 1.000000000000000000, 0.9659258262890683122, 1.000000000000000000, 0.9659258262890683122, 1.000000000000000000, 0.9659258262890683122, 1.000000000000000000, 0.9659258262890683122, 1.000000000000000000, 0.9659258262890683122, 1.000000000000000000, 0.9659258262890683122, 1.000000000000000000, 0.9659258262890683122, 1.000000000000000000, 0.9659258262890683122, 1.000000000000000000, 0.9659258262890683122, 1.000000000000000000, 0.9659258262890683122, 1.000000000000000000, 0.9659258262890683122, 1.000000000000000000, 0.9659258262890683122, 1.000000000000000000, 0.9659258262890683122, 1.000000000000000000, 0.9659258262890683122, 1.000000000000000000, 0.9659258262890683122, 1.000000000000000000, 0.9659258262890683122, 1.000000000000000000, 0.9659258262890683122, 1.000000000000000000, 0.9659258262890683122, 1.000000000000000000, 0.9659258262890683122, 1.000000000000000000, 0.9659258262890683122, 1.000000000000000000, 0.9659258262890683122, 1.000000000000000000, 0.9659258262890683122, 1.000000000000000000, 0.9659258262890683122, 1.000000000000000000, 0.9659258262890683122, 1.000000000000000000, 0.9659258262890683122, 1.000000000000000000, 0.9659258262890683122, 1.000000000000000000, 0.9659258262890683122, 1.000000000000000000, 0.9659258262890683122, 1.000000000000000000, 0.9659258262890683122, 1.000000000000000000, 0.9659258262890683122, 1.000000000000000000, 0.9659258262890683122, 1.000000000000000000, 0.9659258262890683122, 1.000000000000000000, 0.9659258262890683122, 1.000000000000000000, 0.9659258262890683122, 1.000000000000000000, 0.9659258262890683122, 1.000000000000000000, 0.9659258262890683122, 1.000000000000000000, 0.9659258262890683122, 1.000000000000000000, 0.9659258262890683122, 1.000000000000000000, 0.9659258262890683122, 1.000000000000000000, 0.9659258262890683122, 1.000000000000000000, 0.9659258262890683122, 1.000000000000000000, 0.9659258262890683122, 1.000000000000000000, 0.9659258262890683122, 1.000000000000000000, 0.9659258262890683122, 1.000000000000000000, 0.9659258262890683122, 1.000000000000000000, 0.9659258262890683122, 1.000000000000000000, 0.9659258262890683122, 1.000000000000000000, 0.9659258262890683122, 1.000000000000000000, 0.9659258262890683122, 1.000000000000000000, 0.9659258262890683122, 1.000000000000000000, 0.9659258262890683122, 1.000000000000000000, 0.9659258262890683122, 1.000000000000000000, 0.9659258262890683122, 1.000000000000000000, 0.9659258262890683122, 1.000000000000000000, 0.9659258262890683122, 1.000000000000000000, 0.9659258262890683122, 1.000000000000000000, 0.9659258262890683122, 1.000000000000000000, 0.9659258262890683122, 1.000000000000000000, 0.9659258262890683122, 1.000000000000000000, 0.9659258262890683122, 1.000000000000000000, 0.9659258262890683122, 1.000000000000000000, 0.9659258262890683122, 1.000000000000000000, 0.9659258262890683122, 1.000000000000000000, 0.9659258262890683122, 1.000000000000000000, 0.9659258262890683122, 1.000000000000000000, 0.9659258262890683122, 1.000000000000000000, 0.9659258262890683122, 1.000000000000000000, 0.9659258262890683122, 1.000000000000000000, 0.9659258262890683122, 1.000000000000000000, 0.9659258262890683122, 1.000000000000000000, 0.9659258262890683122, 1.000000000000000000, 0.9659258262890683122, 1.000000000000000000, 0.9659258262890683122, 1.000000000000000000, 0.9659258262890683122, 1.000000000000000000, 0.9659258262890683122, 1.000000000000000000, 0.9659258262890683122, 1.000000000000000000, 0.9659258262890683122, 1.000000000000000000, 0.9659258262890683122, 1.000000000000000000, 0.9659258262890683122, 1.000000000000000000, 0.9659258262890683122, 1.000000000000000000, 0.9659258262890683122, 1.000000000000000000, 0.9659258262890683122, 1.000000000000000000, 0.9659258262890683122, 1.000000000000000000, 0.9659258262890683122, 1.000000000000000000, 0.9659258262890683122, 1.000000000000000000, 0.9659258262890683122, 1.000000000000000000, 0.9659258262890683122, 1.000000000000000000),
 ( 0.3333333333333333703, 0.3219752754296894559, 0.3333333333333333703, 0.3219752754296894559, 0.3333333333333333703, 0.3219752754296894559, 0.3333333333333333703, 0.3219752754296894559, 0.3333333333333333703, 0.3219752754296894559, 0.3333333333333333703, 0.3219752754296894559, 0.3333333333333333703, 0.3219752754296894559, 0.3333333333333333703, 0.3219752754296894559, 0.3333333333333333703, 0.3219752754296894559, 0.3333333333333333703, 0.3219752754296894559, 0.3333333333333333703, 0.3219752754296894559, 0.3333333333333333703, 0.3219752754296894559, 0.3333333333333333703, 0.3219752754296894559, 0.3333333333333333703, 0.3219752754296894559, 0.3333333333333333703, 0.3219752754296894559, 0.3333333333333333703, 0.3219752754296894559, 0.3333333333333333703, 0.3219752754296894559, 0.3333333333333333703, 0.3219752754296894559, 0.3333333333333333703, 0.3219752754296894559, 0.3333333333333333703, 0.3219752754296894559, 0.3333333333333333703, 0.3219752754296894559, 0.3333333333333333703, 0.3219752754296894559, 0.3333333333333333703, 0.3219752754296894559, 0.3333333333333333703, 0.3219752754296894559, 0.3333333333333333703, 0.3219752754296894559, 0.3333333333333333703, 0.3219752754296894559, 0.3333333333333333703, 0.3219752754296894559, 0.3333333333333333703, 0.3219752754296894559, 0.3333333333333333703, 0.3219752754296894559, 0.3333333333333333703, 0.3219752754296894559, 0.3333333333333333703, 0.3219752754296894559, 0.3333333333333333703, 0.3219752754296894559, 0.3333333333333333703, 0.3219752754296894559, 0.3333333333333333703, 0.3219752754296894559, 0.3333333333333333703, 0.3219752754296894559, 0.3333333333333333703, 0.3219752754296894559, 0.3333333333333333703, 0.3219752754296894559, 0.3333333333333333703, 0.3219752754296894559, 0.3333333333333333703, 0.3219752754296894559, 0.3333333333333333703, 0.3219752754296894559, 0.3333333333333333703, 0.3219752754296894559, 0.3333333333333333703, 0.3219752754296894559, 0.3333333333333333703, 0.3219752754296894559, 0.3333333333333333703, 0.3219752754296894559, 0.3333333333333333703, 0.3219752754296894559, 0.3333333333333333703, 0.3219752754296894559, 0.3333333333333333703, 0.3219752754296894559, 0.3333333333333333703, 0.3219752754296894559, 0.3333333333333333703, 0.3219752754296894559, 0.3333333333333333703, 0.3219752754296894559, 0.3333333333333333703, 0.3219752754296894559, 0.3333333333333333703, 0.3219752754296894559, 0.3333333333333333703, 0.3219752754296894559, 0.3333333333333333703, 0.3219752754296894559, 0.3333333333333333703, 0.3219752754296894559, 0.3333333333333333703, 0.3219752754296894559, 0.3333333333333333703, 0.3219752754296894559, 0.3333333333333333703, 0.3219752754296894559, 0.3333333333333333703, 0.3219752754296894559, 0.3333333333333333703, 0.3219752754296894559, 0.3333333333333333703, 0.3219752754296894559, 0.3333333333333333703, 0.3219752754296894559, 0.3333333333333333703, 0.3219752754296894559, 0.3333333333333333703, 0.3219752754296894559, 0.3333333333333333703, 0.3219752754296894559, 0.3333333333333333703, 0.3219752754296894559, 0.3333333333333333703, 0.3219752754296894559, 0.3333333333333333703, 0.3219752754296894559, 0.3333333333333333703, 0.3219752754296894559, 0.3333333333333333703, 0.3219752754296894559, 0.3333333333333333703, 0.3219752754296894559, 0.3333333333333333703, 0.3219752754296894559, 0.3333333333333333703, 0.3219752754296894559, 0.3333333333333333703, 0.3219752754296894559, 0.3333333333333333703, 0.3219752754296894559, 0.3333333333333333703, 0.3219752754296894559, 0.3333333333333333703, 0.3219752754296894559, 0.3333333333333333703, 0.3219752754296894559, 0.3333333333333333703, 0.3219752754296894559, 0.3333333333333333703, 0.3219752754296894559, 0.3333333333333333703, 0.3219752754296894559, 0.3333333333333333703, 0.3219752754296894559, 0.3333333333333333703, 0.3219752754296894559, 0.3333333333333333703, 0.3219752754296894559, 0.3333333333333333703, 0.3219752754296894559, 0.3333333333333333703, 0.3219752754296894559, 0.3333333333333333703, 0.3219752754296894559, 0.3333333333333333703, 0.3219752754296894559, 0.3333333333333333703, 0.3219752754296894559, 0.3333333333333333703, 0.3219752754296894559, 0.3333333333333333703, 0.3219752754296894559, 0.3333333333333333703, 0.3219752754296894559, 0.3333333333333333703, 0.3219752754296894559, 0.3333333333333333703, 0.3219752754296894559, 0.3333333333333333703, 0.3219752754296894559, 0.3333333333333333703, 0.3219752754296894559, 0.3333333333333333703, 0.3219752754296894559, 0.3333333333333333703, 0.3219752754296894559, 0.3333333333333333703, 0.3219752754296894559, 0.3333333333333333703, 0.3219752754296894559, 0.3333333333333333703, 0.3219752754296894559, 0.3333333333333333703, 0.3219752754296894559, 0.3333333333333333703, 0.3219752754296894559, 0.3333333333333333703, 0.3219752754296894559, 0.3333333333333333703, 0.3219752754296894559, 0.3333333333333333703, 0.3219752754296894559, 0.3333333333333333703, 0.3219752754296894559, 0.3333333333333333703, 0.3219752754296894559, 0.3333333333333333703, 0.3219752754296894559, 0.3333333333333333703, 0.3219752754296894559, 0.3333333333333333703, 0.3219752754296894559, 0.3333333333333333703, 0.3219752754296894559, 0.3333333333333333703, 0.3219752754296894559, 0.3333333333333333703, 0.3219752754296894559, 0.3333333333333333703, 0.3219752754296894559, 0.3333333333333333703, 0.3219752754296894559, 0.3333333333333333703, 0.3219752754296894559, 0.3333333333333333703, 0.3219752754296894559, 0.3333333333333333703, 0.3219752754296894559, 0.3333333333333333703, 0.3219752754296894559, 0.3333333333333333703, 0.3219752754296894559, 0.3333333333333333703, 0.3219752754296894559, 0.3333333333333333703, 0.3219752754296894559, 0.3333333333333333703, 0.3219752754296894559, 0.3333333333333333703, 0.3219752754296894559, 0.3333333333333333703, 0.3219752754296894559, 0.3333333333333333703, 0.3219752754296894559, 0.3333333333333333703, 0.3219752754296894559, 0.3333333333333333703, 0.3219752754296894559, 0.3333333333333333703, 0.3219752754296894559, 0.3333333333333333703, 0.3219752754296894559, 0.3333333333333333703, 0.3219752754296894559, 0.3333333333333333703, 0.3219752754296894559, 0.3333333333333333703, 0.3219752754296894559, 0.3333333333333333703, 0.3219752754296894559, 0.3333333333333333703, 0.3219752754296894559, 0.3333333333333333703, 0.3219752754296894559, 0.3333333333333333703, 0.3219752754296894559, 0.3333333333333333703, 0.3219752754296894559, 0.3333333333333333703, 0.3219752754296894559, 0.3333333333333333703, 0.3219752754296894559, 0.3333333333333333703, 0.3219752754296894559, 0.3333333333333333703, 0.3219752754296894559, 0.3333333333333333703, 0.3219752754296894559, 0.3333333333333333703, 0.3219752754296894559, 0.3333333333333333703, 0.3219752754296894559, 0.3333333333333333703, 0.3219752754296894559, 0.3333333333333333703, 0.3219752754296894559, 0.3333333333333333703, 0.3219752754296894559, 0.3333333333333333703, 0.3219752754296894559, 0.3333333333333333703, 0.3219752754296894559, 0.3333333333333333703, 0.3219752754296894559, 0.3333333333333333703, 0.3219752754296894559, 0.3333333333333333703, 0.3219752754296894559, 0.3333333333333333703, 0.3219752754296894559, 0.3333333333333333703, 0.3219752754296894559, 0.3333333333333333703, 0.3219752754296894559, 0.3333333333333333703, 0.3219752754296894559, 0.3333333333333333703, 0.3219752754296894559, 0.3333333333333333703, 0.3219752754296894559, 0.3333333333333333703, 0.3219752754296894559, 0.3333333333333333703, 0.3219752754296894559, 0.3333333333333333703, 0.3219752754296894559, 0.3333333333333333703, 0.3219752754296894559, 0.3333333333333333703, 0.3219752754296894559, 0.3333333333333333703, 0.3219752754296894559, 0.3333333333333333703, 0.3219752754296894559, 0.3333333333333333703, 0.3219752754296894559, 0.3333333333333333703, 0.3219752754296894559, 0.3333333333333333703, 0.3219752754296894559, 0.3333333333333333703, 0.3219752754296894559, 0.3333333333333333703, 0.3219752754296894559, 0.3333333333333333703, 0.3219752754296894559, 0.3333333333333333703, 0.3219752754296894559, 0.3333333333333333703, 0.3219752754296894559, 0.3333333333333333703, 0.3219752754296894559, 0.3333333333333333703, 0.3219752754296894559, 0.3333333333333333703, 0.3219752754296894559, 0.3333333333333333703, 0.3219752754296894559, 0.3333333333333333703, 0.3219752754296894559, 0.3333333333333333703, 0.3219752754296894559, 0.3333333333333333703, 0.3219752754296894559, 0.3333333333333333703, 0.3219752754296894559, 0.3333333333333333703, 0.3219752754296894559, 0.3333333333333333703, 0.3219752754296894559, 0.3333333333333333703, 0.3219752754296894559, 0.3333333333333333703, 0.3219752754296894559, 0.3333333333333333703, 0.3219752754296894559, 0.3333333333333333703, 0.3219752754296894559, 0.3333333333333333703, 0.3219752754296894559, 0.3333333333333333703, 0.3219752754296894559, 0.3333333333333333703, 0.3219752754296894559, 0.3333333333333333703),
 ( 0.3333333333333333703, 0.3219752754296894559, 0.3333333333333333703, 0.3219752754296894559, 0.3333333333333333703, 0.3219752754296894559, 0.3333333333333333703, 0.3219752754296894559, 0.3333333333333333703, 0.3219752754296894559, 0.3333333333333333703, 0.3219752754296894559, 0.3333333333333333703, 0.3219752754296894559, 0.3333333333333333703, 0.3219752754296894559, 0.3333333333333333703, 0.3219752754296894559, 0.3333333333333333703, 0.3219752754296894559, 0.3333333333333333703, 0.3219752754296894559, 0.3333333333333333703, 0.3219752754296894559, 0.3333333333333333703, 0.3219752754296894559, 0.3333333333333333703, 0.3219752754296894559, 0.3333333333333333703, 0.3219752754296894559, 0.3333333333333333703, 0.3219752754296894559, 0.3333333333333333703, 0.3219752754296894559, 0.3333333333333333703, 0.3219752754296894559, 0.3333333333333333703, 0.3219752754296894559, 0.3333333333333333703, 0.3219752754296894559, 0.3333333333333333703, 0.3219752754296894559, 0.3333333333333333703, 0.3219752754296894559, 0.3333333333333333703, 0.3219752754296894559, 0.3333333333333333703, 0.3219752754296894559, 0.3333333333333333703, 0.3219752754296894559, 0.3333333333333333703, 0.3219752754296894559, 0.3333333333333333703, 0.3219752754296894559, 0.3333333333333333703, 0.3219752754296894559, 0.3333333333333333703, 0.3219752754296894559, 0.3333333333333333703, 0.3219752754296894559, 0.3333333333333333703, 0.3219752754296894559, 0.3333333333333333703, 0.3219752754296894559, 0.3333333333333333703, 0.3219752754296894559, 0.3333333333333333703, 0.3219752754296894559, 0.3333333333333333703, 0.3219752754296894559, 0.3333333333333333703, 0.3219752754296894559, 0.3333333333333333703, 0.3219752754296894559, 0.3333333333333333703, 0.3219752754296894559, 0.3333333333333333703, 0.3219752754296894559, 0.3333333333333333703, 0.3219752754296894559, 0.3333333333333333703, 0.3219752754296894559, 0.3333333333333333703, 0.3219752754296894559, 0.3333333333333333703, 0.3219752754296894559, 0.3333333333333333703, 0.3219752754296894559, 0.3333333333333333703, 0.3219752754296894559, 0.3333333333333333703, 0.3219752754296894559, 0.3333333333333333703, 0.3219752754296894559, 0.3333333333333333703, 0.3219752754296894559, 0.3333333333333333703, 0.3219752754296894559, 0.3333333333333333703, 0.3219752754296894559, 0.3333333333333333703, 0.3219752754296894559, 0.3333333333333333703, 0.3219752754296894559, 0.3333333333333333703, 0.3219752754296894559, 0.3333333333333333703, 0.3219752754296894559, 0.3333333333333333703, 0.3219752754296894559, 0.3333333333333333703, 0.3219752754296894559, 0.3333333333333333703, 0.3219752754296894559, 0.3333333333333333703, 0.3219752754296894559, 0.3333333333333333703, 0.3219752754296894559, 0.3333333333333333703, 0.3219752754296894559, 0.3333333333333333703, 0.3219752754296894559, 0.3333333333333333703, 0.3219752754296894559, 0.3333333333333333703, 0.3219752754296894559, 0.3333333333333333703, 0.3219752754296894559, 0.3333333333333333703, 0.3219752754296894559, 0.3333333333333333703, 0.3219752754296894559, 0.3333333333333333703, 0.3219752754296894559, 0.3333333333333333703, 0.3219752754296894559, 0.3333333333333333703, 0.3219752754296894559, 0.3333333333333333703, 0.3219752754296894559, 0.3333333333333333703, 0.3219752754296894559, 0.3333333333333333703, 0.3219752754296894559, 0.3333333333333333703, 0.3219752754296894559, 0.3333333333333333703, 0.3219752754296894559, 0.3333333333333333703, 0.3219752754296894559, 0.3333333333333333703, 0.3219752754296894559, 0.3333333333333333703, 0.3219752754296894559, 0.3333333333333333703, 0.3219752754296894559, 0.3333333333333333703, 0.3219752754296894559, 0.3333333333333333703, 0.3219752754296894559, 0.3333333333333333703, 0.3219752754296894559, 0.3333333333333333703, 0.3219752754296894559, 0.3333333333333333703, 0.3219752754296894559, 0.3333333333333333703, 0.3219752754296894559, 0.3333333333333333703, 0.3219752754296894559, 0.3333333333333333703, 0.3219752754296894559, 0.3333333333333333703, 0.3219752754296894559, 0.3333333333333333703, 0.3219752754296894559, 0.3333333333333333703, 0.3219752754296894559, 0.3333333333333333703, 0.3219752754296894559, 0.3333333333333333703, 0.3219752754296894559, 0.3333333333333333703, 0.3219752754296894559, 0.3333333333333333703, 0.3219752754296894559, 0.3333333333333333703, 0.3219752754296894559, 0.3333333333333333703, 0.3219752754296894559, 0.3333333333333333703, 0.3219752754296894559, 0.3333333333333333703, 0.3219752754296894559, 0.3333333333333333703, 0.3219752754296894559, 0.3333333333333333703, 0.3219752754296894559, 0.3333333333333333703, 0.3219752754296894559, 0.3333333333333333703, 0.3219752754296894559, 0.3333333333333333703, 0.3219752754296894559, 0.3333333333333333703, 0.3219752754296894559, 0.3333333333333333703, 0.3219752754296894559, 0.3333333333333333703, 0.3219752754296894559, 0.3333333333333333703, 0.3219752754296894559, 0.3333333333333333703, 0.3219752754296894559, 0.3333333333333333703, 0.3219752754296894559, 0.3333333333333333703, 0.3219752754296894559, 0.3333333333333333703, 0.3219752754296894559, 0.3333333333333333703, 0.3219752754296894559, 0.3333333333333333703, 0.3219752754296894559, 0.3333333333333333703, 0.3219752754296894559, 0.3333333333333333703, 0.3219752754296894559, 0.3333333333333333703, 0.3219752754296894559, 0.3333333333333333703, 0.3219752754296894559, 0.3333333333333333703, 0.3219752754296894559, 0.3333333333333333703, 0.3219752754296894559, 0.3333333333333333703, 0.3219752754296894559, 0.3333333333333333703, 0.3219752754296894559, 0.3333333333333333703, 0.3219752754296894559, 0.3333333333333333703, 0.3219752754296894559, 0.3333333333333333703, 0.3219752754296894559, 0.3333333333333333703, 0.3219752754296894559, 0.3333333333333333703, 0.3219752754296894559, 0.3333333333333333703, 0.3219752754296894559, 0.3333333333333333703, 0.3219752754296894559, 0.3333333333333333703, 0.3219752754296894559, 0.3333333333333333703, 0.3219752754296894559, 0.3333333333333333703, 0.3219752754296894559, 0.3333333333333333703, 0.3219752754296894559, 0.3333333333333333703, 0.3219752754296894559, 0.3333333333333333703, 0.3219752754296894559, 0.3333333333333333703, 0.3219752754296894559, 0.3333333333333333703, 0.3219752754296894559, 0.3333333333333333703, 0.3219752754296894559, 0.3333333333333333703, 0.3219752754296894559, 0.3333333333333333703, 0.3219752754296894559, 0.3333333333333333703, 0.3219752754296894559, 0.3333333333333333703, 0.3219752754296894559, 0.3333333333333333703, 0.3219752754296894559, 0.3333333333333333703, 0.3219752754296894559, 0.3333333333333333703, 0.3219752754296894559, 0.3333333333333333703, 0.3219752754296894559, 0.3333333333333333703, 0.3219752754296894559, 0.3333333333333333703, 0.3219752754296894559, 0.3333333333333333703, 0.3219752754296894559, 0.3333333333333333703, 0.3219752754296894559, 0.3333333333333333703, 0.3219752754296894559, 0.3333333333333333703, 0.3219752754296894559, 0.3333333333333333703, 0.3219752754296894559, 0.3333333333333333703, 0.3219752754296894559, 0.3333333333333333703, 0.3219752754296894559, 0.3333333333333333703, 0.3219752754296894559, 0.3333333333333333703, 0.3219752754296894559, 0.3333333333333333703, 0.3219752754296894559, 0.3333333333333333703, 0.3219752754296894559, 0.3333333333333333703, 0.3219752754296894559, 0.3333333333333333703, 0.3219752754296894559, 0.3333333333333333703, 0.3219752754296894559, 0.3333333333333333703, 0.3219752754296894559, 0.3333333333333333703, 0.3219752754296894559, 0.3333333333333333703, 0.3219752754296894559, 0.3333333333333333703, 0.3219752754296894559, 0.3333333333333333703, 0.3219752754296894559, 0.3333333333333333703, 0.3219752754296894559, 0.3333333333333333703, 0.3219752754296894559, 0.3333333333333333703, 0.3219752754296894559, 0.3333333333333333703, 0.3219752754296894559, 0.3333333333333333703, 0.3219752754296894559, 0.3333333333333333703, 0.3219752754296894559, 0.3333333333333333703, 0.3219752754296894559, 0.3333333333333333703, 0.3219752754296894559, 0.3333333333333333703, 0.3219752754296894559, 0.3333333333333333703, 0.3219752754296894559, 0.3333333333333333703, 0.3219752754296894559, 0.3333333333333333703, 0.3219752754296894559, 0.3333333333333333703, 0.3219752754296894559, 0.3333333333333333703, 0.3219752754296894559, 0.3333333333333333703, 0.3219752754296894559, 0.3333333333333333703, 0.3219752754296894559, 0.3333333333333333703, 0.3219752754296894559, 0.3333333333333333703, 0.3219752754296894559, 0.3333333333333333703, 0.3219752754296894559, 0.3333333333333333703, 0.3219752754296894559, 0.3333333333333333703, 0.3219752754296894559, 0.3333333333333333703, 0.3219752754296894559, 0.3333333333333333703, 0.3219752754296894559, 0.3333333333333333703, 0.3219752754296894559, 0.3333333333333333703, 0.3219752754296894559, 0.3333333333333333703, 0.3219752754296894559, 0.3333333333333333703, 0.3219752754296894559, 0.3333333333333333703),
 ( 1.000000000000000000, 0.9659258262890683122, 1.000000000000000000, 0.9659258262890683122, 1.000000000000000000, 0.9659258262890683122, 1.000000000000000000, 0.9659258262890683122, 1.000000000000000000, 0.9659258262890683122, 1.000000000000000000, 0.9659258262890683122, 1.000000000000000000, 0.9659258262890683122, 1.000000000000000000, 0.9659258262890683122, 1.000000000000000000, 0.9659258262890683122, 1.000000000000000000, 0.9659258262890683122, 1.000000000000000000, 0.9659258262890683122, 1.000000000000000000, 0.9659258262890683122, 1.000000000000000000, 0.9659258262890683122, 1.000000000000000000, 0.9659258262890683122, 1.000000000000000000, 0.9659258262890683122, 1.000000000000000000, 0.9659258262890683122, 1.000000000000000000, 0.9659258262890683122, 1.000000000000000000, 0.9659258262890683122, 1.000000000000000000, 0.9659258262890683122, 1.000000000000000000, 0.9659258262890683122, 1.000000000000000000, 0.9659258262890683122, 1.000000000000000000, 0.9659258262890683122, 1.000000000000000000, 0.9659258262890683122, 1.000000000000000000, 0.9659258262890683122, 1.000000000000000000, 0.9659258262890683122, 1.000000000000000000, 0.9659258262890683122, 1.000000000000000000, 0.9659258262890683122, 1.000000000000000000, 0.9659258262890683122, 1.000000000000000000, 0.9659258262890683122, 1.000000000000000000, 0.9659258262890683122, 1.000000000000000000, 0.9659258262890683122, 1.000000000000000000, 0.9659258262890683122, 1.000000000000000000, 0.9659258262890683122, 1.000000000000000000, 0.9659258262890683122, 1.000000000000000000, 0.9659258262890683122, 1.000000000000000000, 0.9659258262890683122, 1.000000000000000000, 0.9659258262890683122, 1.000000000000000000, 0.9659258262890683122, 1.000000000000000000, 0.9659258262890683122, 1.000000000000000000, 0.9659258262890683122, 1.000000000000000000, 0.9659258262890683122, 1.000000000000000000, 0.9659258262890683122, 1.000000000000000000, 0.9659258262890683122, 1.000000000000000000, 0.9659258262890683122, 1.000000000000000000, 0.9659258262890683122, 1.000000000000000000, 0.9659258262890683122, 1.000000000000000000, 0.9659258262890683122, 1.000000000000000000, 0.9659258262890683122, 1.000000000000000000, 0.9659258262890683122, 1.000000000000000000, 0.9659258262890683122, 1.000000000000000000, 0.9659258262890683122, 1.000000000000000000, 0.9659258262890683122, 1.000000000000000000, 0.9659258262890683122, 1.000000000000000000, 0.9659258262890683122, 1.000000000000000000, 0.9659258262890683122, 1.000000000000000000, 0.9659258262890683122, 1.000000000000000000, 0.9659258262890683122, 1.000000000000000000, 0.9659258262890683122, 1.000000000000000000, 0.9659258262890683122, 1.000000000000000000, 0.9659258262890683122, 1.000000000000000000, 0.9659258262890683122, 1.000000000000000000, 0.9659258262890683122, 1.000000000000000000, 0.9659258262890683122, 1.000000000000000000, 0.9659258262890683122, 1.000000000000000000, 0.9659258262890683122, 1.000000000000000000, 0.9659258262890683122, 1.000000000000000000, 0.9659258262890683122, 1.000000000000000000, 0.9659258262890683122, 1.000000000000000000, 0.9659258262890683122, 1.000000000000000000, 0.9659258262890683122, 1.000000000000000000, 0.9659258262890683122, 1.000000000000000000, 0.9659258262890683122, 1.000000000000000000, 0.9659258262890683122, 1.000000000000000000, 0.9659258262890683122, 1.000000000000000000, 0.9659258262890683122, 1.000000000000000000, 0.9659258262890683122, 1.000000000000000000, 0.9659258262890683122, 1.000000000000000000, 0.9659258262890683122, 1.000000000000000000, 0.9659258262890683122, 1.000000000000000000, 0.9659258262890683122, 1.000000000000000000, 0.9659258262890683122, 1.000000000000000000, 0.9659258262890683122, 1.000000000000000000, 0.9659258262890683122, 1.000000000000000000, 0.9659258262890683122, 1.000000000000000000, 0.9659258262890683122, 1.000000000000000000, 0.9659258262890683122, 1.000000000000000000, 0.9659258262890683122, 1.000000000000000000, 0.9659258262890683122, 1.000000000000000000, 0.9659258262890683122, 1.000000000000000000, 0.9659258262890683122, 1.000000000000000000, 0.9659258262890683122, 1.000000000000000000, 0.9659258262890683122, 1.000000000000000000, 0.9659258262890683122, 1.000000000000000000, 0.9659258262890683122, 1.000000000000000000, 0.9659258262890683122, 1.000000000000000000, 0.9659258262890683122, 1.000000000000000000, 0.9659258262890683122, 1.000000000000000000, 0.9659258262890683122, 1.000000000000000000, 0.9659258262890683122, 1.000000000000000000, 0.9659258262890683122, 1.000000000000000000, 0.9659258262890683122, 1.000000000000000000, 0.9659258262890683122, 1.000000000000000000, 0.9659258262890683122, 1.000000000000000000, 0.9659258262890683122, 1.000000000000000000, 0.9659258262890683122, 1.000000000000000000, 0.9659258262890683122, 1.000000000000000000, 0.9659258262890683122, 1.000000000000000000, 0.9659258262890683122, 1.000000000000000000, 0.9659258262890683122, 1.000000000000000000, 0.9659258262890683122, 1.000000000000000000, 0.9659258262890683122, 1.000000000000000000, 0.9659258262890683122, 1.000000000000000000, 0.9659258262890683122, 1.000000000000000000, 0.9659258262890683122, 1.000000000000000000, 0.9659258262890683122, 1.000000000000000000, 0.9659258262890683122, 1.000000000000000000, 0.9659258262890683122, 1.000000000000000000, 0.9659258262890683122, 1.000000000000000000, 0.9659258262890683122, 1.000000000000000000, 0.9659258262890683122, 1.000000000000000000, 0.9659258262890683122, 1.000000000000000000, 0.9659258262890683122, 1.000000000000000000, 0.9659258262890683122, 1.000000000000000000, 0.9659258262890683122, 1.000000000000000000, 0.9659258262890683122, 1.000000000000000000, 0.9659258262890683122, 1.000000000000000000, 0.9659258262890683122, 1.000000000000000000, 0.9659258262890683122, 1.000000000000000000, 0.9659258262890683122, 1.000000000000000000, 0.9659258262890683122, 1.000000000000000000, 0.9659258262890683122, 1.000000000000000000, 0.9659258262890683122, 1.000000000000000000, 0.9659258262890683122, 1.000000000000000000, 0.9659258262890683122, 1.000000000000000000, 0.9659258262890683122, 1.000000000000000000, 0.9659258262890683122, 1.000000000000000000, 0.9659258262890683122, 1.000000000000000000, 0.9659258262890683122, 1.000000000000000000, 0.9659258262890683122, 1.000000000000000000, 0.9659258262890683122, 1.000000000000000000, 0.9659258262890683122, 1.000000000000000000, 0.9659258262890683122, 1.000000000000000000, 0.9659258262890683122, 1.000000000000000000, 0.9659258262890683122, 1.000000000000000000, 0.9659258262890683122, 1.000000000000000000, 0.9659258262890683122, 1.000000000000000000, 0.9659258262890683122, 1.000000000000000000, 0.9659258262890683122, 1.000000000000000000, 0.9659258262890683122, 1.000000000000000000, 0.9659258262890683122, 1.000000000000000000, 0.9659258262890683122, 1.000000000000000000, 0.9659258262890683122, 1.000000000000000000, 0.9659258262890683122, 1.000000000000000000, 0.9659258262890683122, 1.000000000000000000, 0.9659258262890683122, 1.000000000000000000, 0.9659258262890683122, 1.000000000000000000, 0.9659258262890683122, 1.000000000000000000, 0.9659258262890683122, 1.000000000000000000, 0.9659258262890683122, 1.000000000000000000, 0.9659258262890683122, 1.000000000000000000, 0.9659258262890683122, 1.000000000000000000, 0.9659258262890683122, 1.000000000000000000, 0.9659258262890683122, 1.000000000000000000, 0.9659258262890683122, 1.000000000000000000, 0.9659258262890683122, 1.000000000000000000, 0.9659258262890683122, 1.000000000000000000, 0.9659258262890683122, 1.000000000000000000, 0.9659258262890683122, 1.000000000000000000, 0.9659258262890683122, 1.000000000000000000, 0.9659258262890683122, 1.000000000000000000, 0.9659258262890683122, 1.000000000000000000, 0.9659258262890683122, 1.000000000000000000, 0.9659258262890683122, 1.000000000000000000, 0.9659258262890683122, 1.000000000000000000, 0.9659258262890683122, 1.000000000000000000, 0.9659258262890683122, 1.000000000000000000, 0.9659258262890683122, 1.000000000000000000, 0.9659258262890683122, 1.000000000000000000, 0.9659258262890683122, 1.000000000000000000, 0.9659258262890683122, 1.000000000000000000, 0.9659258262890683122, 1.000000000000000000, 0.9659258262890683122, 1.000000000000000000, 0.9659258262890683122, 1.000000000000000000, 0.9659258262890683122, 1.000000000000000000, 0.9659258262890683122, 1.000000000000000000, 0.9659258262890683122, 1.000000000000000000, 0.9659258262890683122, 1.000000000000000000, 0.9659258262890683122, 1.000000000000000000, 0.9659258262890683122, 1.000000000000000000, 0.9659258262890683122, 1.000000000000000000, 0.9659258262890683122, 1.000000000000000000, 0.9659258262890683122, 1.000000000000000000),
 ( 0.3333333333333333703, 0.3219752754296894559, 0.3333333333333333703, 0.3219752754296894559, 0.3333333333333333703, 0.3219752754296894559, 0.3333333333333333703, 0.3219752754296894559, 0.3333333333333333703, 0.3219752754296894559, 0.3333333333333333703, 0.3219752754296894559, 0.3333333333333333703, 0.3219752754296894559, 0.3333333333333333703, 0.3219752754296894559, 0.3333333333333333703, 0.3219752754296894559, 0.3333333333333333703, 0.3219752754296894559, 0.3333333333333333703, 0.3219752754296894559, 0.3333333333333333703, 0.3219752754296894559, 0.3333333333333333703, 0.3219752754296894559, 0.3333333333333333703, 0.3219752754296894559, 0.3333333333333333703, 0.3219752754296894559, 0.3333333333333333703, 0.3219752754296894559, 0.3333333333333333703, 0.3219752754296894559, 0.3333333333333333703, 0.3219752754296894559, 0.3333333333333333703, 0.3219752754296894559, 0.3333333333333333703, 0.3219752754296894559, 0.3333333333333333703, 0.3219752754296894559, 0.3333333333333333703, 0.3219752754296894559, 0.3333333333333333703, 0.3219752754296894559, 0.3333333333333333703, 0.3219752754296894559, 0.3333333333333333703, 0.3219752754296894559, 0.3333333333333333703, 0.3219752754296894559, 0.3333333333333333703, 0.3219752754296894559, 0.3333333333333333703, 0.3219752754296894559, 0.3333333333333333703, 0.3219752754296894559, 0.3333333333333333703, 0.3219752754296894559, 0.3333333333333333703, 0.3219752754296894559, 0.3333333333333333703, 0.3219752754296894559, 0.3333333333333333703, 0.3219752754296894559, 0.3333333333333333703, 0.3219752754296894559, 0.3333333333333333703, 0.3219752754296894559, 0.3333333333333333703, 0.3219752754296894559, 0.3333333333333333703, 0.3219752754296894559, 0.3333333333333333703, 0.3219752754296894559, 0.3333333333333333703, 0.3219752754296894559, 0.3333333333333333703, 0.3219752754296894559, 0.3333333333333333703, 0.3219752754296894559, 0.3333333333333333703, 0.3219752754296894559, 0.3333333333333333703, 0.3219752754296894559, 0.3333333333333333703, 0.3219752754296894559, 0.3333333333333333703, 0.3219752754296894559, 0.3333333333333333703, 0.3219752754296894559, 0.3333333333333333703, 0.3219752754296894559, 0.3333333333333333703, 0.3219752754296894559, 0.3333333333333333703, 0.3219752754296894559, 0.3333333333333333703, 0.3219752754296894559, 0.3333333333333333703, 0.3219752754296894559, 0.3333333333333333703, 0.3219752754296894559, 0.3333333333333333703, 0.3219752754296894559, 0.3333333333333333703, 0.3219752754296894559, 0.3333333333333333703, 0.3219752754296894559, 0.3333333333333333703, 0.3219752754296894559, 0.3333333333333333703, 0.3219752754296894559, 0.3333333333333333703, 0.3219752754296894559, 0.3333333333333333703, 0.3219752754296894559, 0.3333333333333333703, 0.3219752754296894559, 0.3333333333333333703, 0.3219752754296894559, 0.3333333333333333703, 0.3219752754296894559, 0.3333333333333333703, 0.3219752754296894559, 0.3333333333333333703, 0.3219752754296894559, 0.3333333333333333703, 0.3219752754296894559, 0.3333333333333333703, 0.3219752754296894559, 0.3333333333333333703, 0.3219752754296894559, 0.3333333333333333703, 0.3219752754296894559, 0.3333333333333333703, 0.3219752754296894559, 0.3333333333333333703, 0.3219752754296894559, 0.3333333333333333703, 0.3219752754296894559, 0.3333333333333333703, 0.3219752754296894559, 0.3333333333333333703, 0.3219752754296894559, 0.3333333333333333703, 0.3219752754296894559, 0.3333333333333333703, 0.3219752754296894559, 0.3333333333333333703, 0.3219752754296894559, 0.3333333333333333703, 0.3219752754296894559, 0.3333333333333333703, 0.3219752754296894559, 0.3333333333333333703, 0.3219752754296894559, 0.3333333333333333703, 0.3219752754296894559, 0.3333333333333333703, 0.3219752754296894559, 0.3333333333333333703, 0.3219752754296894559, 0.3333333333333333703, 0.3219752754296894559, 0.3333333333333333703, 0.3219752754296894559, 0.3333333333333333703, 0.3219752754296894559, 0.3333333333333333703, 0.3219752754296894559, 0.3333333333333333703, 0.3219752754296894559, 0.3333333333333333703, 0.3219752754296894559, 0.3333333333333333703, 0.3219752754296894559, 0.3333333333333333703, 0.3219752754296894559, 0.3333333333333333703, 0.3219752754296894559, 0.3333333333333333703, 0.3219752754296894559, 0.3333333333333333703, 0.3219752754296894559, 0.3333333333333333703, 0.3219752754296894559, 0.3333333333333333703, 0.3219752754296894559, 0.3333333333333333703, 0.3219752754296894559, 0.3333333333333333703, 0.3219752754296894559, 0.3333333333333333703, 0.3219752754296894559, 0.3333333333333333703, 0.3219752754296894559, 0.3333333333333333703, 0.3219752754296894559, 0.3333333333333333703, 0.3219752754296894559, 0.3333333333333333703, 0.3219752754296894559, 0.3333333333333333703, 0.3219752754296894559, 0.3333333333333333703, 0.3219752754296894559, 0.3333333333333333703, 0.3219752754296894559, 0.3333333333333333703, 0.3219752754296894559, 0.3333333333333333703, 0.3219752754296894559, 0.3333333333333333703, 0.3219752754296894559, 0.3333333333333333703, 0.3219752754296894559, 0.3333333333333333703, 0.3219752754296894559, 0.3333333333333333703, 0.3219752754296894559, 0.3333333333333333703, 0.3219752754296894559, 0.3333333333333333703, 0.3219752754296894559, 0.3333333333333333703, 0.3219752754296894559, 0.3333333333333333703, 0.3219752754296894559, 0.3333333333333333703, 0.3219752754296894559, 0.3333333333333333703, 0.3219752754296894559, 0.3333333333333333703, 0.3219752754296894559, 0.3333333333333333703, 0.3219752754296894559, 0.3333333333333333703, 0.3219752754296894559, 0.3333333333333333703, 0.3219752754296894559, 0.3333333333333333703, 0.3219752754296894559, 0.3333333333333333703, 0.3219752754296894559, 0.3333333333333333703, 0.3219752754296894559, 0.3333333333333333703, 0.3219752754296894559, 0.3333333333333333703, 0.3219752754296894559, 0.3333333333333333703, 0.3219752754296894559, 0.3333333333333333703, 0.3219752754296894559, 0.3333333333333333703, 0.3219752754296894559, 0.3333333333333333703, 0.3219752754296894559, 0.3333333333333333703, 0.3219752754296894559, 0.3333333333333333703, 0.3219752754296894559, 0.3333333333333333703, 0.3219752754296894559, 0.3333333333333333703, 0.3219752754296894559, 0.3333333333333333703, 0.3219752754296894559, 0.3333333333333333703, 0.3219752754296894559, 0.3333333333333333703, 0.3219752754296894559, 0.3333333333333333703, 0.3219752754296894559, 0.3333333333333333703, 0.3219752754296894559, 0.3333333333333333703, 0.3219752754296894559, 0.3333333333333333703, 0.3219752754296894559, 0.3333333333333333703, 0.3219752754296894559, 0.3333333333333333703, 0.3219752754296894559, 0.3333333333333333703, 0.3219752754296894559, 0.3333333333333333703, 0.3219752754296894559, 0.3333333333333333703, 0.3219752754296894559, 0.3333333333333333703, 0.3219752754296894559, 0.3333333333333333703, 0.3219752754296894559, 0.3333333333333333703, 0.3219752754296894559, 0.3333333333333333703, 0.3219752754296894559, 0.3333333333333333703, 0.3219752754296894559, 0.3333333333333333703, 0.3219752754296894559, 0.3333333333333333703, 0.3219752754296894559, 0.3333333333333333703, 0.3219752754296894559, 0.3333333333333333703, 0.3219752754296894559, 0.3333333333333333703, 0.3219752754296894559, 0.3333333333333333703, 0.3219752754296894559, 0.3333333333333333703, 0.3219752754296894559, 0.3333333333333333703, 0.3219752754296894559, 0.3333333333333333703, 0.3219752754296894559, 0.3333333333333333703, 0.3219752754296894559, 0.3333333333333333703, 0.3219752754296894559, 0.3333333333333333703, 0.3219752754296894559, 0.3333333333333333703, 0.3219752754296894559, 0.3333333333333333703, 0.3219752754296894559, 0.3333333333333333703, 0.3219752754296894559, 0.3333333333333333703, 0.3219752754296894559, 0.3333333333333333703, 0.3219752754296894559, 0.3333333333333333703, 0.3219752754296894559, 0.3333333333333333703, 0.3219752754296894559, 0.3333333333333333703, 0.3219752754296894559, 0.3333333333333333703, 0.3219752754296894559, 0.3333333333333333703, 0.3219752754296894559, 0.3333333333333333703, 0.3219752754296894559, 0.3333333333333333703, 0.3219752754296894559, 0.3333333333333333703, 0.3219752754296894559, 0.3333333333333333703, 0.3219752754296894559, 0.3333333333333333703, 0.3219752754296894559, 0.3333333333333333703, 0.3219752754296894559, 0.3333333333333333703, 0.3219752754296894559, 0.3333333333333333703, 0.3219752754296894559, 0.3333333333333333703, 0.3219752754296894559, 0.3333333333333333703, 0.3219752754296894559, 0.3333333333333333703, 0.3219752754296894559, 0.3333333333333333703, 0.3219752754296894559, 0.3333333333333333703, 0.3219752754296894559, 0.3333333333333333703, 0.3219752754296894559, 0.3333333333333333703, 0.3219752754296894559, 0.3333333333333333703, 0.3219752754296894559, 0.3333333333333333703, 0.3219752754296894559, 0.3333333333333333703, 0.3219752754296894559, 0.3333333333333333703, 0.3219752754296894559, 0.3333333333333333703),
 ( 0.3333333333333333703, 0.3219752754296894559, 0.3333333333333333703, 0.3219752754296894559, 0.3333333333333333703, 0.3219752754296894559, 0.3333333333333333703, 0.3219752754296894559, 0.3333333333333333703, 0.3219752754296894559, 0.3333333333333333703, 0.3219752754296894559, 0.3333333333333333703, 0.3219752754296894559, 0.3333333333333333703, 0.3219752754296894559, 0.3333333333333333703, 0.3219752754296894559, 0.3333333333333333703, 0.3219752754296894559, 0.3333333333333333703, 0.3219752754296894559, 0.3333333333333333703, 0.3219752754296894559, 0.3333333333333333703, 0.3219752754296894559, 0.3333333333333333703, 0.3219752754296894559, 0.3333333333333333703, 0.3219752754296894559, 0.3333333333333333703, 0.3219752754296894559, 0.3333333333333333703, 0.3219752754296894559, 0.3333333333333333703, 0.3219752754296894559, 0.3333333333333333703, 0.3219752754296894559, 0.3333333333333333703, 0.3219752754296894559, 0.3333333333333333703, 0.3219752754296894559, 0.3333333333333333703, 0.3219752754296894559, 0.3333333333333333703, 0.3219752754296894559, 0.3333333333333333703, 0.3219752754296894559, 0.3333333333333333703, 0.3219752754296894559, 0.3333333333333333703, 0.3219752754296894559, 0.3333333333333333703, 0.3219752754296894559, 0.3333333333333333703, 0.3219752754296894559, 0.3333333333333333703, 0.3219752754296894559, 0.3333333333333333703, 0.3219752754296894559, 0.3333333333333333703, 0.3219752754296894559, 0.3333333333333333703, 0.3219752754296894559, 0.3333333333333333703, 0.3219752754296894559, 0.3333333333333333703, 0.3219752754296894559, 0.3333333333333333703, 0.3219752754296894559, 0.3333333333333333703, 0.3219752754296894559, 0.3333333333333333703, 0.3219752754296894559, 0.3333333333333333703, 0.3219752754296894559, 0.3333333333333333703, 0.3219752754296894559, 0.3333333333333333703, 0.3219752754296894559, 0.3333333333333333703, 0.3219752754296894559, 0.3333333333333333703, 0.3219752754296894559, 0.3333333333333333703, 0.3219752754296894559, 0.3333333333333333703, 0.3219752754296894559, 0.3333333333333333703, 0.3219752754296894559, 0.3333333333333333703, 0.3219752754296894559, 0.3333333333333333703, 0.3219752754296894559, 0.3333333333333333703, 0.3219752754296894559, 0.3333333333333333703, 0.3219752754296894559, 0.3333333333333333703, 0.3219752754296894559, 0.3333333333333333703, 0.3219752754296894559, 0.3333333333333333703, 0.3219752754296894559, 0.3333333333333333703, 0.3219752754296894559, 0.3333333333333333703, 0.3219752754296894559, 0.3333333333333333703, 0.3219752754296894559, 0.3333333333333333703, 0.3219752754296894559, 0.3333333333333333703, 0.3219752754296894559, 0.3333333333333333703, 0.3219752754296894559, 0.3333333333333333703, 0.3219752754296894559, 0.3333333333333333703, 0.3219752754296894559, 0.3333333333333333703, 0.3219752754296894559, 0.3333333333333333703, 0.3219752754296894559, 0.3333333333333333703, 0.3219752754296894559, 0.3333333333333333703, 0.3219752754296894559, 0.3333333333333333703, 0.3219752754296894559, 0.3333333333333333703, 0.3219752754296894559, 0.3333333333333333703, 0.3219752754296894559, 0.3333333333333333703, 0.3219752754296894559, 0.3333333333333333703, 0.3219752754296894559, 0.3333333333333333703, 0.3219752754296894559, 0.3333333333333333703, 0.3219752754296894559, 0.3333333333333333703, 0.3219752754296894559, 0.3333333333333333703, 0.3219752754296894559, 0.3333333333333333703, 0.3219752754296894559, 0.3333333333333333703, 0.3219752754296894559, 0.3333333333333333703, 0.3219752754296894559, 0.3333333333333333703, 0.3219752754296894559, 0.3333333333333333703, 0.3219752754296894559, 0.3333333333333333703, 0.3219752754296894559, 0.3333333333333333703, 0.3219752754296894559, 0.3333333333333333703, 0.3219752754296894559, 0.3333333333333333703, 0.3219752754296894559, 0.3333333333333333703, 0.3219752754296894559, 0.3333333333333333703, 0.3219752754296894559, 0.3333333333333333703, 0.3219752754296894559, 0.3333333333333333703, 0.3219752754296894559, 0.3333333333333333703, 0.3219752754296894559, 0.3333333333333333703, 0.3219752754296894559, 0.3333333333333333703, 0.3219752754296894559, 0.3333333333333333703, 0.3219752754296894559, 0.3333333333333333703, 0.3219752754296894559, 0.3333333333333333703, 0.3219752754296894559, 0.3333333333333333703, 0.3219752754296894559, 0.3333333333333333703, 0.3219752754296894559, 0.3333333333333333703, 0.3219752754296894559, 0.3333333333333333703, 0.3219752754296894559, 0.3333333333333333703, 0.3219752754296894559, 0.3333333333333333703, 0.3219752754296894559, 0.3333333333333333703, 0.3219752754296894559, 0.3333333333333333703, 0.3219752754296894559, 0.3333333333333333703, 0.3219752754296894559, 0.3333333333333333703, 0.3219752754296894559, 0.3333333333333333703, 0.3219752754296894559, 0.3333333333333333703, 0.3219752754296894559, 0.3333333333333333703, 0.3219752754296894559, 0.3333333333333333703, 0.3219752754296894559, 0.3333333333333333703, 0.3219752754296894559, 0.3333333333333333703, 0.3219752754296894559, 0.3333333333333333703, 0.3219752754296894559, 0.3333333333333333703, 0.3219752754296894559, 0.3333333333333333703, 0.3219752754296894559, 0.3333333333333333703, 0.3219752754296894559, 0.3333333333333333703, 0.3219752754296894559, 0.3333333333333333703, 0.3219752754296894559, 0.3333333333333333703, 0.3219752754296894559, 0.3333333333333333703, 0.3219752754296894559, 0.3333333333333333703, 0.3219752754296894559, 0.3333333333333333703, 0.3219752754296894559, 0.3333333333333333703, 0.3219752754296894559, 0.3333333333333333703, 0.3219752754296894559, 0.3333333333333333703, 0.3219752754296894559, 0.3333333333333333703, 0.3219752754296894559, 0.3333333333333333703, 0.3219752754296894559, 0.3333333333333333703, 0.3219752754296894559, 0.3333333333333333703, 0.3219752754296894559, 0.3333333333333333703, 0.3219752754296894559, 0.3333333333333333703, 0.3219752754296894559, 0.3333333333333333703, 0.3219752754296894559, 0.3333333333333333703, 0.3219752754296894559, 0.3333333333333333703, 0.3219752754296894559, 0.3333333333333333703, 0.3219752754296894559, 0.3333333333333333703, 0.3219752754296894559, 0.3333333333333333703, 0.3219752754296894559, 0.3333333333333333703, 0.3219752754296894559, 0.3333333333333333703, 0.3219752754296894559, 0.3333333333333333703, 0.3219752754296894559, 0.3333333333333333703, 0.3219752754296894559, 0.3333333333333333703, 0.3219752754296894559, 0.3333333333333333703, 0.3219752754296894559, 0.3333333333333333703, 0.3219752754296894559, 0.3333333333333333703, 0.3219752754296894559, 0.3333333333333333703, 0.3219752754296894559, 0.3333333333333333703, 0.3219752754296894559, 0.3333333333333333703, 0.3219752754296894559, 0.3333333333333333703, 0.3219752754296894559, 0.3333333333333333703, 0.3219752754296894559, 0.3333333333333333703, 0.3219752754296894559, 0.3333333333333333703, 0.3219752754296894559, 0.3333333333333333703, 0.3219752754296894559, 0.3333333333333333703, 0.3219752754296894559, 0.3333333333333333703, 0.3219752754296894559, 0.3333333333333333703, 0.3219752754296894559, 0.3333333333333333703, 0.3219752754296894559, 0.3333333333333333703, 0.3219752754296894559, 0.3333333333333333703, 0.3219752754296894559, 0.3333333333333333703, 0.3219752754296894559, 0.3333333333333333703, 0.3219752754296894559, 0.3333333333333333703, 0.3219752754296894559, 0.3333333333333333703, 0.3219752754296894559, 0.3333333333333333703, 0.3219752754296894559, 0.3333333333333333703, 0.3219752754296894559, 0.3333333333333333703, 0.3219752754296894559, 0.3333333333333333703, 0.3219752754296894559, 0.3333333333333333703, 0.3219752754296894559, 0.3333333333333333703, 0.3219752754296894559, 0.3333333333333333703, 0.3219752754296894559, 0.3333333333333333703, 0.3219752754296894559, 0.3333333333333333703, 0.3219752754296894559, 0.3333333333333333703, 0.3219752754296894559, 0.3333333333333333703, 0.3219752754296894559, 0.3333333333333333703, 0.3219752754296894559, 0.3333333333333333703, 0.3219752754296894559, 0.3333333333333333703, 0.3219752754296894559, 0.3333333333333333703, 0.3219752754296894559, 0.3333333333333333703, 0.3219752754296894559, 0.3333333333333333703, 0.3219752754296894559, 0.3333333333333333703, 0.3219752754296894559, 0.3333333333333333703, 0.3219752754296894559, 0.3333333333333333703, 0.3219752754296894559, 0.3333333333333333703, 0.3219752754296894559, 0.3333333333333333703, 0.3219752754296894559, 0.3333333333333333703, 0.3219752754296894559, 0.3333333333333333703, 0.3219752754296894559, 0.3333333333333333703, 0.3219752754296894559, 0.3333333333333333703, 0.3219752754296894559, 0.3333333333333333703, 0.3219752754296894559, 0.3333333333333333703, 0.3219752754296894559, 0.3333333333333333703, 0.3219752754296894559, 0.3333333333333333703, 0.3219752754296894559, 0.3333333333333333703, 0.3219752754296894559, 0.3333333333333333703, 0.3219752754296894559, 0.3333333333333333703, 0.3219752754296894559, 0.3333333333333333703),
 ( 1.000000000000000000, 0.9659258262890683122, 1.000000000000000000, 0.9659258262890683122, 1.000000000000000000, 0.9659258262890683122, 1.000000000000000000, 0.9659258262890683122, 1.000000000000000000, 0.9659258262890683122, 1.000000000000000000, 0.9659258262890683122, 1.000000000000000000, 0.9659258262890683122, 1.000000000000000000, 0.9659258262890683122, 1.000000000000000000, 0.9659258262890683122, 1.000000000000000000, 0.9659258262890683122, 1.000000000000000000, 0.9659258262890683122, 1.000000000000000000, 0.9659258262890683122, 1.000000000000000000, 0.9659258262890683122, 1.000000000000000000, 0.9659258262890683122, 1.000000000000000000, 0.9659258262890683122, 1.000000000000000000, 0.9659258262890683122, 1.000000000000000000, 0.9659258262890683122, 1.000000000000000000, 0.9659258262890683122, 1.000000000000000000, 0.9659258262890683122, 1.000000000000000000, 0.9659258262890683122, 1.000000000000000000, 0.9659258262890683122, 1.000000000000000000, 0.9659258262890683122, 1.000000000000000000, 0.9659258262890683122, 1.000000000000000000, 0.9659258262890683122, 1.000000000000000000, 0.9659258262890683122, 1.000000000000000000, 0.9659258262890683122, 1.000000000000000000, 0.9659258262890683122, 1.000000000000000000, 0.9659258262890683122, 1.000000000000000000, 0.9659258262890683122, 1.000000000000000000, 0.9659258262890683122, 1.000000000000000000, 0.9659258262890683122, 1.000000000000000000, 0.9659258262890683122, 1.000000000000000000, 0.9659258262890683122, 1.000000000000000000, 0.9659258262890683122, 1.000000000000000000, 0.9659258262890683122, 1.000000000000000000, 0.9659258262890683122, 1.000000000000000000, 0.9659258262890683122, 1.000000000000000000, 0.9659258262890683122, 1.000000000000000000, 0.9659258262890683122, 1.000000000000000000, 0.9659258262890683122, 1.000000000000000000, 0.9659258262890683122, 1.000000000000000000, 0.9659258262890683122, 1.000000000000000000, 0.9659258262890683122, 1.000000000000000000, 0.9659258262890683122, 1.000000000000000000, 0.9659258262890683122, 1.000000000000000000, 0.9659258262890683122, 1.000000000000000000, 0.9659258262890683122, 1.000000000000000000, 0.9659258262890683122, 1.000000000000000000, 0.9659258262890683122, 1.000000000000000000, 0.9659258262890683122, 1.000000000000000000, 0.9659258262890683122, 1.000000000000000000, 0.9659258262890683122, 1.000000000000000000, 0.9659258262890683122, 1.000000000000000000, 0.9659258262890683122, 1.000000000000000000, 0.9659258262890683122, 1.000000000000000000, 0.9659258262890683122, 1.000000000000000000, 0.9659258262890683122, 1.000000000000000000, 0.9659258262890683122, 1.000000000000000000, 0.9659258262890683122, 1.000000000000000000, 0.9659258262890683122, 1.000000000000000000, 0.9659258262890683122, 1.000000000000000000, 0.9659258262890683122, 1.000000000000000000, 0.9659258262890683122, 1.000000000000000000, 0.9659258262890683122, 1.000000000000000000, 0.9659258262890683122, 1.000000000000000000, 0.9659258262890683122, 1.000000000000000000, 0.9659258262890683122, 1.000000000000000000, 0.9659258262890683122, 1.000000000000000000, 0.9659258262890683122, 1.000000000000000000, 0.9659258262890683122, 1.000000000000000000, 0.9659258262890683122, 1.000000000000000000, 0.9659258262890683122, 1.000000000000000000, 0.9659258262890683122, 1.000000000000000000, 0.9659258262890683122, 1.000000000000000000, 0.9659258262890683122, 1.000000000000000000, 0.9659258262890683122, 1.000000000000000000, 0.9659258262890683122, 1.000000000000000000, 0.9659258262890683122, 1.000000000000000000, 0.9659258262890683122, 1.000000000000000000, 0.9659258262890683122, 1.000000000000000000, 0.9659258262890683122, 1.000000000000000000, 0.9659258262890683122, 1.000000000000000000, 0.9659258262890683122, 1.000000000000000000, 0.9659258262890683122, 1.000000000000000000, 0.9659258262890683122, 1.000000000000000000, 0.9659258262890683122, 1.000000000000000000, 0.9659258262890683122, 1.000000000000000000, 0.9659258262890683122, 1.000000000000000000, 0.9659258262890683122, 1.000000000000000000, 0.9659258262890683122, 1.000000000000000000, 0.9659258262890683122, 1.000000000000000000, 0.9659258262890683122, 1.000000000000000000, 0.9659258262890683122, 1.000000000000000000, 0.9659258262890683122, 1.000000000000000000, 0.9659258262890683122, 1.000000000000000000, 0.9659258262890683122, 1.000000000000000000, 0.9659258262890683122, 1.000000000000000000, 0.9659258262890683122, 1.000000000000000000, 0.9659258262890683122, 1.000000000000000000, 0.9659258262890683122, 1.000000000000000000, 0.9659258262890683122, 1.000000000000000000, 0.9659258262890683122, 1.000000000000000000, 0.9659258262890683122, 1.000000000000000000, 0.9659258262890683122, 1.000000000000000000, 0.9659258262890683122, 1.000000000000000000, 0.9659258262890683122, 1.000000000000000000, 0.9659258262890683122, 1.000000000000000000, 0.9659258262890683122, 1.000000000000000000, 0.9659258262890683122, 1.000000000000000000, 0.9659258262890683122, 1.000000000000000000, 0.9659258262890683122, 1.000000000000000000, 0.9659258262890683122, 1.000000000000000000, 0.9659258262890683122, 1.000000000000000000, 0.9659258262890683122, 1.000000000000000000, 0.9659258262890683122, 1.000000000000000000, 0.9659258262890683122, 1.000000000000000000, 0.9659258262890683122, 1.000000000000000000, 0.9659258262890683122, 1.000000000000000000, 0.9659258262890683122, 1.000000000000000000, 0.9659258262890683122, 1.000000000000000000, 0.9659258262890683122, 1.000000000000000000, 0.9659258262890683122, 1.000000000000000000, 0.9659258262890683122, 1.000000000000000000, 0.9659258262890683122, 1.000000000000000000, 0.9659258262890683122, 1.000000000000000000, 0.9659258262890683122, 1.000000000000000000, 0.9659258262890683122, 1.000000000000000000, 0.9659258262890683122, 1.000000000000000000, 0.9659258262890683122, 1.000000000000000000, 0.9659258262890683122, 1.000000000000000000, 0.9659258262890683122, 1.000000000000000000, 0.9659258262890683122, 1.000000000000000000, 0.9659258262890683122, 1.000000000000000000, 0.9659258262890683122, 1.000000000000000000, 0.9659258262890683122, 1.000000000000000000, 0.9659258262890683122, 1.000000000000000000, 0.9659258262890683122, 1.000000000000000000, 0.9659258262890683122, 1.000000000000000000, 0.9659258262890683122, 1.000000000000000000, 0.9659258262890683122, 1.000000000000000000, 0.9659258262890683122, 1.000000000000000000, 0.9659258262890683122, 1.000000000000000000, 0.9659258262890683122, 1.000000000000000000, 0.9659258262890683122, 1.000000000000000000, 0.9659258262890683122, 1.000000000000000000, 0.9659258262890683122, 1.000000000000000000, 0.9659258262890683122, 1.000000000000000000, 0.9659258262890683122, 1.000000000000000000, 0.9659258262890683122, 1.000000000000000000, 0.9659258262890683122, 1.000000000000000000, 0.9659258262890683122, 1.000000000000000000, 0.9659258262890683122, 1.000000000000000000, 0.9659258262890683122, 1.000000000000000000, 0.9659258262890683122, 1.000000000000000000, 0.9659258262890683122, 1.000000000000000000, 0.9659258262890683122, 1.000000000000000000, 0.9659258262890683122, 1.000000000000000000, 0.9659258262890683122, 1.000000000000000000, 0.9659258262890683122, 1.000000000000000000, 0.9659258262890683122, 1.000000000000000000, 0.9659258262890683122, 1.000000000000000000, 0.9659258262890683122, 1.000000000000000000, 0.9659258262890683122, 1.000000000000000000, 0.9659258262890683122, 1.000000000000000000, 0.9659258262890683122, 1.000000000000000000, 0.9659258262890683122, 1.000000000000000000, 0.9659258262890683122, 1.000000000000000000, 0.9659258262890683122, 1.000000000000000000, 0.9659258262890683122, 1.000000000000000000, 0.9659258262890683122, 1.000000000000000000, 0.9659258262890683122, 1.000000000000000000, 0.9659258262890683122, 1.000000000000000000, 0.9659258262890683122, 1.000000000000000000, 0.9659258262890683122, 1.000000000000000000, 0.9659258262890683122, 1.000000000000000000, 0.9659258262890683122, 1.000000000000000000, 0.9659258262890683122, 1.000000000000000000, 0.9659258262890683122, 1.000000000000000000, 0.9659258262890683122, 1.000000000000000000, 0.9659258262890683122, 1.000000000000000000, 0.9659258262890683122, 1.000000000000000000, 0.9659258262890683122, 1.000000000000000000, 0.9659258262890683122, 1.000000000000000000, 0.9659258262890683122, 1.000000000000000000, 0.9659258262890683122, 1.000000000000000000, 0.9659258262890683122, 1.000000000000000000, 0.9659258262890683122, 1.000000000000000000, 0.9659258262890683122, 1.000000000000000000, 0.9659258262890683122, 1.000000000000000000, 0.9659258262890683122, 1.000000000000000000, 0.9659258262890683122, 1.000000000000000000, 0.9659258262890683122, 1.000000000000000000) ) ) 
 REPRESENTATION_ITEM ( '' )  SURFACE ( )  );
#6401 = CARTESIAN_POINT ( 'NONE',  ( 10.04305231718579705, 62.59999999999998721, 30.90933677959248982 ) ) ;
#6402 = CARTESIAN_POINT ( 'NONE',  ( -20.75514604977248823, 21.07500000273118346, -28.56700777964554305 ) ) ;
#6403 = CARTESIAN_POINT ( 'NONE',  ( 2.375766604868046361, 76.55125428154684641, 14.99999999999999822 ) ) ;
#6404 = CARTESIAN_POINT ( 'NONE',  ( 15.04653450569339945, 67.42409749907601224, 25.98046417659831775 ) ) ;
#6405 = CARTESIAN_POINT ( 'NONE',  ( -8.601468415847518756, 72.57500000273117280, -11.83890561707634781 ) ) ;
#6406 = CYLINDRICAL_SURFACE ( 'NONE', #18984, 32.50000000000000000 ) ;
#6407 = DIRECTION ( 'NONE',  ( -1.224646799147353207E-16, -1.499759782661857882E-32, 1.000000000000000000 ) ) ;
#6408 = EDGE_CURVE ( 'NONE', #10494, #28763, #6262, .T. ) ;
#6409 = VECTOR ( 'NONE', #31627, 1000.000000000000000 ) ;
#6410 = CARTESIAN_POINT ( 'NONE',  ( 26.29305231718579350, 8.800000000000016698, 19.10302069950537529 ) ) ;
#6411 = VERTEX_POINT ( 'NONE', #5387 ) ;
#6412 = CARTESIAN_POINT ( 'NONE',  ( -23.41746825000000598, 8.224999997268824359, 7.608796670333726198 ) ) ;
#6413 = DIRECTION ( 'NONE',  ( 0.000000000000000000, 1.000000000000000000, 0.000000000000000000 ) ) ;
#6414 = CARTESIAN_POINT ( 'NONE',  ( 19.09188309203661049, 40.35937499999999289, -19.09188309203694445 ) ) ;
#6415 = CARTESIAN_POINT ( 'NONE',  ( 27.16883889988623935, 16.32500000273118346, -19.73931689729374384 ) ) ;
#6416 = CARTESIAN_POINT ( 'NONE',  ( 33.58253175000000113, 64.22500000273117848, -10.91162601494193751 ) ) ;
#6417 = CARTESIAN_POINT ( 'NONE',  ( 27.16883889988624290, 28.17500000273119554, 19.73931689729373673 ) ) ;
#6418 = CARTESIAN_POINT ( 'NONE',  ( -27.16883889988623935, 17.57500000273119767, 19.73931689729374739 ) ) ;
#6419 = CARTESIAN_POINT ( 'NONE',  ( 33.58253175000000823, 10.27500000273117386, 10.91162601494192685 ) ) ;
#6420 = CARTESIAN_POINT ( 'NONE',  ( 25.98046417659858420, 15.01340250092397888, 15.04653450569292872 ) ) ;
#6421 = EDGE_CURVE ( 'NONE', #18399, #21929, #11969, .T. ) ;
#6422 = CARTESIAN_POINT ( 'NONE',  ( 20.50609665441005092, 54.96875000000000000, 20.50609665440969209 ) ) ;
#6423 = CARTESIAN_POINT ( 'NONE',  ( 3.880418787951102289, 16.44874571845315359, -24.50000000000000711 ) ) ;
#6424 = CARTESIAN_POINT ( 'NONE',  ( -8.960552108402744065E-16, 74.87500000273116996, -14.63369212191046209 ) ) ;
#6425 = CARTESIAN_POINT ( 'NONE',  ( -32.50000000000000000, 45.89999999999999858, -10.55989012756945478 ) ) ;
#6426 = CARTESIAN_POINT ( 'NONE',  ( -33.58253175000000113, 49.22500000273119269, 10.91162601494193929 ) ) ;
#6427 = CARTESIAN_POINT ( 'NONE',  ( 23.41746824999999887, 4.624999997268814056, 0.000000000000000000 ) ) ;
#6428 = ADVANCED_FACE ( 'NONE', ( #21682 ), #24253, .F. ) ;
#6429 = ORIENTED_EDGE ( 'NONE', *, *, #3604, .T. ) ;
#6430 = CARTESIAN_POINT ( 'NONE',  ( 33.58253175000000113, 60.47500000273118559, -10.91162601494193751 ) ) ;
#6431 = CARTESIAN_POINT ( 'NONE',  ( -26.29305231718578995, 2.199999999999979750, 19.10302069950538595 ) ) ;
#6432 = CARTESIAN_POINT ( 'NONE',  ( -7.236395654485763274, 6.024999997268825958, 22.27133577429736633 ) ) ;
#6433 = CARTESIAN_POINT ( 'NONE',  ( -0.04044903254992426173, 22.46131916759064850, 27.95245687107223276 ) ) ;
#6434 = EDGE_LOOP ( 'NONE', ( #972, #26025, #15008, #11207 ) ) ;
#6435 = AXIS2_PLACEMENT_3D ( 'NONE', #4623, #25733, #12862 ) ;
#6436 = CARTESIAN_POINT ( 'NONE',  ( 27.16883889988623935, 34.32500000273118701, -19.73931689729374384 ) ) ;
#6437 = DIRECTION ( 'NONE',  ( -1.000000000000000000, -1.224646799147353454E-16, 0.000000000000000000 ) ) ;
#6438 = ORIENTED_EDGE ( 'NONE', *, *, #16640, .F. ) ;
#6439 = CARTESIAN_POINT ( 'NONE',  ( -15.01150461594595775, 48.80989583333332860, 26.00068869287368756 ) ) ;
#6440 = CARTESIAN_POINT ( 'NONE',  ( 10.37757302488624767, 57.97500000273119980, 31.93888565452638417 ) ) ;
#6441 = CARTESIAN_POINT ( 'NONE',  ( 15.00000000000000355, 75.15000000546237402, 4.873795443493592394 ) ) ;
#6442 = CARTESIAN_POINT ( 'NONE',  ( 27.16883889988623935, 72.32500000273117280, -19.73931689729374384 ) ) ;
#6443 = CARTESIAN_POINT ( 'NONE',  ( 15.01150461594596308, 29.90364583333332504, -26.00068869287367335 ) ) ;
#6444 = CARTESIAN_POINT ( 'NONE',  ( -7.570916362186215665, 3.400000000000014122, 23.30088464923126423 ) ) ;
#6445 = CARTESIAN_POINT ( 'NONE',  ( -27.16883889988623935, 1.575000002731197224, 19.73931689729374739 ) ) ;
#6446 = CARTESIAN_POINT ( 'NONE',  ( -27.16883889988624290, 14.92500000273117067, -19.73931689729374028 ) ) ;
#6447 = CARTESIAN_POINT ( 'NONE',  ( -4.300734207923755825, 75.27500000273118985, 13.23629886949340673 ) ) ;
#6448 = CARTESIAN_POINT ( 'NONE',  ( 25.98046417659831775, 42.50222249907603356, -15.04653450569338879 ) ) ;
#6449 = CARTESIAN_POINT ( 'NONE',  ( 11.25946833292375793, 72.17500000273119554, 8.180482586598731842 ) ) ;
#6450 = CARTESIAN_POINT ( 'NONE',  ( -2.584737979205442066E-13, 57.11718750000000711, -30.02300923189239867 ) ) ;
#6451 = CARTESIAN_POINT ( 'NONE',  ( 0.000000000000000000, 16.99999999999998579, 0.000000000000000000 ) ) ;
#6452 = CARTESIAN_POINT ( 'NONE',  ( 7.570916362186207671, 5.349999994537641079, 23.30088464923126779 ) ) ;
#6453 = FACE_OUTER_BOUND ( 'NONE', #15705, .T. ) ;
#6454 = CARTESIAN_POINT ( 'NONE',  ( 7.025853678916867295, 67.56732666574268364, 26.06988505166722803 ) ) ;
#6455 = CARTESIAN_POINT ( 'NONE',  ( -33.58253175000000113, 39.12500000273119838, 0.000000000000000000 ) ) ;
#6456 = CARTESIAN_POINT ( 'NONE',  ( 2.688165632520823219E-15, 77.37500000273118417, 14.63369212191046387 ) ) ;
#6457 = CARTESIAN_POINT ( 'NONE',  ( 20.75514604977248467, 48.67500000273117422, -28.56700777964554305 ) ) ;
#6458 = CARTESIAN_POINT ( 'NONE',  ( 6.486482029760648627E-15, 29.87500000273119483, 35.31076352940722529 ) ) ;
#6459 = CARTESIAN_POINT ( 'NONE',  ( 0.5672726147806251840, 16.99999999999999289, 24.06736868777154470 ) ) ;
#6460 = CARTESIAN_POINT ( 'NONE',  ( -24.20753774853730889, 35.34635416666666430, 13.97622843553634020 ) ) ;
#6461 = CARTESIAN_POINT ( 'NONE',  ( -15.14183272437242067, 14.44999999453762207, -20.84094480462497856 ) ) ;
#6462 = CIRCLE ( 'NONE', #9190, 13.38432950954957157 ) ;
#6463 = DIRECTION ( 'NONE',  ( 0.000000000000000000, -1.000000000000000000, 0.000000000000000000 ) ) ;
#6464 = CARTESIAN_POINT ( 'NONE',  ( -2.092463501923844636E-15, 69.49999999999997158, -34.17252228774368916 ) ) ;
#6465 = CARTESIAN_POINT ( 'NONE',  ( -14.47279130897152299, 7.924999997268802332, 19.92008829642072243 ) ) ;
#6466 = CARTESIAN_POINT ( 'NONE',  ( -25.98046417659831420, 23.59597249907602290, 15.04653450569339945 ) ) ;
#6467 =( BOUNDED_CURVE ( )  B_SPLINE_CURVE ( 2, ( #6025, #3956, #16503, #19414, #19747, #6191, #11676, #14097, #700, #26956, #3790, #13927, #19582 ),
 .UNSPECIFIED., .F., .T. ) 
 B_SPLINE_CURVE_WITH_KNOTS ( ( 3, 2, 2, 2, 2, 2, 3 ),
 ( 0.8525641025641025328, 0.8538461538461538103, 0.8564102564102563653, 0.8589743589743589203, 0.8615384615384615863, 0.8641025641025641413, 0.8653846153846154188 ),
 .UNSPECIFIED. ) 
 CURVE ( )  GEOMETRIC_REPRESENTATION_ITEM ( )  RATIONAL_B_SPLINE_CURVE ( ( 0.9755282581475768211, 0.9755282581475768211, 1.000000000000000000, 0.9510565162951535312, 1.000000000000000000, 0.9510565162951535312, 1.000000000000000000, 0.9510565162951535312, 1.000000000000000000, 0.9510565162951535312, 1.000000000000000000, 0.9755282581475768211, 0.9755282581475768211 ) ) 
 REPRESENTATION_ITEM ( '' )  );
#6468 = DIRECTION ( 'NONE',  ( 0.000000000000000000, 0.000000000000000000, -1.000000000000000000 ) ) ;
#6469 = CARTESIAN_POINT ( 'NONE',  ( 6.950374756619257965, 38.63503499907601224, -26.09010956794244507 ) ) ;
#6470 = CARTESIAN_POINT ( 'NONE',  ( -7.570916362186210335, 12.59999999999999964, -23.30088464923126779 ) ) ;
#6471 =( BOUNDED_CURVE ( )  B_SPLINE_CURVE ( 2, ( #31135, #10376, #10544, #23423, #28893, #2307, #7965, #10713, #12780, #23075, #28221, #7626, #5396 ),
 .UNSPECIFIED., .F., .T. ) 
 B_SPLINE_CURVE_WITH_KNOTS ( ( 3, 2, 2, 2, 2, 2, 3 ),
 ( 0.6217948717948718063, 0.6230769230769230838, 0.6256410256410256387, 0.6282051282051281937, 0.6307692307692307487, 0.6333333333333333037, 0.6346153846153845812 ),
 .UNSPECIFIED. ) 
 CURVE ( )  GEOMETRIC_REPRESENTATION_ITEM ( )  RATIONAL_B_SPLINE_CURVE ( ( 0.9755282581475768211, 0.9755282581475768211, 1.000000000000000000, 0.9510565162951535312, 1.000000000000000000, 0.9510565162951535312, 1.000000000000000000, 0.9510565162951535312, 1.000000000000000000, 0.9510565162951535312, 1.000000000000000000, 0.9755282581475768211, 0.9755282581475768211 ) ) 
 REPRESENTATION_ITEM ( '' )  );
#6472 = CARTESIAN_POINT ( 'NONE',  ( 10.37757302488624056, 12.52500000273118452, -31.93888565452638417 ) ) ;
#6473 = CARTESIAN_POINT ( 'NONE',  ( 14.47279130897151589, 6.824999997268808904, 19.92008829642072953 ) ) ;
#6474 = CARTESIAN_POINT ( 'NONE',  ( -2.428612866367529427E-13, 50.24218750000000711, -27.95245687107222921 ) ) ;
#6475 = ORIENTED_EDGE ( 'NONE', *, *, #17076, .T. ) ;
#6476 = CARTESIAN_POINT ( 'NONE',  ( -33.58253175000000113, 59.12500000273116996, 0.000000000000000000 ) ) ;
#6477 = CARTESIAN_POINT ( 'NONE',  ( -20.75514604977248112, 31.67500000273119909, 28.56700777964554661 ) ) ;
#6478 = ORIENTED_EDGE ( 'NONE', *, *, #423, .F. ) ;
#6479 = CARTESIAN_POINT ( 'NONE',  ( 30.02300923189239512, 20.16406249999999645, -2.619432448724977703E-13 ) ) ;
#6480 = CARTESIAN_POINT ( 'NONE',  ( 20.53372385742072481, 24.60975666759063785, -20.47846945139902175 ) ) ;
#6481 = CARTESIAN_POINT ( 'NONE',  ( 15.14183272437242422, 16.04999999453762882, -20.84094480462497856 ) ) ;
#6482 = CARTESIAN_POINT ( 'NONE',  ( -7.570916362186210335, 16.34999999453762243, -23.30088464923126779 ) ) ;
#6483 = CARTESIAN_POINT ( 'NONE',  ( 18.94512977948575738, 4.424999997268807661, 13.76444248337723408 ) ) ;
#6484 = CARTESIAN_POINT ( 'NONE',  ( -10.37757302488624411, 22.97500000273117138, -31.93888565452638417 ) ) ;
#6485 = CARTESIAN_POINT ( 'NONE',  ( -20.08610463437157989, 30.20000000546236407, -27.64615127144129758 ) ) ;
#6486 = CARTESIAN_POINT ( 'NONE',  ( 10.04305231718578817, 73.40000000000001990, -30.90933677959249337 ) ) ;
#6487 = CARTESIAN_POINT ( 'NONE',  ( 20.08610463437157279, 37.80000000546237970, -27.64615127144129758 ) ) ;
#6488 = CARTESIAN_POINT ( 'NONE',  ( -20.47846945139902175, 54.68788166759063785, -20.53372385742072481 ) ) ;
#6489 = CARTESIAN_POINT ( 'NONE',  ( 20.75514604977249178, 34.07500000273117990, 28.56700777964553950 ) ) ;
#6490 = CARTESIAN_POINT ( 'NONE',  ( -20.75514604977248823, 52.82500000273116569, -28.56700777964554305 ) ) ;
#6491 = CARTESIAN_POINT ( 'NONE',  ( -28.01184896238290278, 32.05208333333332860, 7.505752307973363457 ) ) ;
#6492 = CARTESIAN_POINT ( 'NONE',  ( -4.523095164977116484E-15, 10.62499999726880695, 24.62258325217400312 ) ) ;
#6493 = CARTESIAN_POINT ( 'NONE',  ( 32.50000000000000711, 14.89999999999999680, 10.55989012756945122 ) ) ;
#6494 = CARTESIAN_POINT ( 'NONE',  ( -24.50000000000001066, 13.09999999999999432, 7.960532557706201828 ) ) ;
#6495 = CARTESIAN_POINT ( 'NONE',  ( -24.18731323226221974, 47.65847249907603356, 14.01125832528330406 ) ) ;
#6496 = CARTESIAN_POINT ( 'NONE',  ( 20.75514604977249178, 53.82500000273119412, 28.56700777964553950 ) ) ;
#6497 = CARTESIAN_POINT ( 'NONE',  ( 10.37757302488624056, 44.77500000273118275, -31.93888565452638417 ) ) ;
#6498 = CARTESIAN_POINT ( 'NONE',  ( -23.41746824999999887, 7.624999997268816720, -2.867812753649727150E-15 ) ) ;
#6499 = FACE_OUTER_BOUND ( 'NONE', #27494, .T. ) ;
#6500 = CARTESIAN_POINT ( 'NONE',  ( -20.75514604977248823, 2.825000002731177240, -28.56700777964554305 ) ) ;
#6501 = CARTESIAN_POINT ( 'NONE',  ( 19.06425588902592239, 35.78163166759063074, 19.11951029504763611 ) ) ;
#6502 = CARTESIAN_POINT ( 'NONE',  ( 0.000000000000000000, 66.99999999999998579, 0.000000000000000000 ) ) ;
#6503 = CYLINDRICAL_SURFACE ( 'NONE', #17697, 15.00000000000000000 ) ;
#6504 = PRODUCT_DEFINITION_CONTEXT ( 'detailed design', #21934, 'design' ) ;
#6505 = CARTESIAN_POINT ( 'NONE',  ( -33.58253175000000113, 25.22500000273119625, 10.91162601494193929 ) ) ;
#6506 = CARTESIAN_POINT ( 'NONE',  ( 1.836970198721029589E-15, 82.00000000000001421, 15.00000000000000000 ) ) ;
#6507 = FACE_BOUND ( 'NONE', #30305, .T. ) ;
#6508 = CARTESIAN_POINT ( 'NONE',  ( 1.555960095263670572E-15, 14.50000000000000178, -24.50000000000000000 ) ) ;
#6509 = CARTESIAN_POINT ( 'NONE',  ( 25.98046417659831775, 52.81472249907603356, -15.04653450569338879 ) ) ;
#6510 = CARTESIAN_POINT ( 'NONE',  ( 32.50000000000000000, 49.60000000546239818, -10.55989012756945833 ) ) ;
#6511 = EDGE_CURVE ( 'NONE', #27108, #9001, #6046, .T. ) ;
#6512 = CARTESIAN_POINT ( 'NONE',  ( -26.29305231718579350, 58.30000000546238681, -19.10302069950537884 ) ) ;
#6513 = CARTESIAN_POINT ( 'NONE',  ( 33.58253175000000113, 34.12500000273119127, -4.112674001490185761E-15 ) ) ;
#6514 = CARTESIAN_POINT ( 'NONE',  ( -13.97622843553632421, 29.33072916666665719, -24.20753774853731599 ) ) ;
#6515 = EDGE_CURVE ( 'NONE', #22342, #16741, #2810, .T. ) ;
#6516 = CARTESIAN_POINT ( 'NONE',  ( -27.16883889988624290, 74.92500000273120975, -19.73931689729374028 ) ) ;
#6517 = CARTESIAN_POINT ( 'NONE',  ( 15.01150461594643204, 31.04947916666666075, 26.00068869287340334 ) ) ;
#6518 = LINE ( 'NONE', #16989, #8055 ) ;
#6519 = EDGE_LOOP ( 'NONE', ( #27199, #16947, #2106, #17327 ) ) ;
#6520 = CARTESIAN_POINT ( 'NONE',  ( 26.02091320914851025, 45.37798583425732346, -14.97647472619946463 ) ) ;
#6521 = CARTESIAN_POINT ( 'NONE',  ( 20.08610463437157279, 11.80000000546236194, -27.64615127144129758 ) ) ;
#6522 = CARTESIAN_POINT ( 'NONE',  ( 20.50609665440969565, 64.42187499999998579, -20.50609665441004736 ) ) ;
#6523 = CARTESIAN_POINT ( 'NONE',  ( 26.29305231718578995, 21.19999999999999574, -19.10302069950538240 ) ) ;
#6524 = CARTESIAN_POINT ( 'NONE',  ( 33.58253175000000823, 40.27500000273118985, 10.91162601494192863 ) ) ;
#6525 = CARTESIAN_POINT ( 'NONE',  ( -10.04305231718579172, 48.10000000546238397, -30.90933677959248982 ) ) ;
#6526 = CARTESIAN_POINT ( 'NONE',  ( -11.25946833292375793, 75.17500000273119554, -8.180482586598733619 ) ) ;
#6527 = CARTESIAN_POINT ( 'NONE',  ( 10.37757302488624056, 28.52500000273120051, -31.93888565452638417 ) ) ;
#6528 = LINE ( 'NONE', #11839, #28560 ) ;
#6529 = CARTESIAN_POINT ( 'NONE',  ( 33.58253175000000113, 54.47500000273117138, -10.91162601494193751 ) ) ;
#6530 =( LENGTH_UNIT ( ) NAMED_UNIT ( * ) SI_UNIT ( .MILLI., .METRE. ) );
#6531 = CARTESIAN_POINT ( 'NONE',  ( -20.08610463437157989, 37.70000000000000995, -27.64615127144129758 ) ) ;
#6532 = CARTESIAN_POINT ( 'NONE',  ( -10.04305231718578462, 36.39999999999999147, 30.90933677959249337 ) ) ;
#6533 = CARTESIAN_POINT ( 'NONE',  ( 7.236395654485760609, 9.024999997268828622, -22.27133577429736633 ) ) ;
#6534 = CARTESIAN_POINT ( 'NONE',  ( -20.75514604977248823, 74.82500000273115859, -28.56700777964554305 ) ) ;
#6535 = CARTESIAN_POINT ( 'NONE',  ( 0.000000000000000000, 80.00000000000001421, 0.000000000000000000 ) ) ;
#6536 = CARTESIAN_POINT ( 'NONE',  ( 8.601468415847520532, 78.07500000273121543, 11.83890561707634603 ) ) ;
#6537 = CARTESIAN_POINT ( 'NONE',  ( 10.37757302488624767, 65.97500000273120691, 31.93888565452638417 ) ) ;
#6538 = CARTESIAN_POINT ( 'NONE',  ( -15.14183272437242778, 5.300000000000006040, 20.84094480462497856 ) ) ;
#6539 = ORIENTED_EDGE ( 'NONE', *, *, #16824, .F. ) ;
#6540 = CARTESIAN_POINT ( 'NONE',  ( 1.577395562988744260E-15, 2.249999994537629444, -25.76082449383753925 ) ) ;
#6541 = CARTESIAN_POINT ( 'NONE',  ( -26.06988505166735237, 13.15142333425730925, -7.025853678916388567 ) ) ;
#6542 = CARTESIAN_POINT ( 'NONE',  ( -19.09188309203694445, 67.00000000000000000, -19.09188309203661049 ) ) ;
#6543 = CARTESIAN_POINT ( 'NONE',  ( 6.486482029760649416E-15, 49.62500000273117706, 35.31076352940723240 ) ) ;
#6544 = CARTESIAN_POINT ( 'NONE',  ( 10.37757302488624056, 4.775000002731191628, -31.93888565452638417 ) ) ;
#6545 = CARTESIAN_POINT ( 'NONE',  ( -33.58253175000000113, 59.47500000273119269, 10.91162601494193929 ) ) ;
#6546 = CARTESIAN_POINT ( 'NONE',  ( 26.07999730980477437, 50.95833333333332860, -6.988114217768290004 ) ) ;
#6547 = CARTESIAN_POINT ( 'NONE',  ( -28.02196122052045268, 36.92746500092395934, 7.468012846824790607 ) ) ;
#6548 = CARTESIAN_POINT ( 'NONE',  ( 14.97647472619900455, 31.90326416574268364, -26.02091320914876960 ) ) ;
#6549 = CARTESIAN_POINT ( 'NONE',  ( 32.50000000000000000, 69.60000000546236265, -10.55989012756945833 ) ) ;
#6550 = CARTESIAN_POINT ( 'NONE',  ( 4.300734207923761154, 79.47500000273116427, 13.23629886949340495 ) ) ;
#6551 = CARTESIAN_POINT ( 'NONE',  ( -26.09010956794245217, 51.52565999907602645, -6.950374756619243755 ) ) ;
#6552 = DIRECTION ( 'NONE',  ( 0.000000000000000000, 0.000000000000000000, 1.000000000000000000 ) ) ;
#6553 = ORIENTED_EDGE ( 'NONE', *, *, #427, .F. ) ;
#6554 = CARTESIAN_POINT ( 'NONE',  ( 10.37757302488624056, 38.77500000273119696, -31.93888565452638417 ) ) ;
#6555 = CARTESIAN_POINT ( 'NONE',  ( -26.29305231718578995, 76.19999999999998863, 19.10302069950538595 ) ) ;
#6556 = CARTESIAN_POINT ( 'NONE',  ( 32.50000000000000000, 27.60000000546238752, -10.55989012756945833 ) ) ;
#6557 = ORIENTED_EDGE ( 'NONE', *, *, #12835, .T. ) ;
#6558 = CARTESIAN_POINT ( 'NONE',  ( 20.50609665441005092, 34.34374999999999289, 20.50609665440969209 ) ) ;
#6559 = VERTEX_POINT ( 'NONE', #13950 ) ;
#6560 =( BOUNDED_CURVE ( )  B_SPLINE_CURVE ( 2, ( #28288, #23490, #5119, #28621, #33605, #12670, #28793, #20583, #10103, #15253, #31368, #2719, #25714 ),
 .UNSPECIFIED., .F., .T. ) 
 B_SPLINE_CURVE_WITH_KNOTS ( ( 3, 2, 2, 2, 2, 2, 3 ),
 ( 0.9294871794871795156, 0.9307692307692307931, 0.9333333333333333481, 0.9358974358974359031, 0.9384615384615384581, 0.9410256410256410131, 0.9423076923076922906 ),
 .UNSPECIFIED. ) 
 CURVE ( )  GEOMETRIC_REPRESENTATION_ITEM ( )  RATIONAL_B_SPLINE_CURVE ( ( 0.9755282581475768211, 0.9755282581475768211, 1.000000000000000000, 0.9510565162951535312, 1.000000000000000000, 0.9510565162951535312, 1.000000000000000000, 0.9510565162951535312, 1.000000000000000000, 0.9510565162951535312, 1.000000000000000000, 0.9755282581475768211, 0.9755282581475768211 ) ) 
 REPRESENTATION_ITEM ( '' )  );
#6561 = CARTESIAN_POINT ( 'NONE',  ( -5.147494310547423346, 56.44874571845314648, 32.50000000000000000 ) ) ;
#6562 = CARTESIAN_POINT ( 'NONE',  ( 20.75514604977248467, 50.42500000273118843, -28.56700777964554305 ) ) ;
#6563 = CARTESIAN_POINT ( 'NONE',  ( 7.505752307972854531, 60.69791666666667140, -28.01184896238303423 ) ) ;
#6564 = EDGE_CURVE ( 'NONE', #9414, #22980, #24018, .T. ) ;
#6565 = CARTESIAN_POINT ( 'NONE',  ( -32.50000000000000000, 14.50000000546236478, 0.000000000000000000 ) ) ;
#6566 = CARTESIAN_POINT ( 'NONE',  ( -4.635254915624208216, 78.39999999999999147, 14.26584774442730463 ) ) ;
#6567 = CARTESIAN_POINT ( 'NONE',  ( 14.47279130897151944, 13.42499999726880411, -19.92008829642072598 ) ) ;
#6568 = CARTESIAN_POINT ( 'NONE',  ( 26.29305231718579350, 52.80000000000001137, 19.10302069950537529 ) ) ;
#6569 = CARTESIAN_POINT ( 'NONE',  ( 33.58253175000000823, 26.27500000273119340, 10.91162601494192863 ) ) ;
#6570 = CARTESIAN_POINT ( 'NONE',  ( 3.980102097228898626E-15, 80.00000000000001421, 32.50000000000000000 ) ) ;
#6571 = CARTESIAN_POINT ( 'NONE',  ( 14.01125832528330051, 19.29909749907602290, 24.18731323226221974 ) ) ;
#6572 = CARTESIAN_POINT ( 'NONE',  ( 4.300734207923761154, 73.47500000273119269, 13.23629886949340495 ) ) ;
#6573 = CARTESIAN_POINT ( 'NONE',  ( 15.00000000000000000, 75.35000000546239107, -4.873795443493596835 ) ) ;
#6574 = CARTESIAN_POINT ( 'NONE',  ( -7.347880794884122694E-16, -16.99999999999999645, 0.000000000000000000 ) ) ;
#6575 = CARTESIAN_POINT ( 'NONE',  ( 26.29305231718578995, 5.199999999999996625, -19.10302069950538240 ) ) ;
#6576 = EDGE_LOOP ( 'NONE', ( #31124, #2559, #1773, #1439 ) ) ;
#6577 = CARTESIAN_POINT ( 'NONE',  ( -23.41746825000000243, 8.024999997268801977, -7.608796670333730638 ) ) ;
#6578 = CARTESIAN_POINT ( 'NONE',  ( 2.688165632520823219E-15, 71.37500000273119838, 14.63369212191046387 ) ) ;
#6579 = CARTESIAN_POINT ( 'NONE',  ( 6.988114217767829928, 43.51041666666666430, -26.07999730980489872 ) ) ;
#6580 = CARTESIAN_POINT ( 'NONE',  ( 27.16883889988624290, 65.92500000273119554, 19.73931689729373673 ) ) ;
#6581 = CARTESIAN_POINT ( 'NONE',  ( -2.162160676586881955E-15, 32.87500000273118417, -35.31076352940723240 ) ) ;
#6582 = CARTESIAN_POINT ( 'NONE',  ( -20.75514604977248112, 19.67500000273119909, 28.56700777964554661 ) ) ;
#6583 = CARTESIAN_POINT ( 'NONE',  ( -10.37757302488623701, 11.77500000273118452, 31.93888565452638417 ) ) ;
#6584 = CARTESIAN_POINT ( 'NONE',  ( 26.02091320914851025, 11.00298583425731103, -14.97647472619946463 ) ) ;
#6585 = CARTESIAN_POINT ( 'NONE',  ( -20.50609665440969209, 55.82812499999999289, 20.50609665441005092 ) ) ;
#6586 = CARTESIAN_POINT ( 'NONE',  ( 8.601468415847516980, 76.67500000273116711, -11.83890561707634603 ) ) ;
#6587 = CARTESIAN_POINT ( 'NONE',  ( -26.29305231718579350, 47.79999999999999716, -19.10302069950537884 ) ) ;
#6588 = CARTESIAN_POINT ( 'NONE',  ( 24.50000000000000000, 7.649999994537632908, 7.960532557706212486 ) ) ;
#6589 = CARTESIAN_POINT ( 'NONE',  ( 6.486482029760648627E-15, 49.62500000273117706, 35.31076352940722529 ) ) ;
#6590 = CARTESIAN_POINT ( 'NONE',  ( -14.47279130897151589, 5.324999997268826668, -19.92008829642072598 ) ) ;
#6591 = ORIENTED_EDGE ( 'NONE', *, *, #11041, .F. ) ;
#6592 = CARTESIAN_POINT ( 'NONE',  ( 33.58253175000000113, 62.37500000273120548, -4.112674001490185761E-15 ) ) ;
#6593 = CARTESIAN_POINT ( 'NONE',  ( 4.159479030958464888E-15, -56.96472381958990638, 0.000000000000000000 ) ) ;
#6594 = CARTESIAN_POINT ( 'NONE',  ( -4.523095164977116484E-15, 12.12499999726881406, 24.62258325217400312 ) ) ;
#6595 = CARTESIAN_POINT ( 'NONE',  ( 6.950374756619721595, 36.06809000092397355, 26.09010956794232428 ) ) ;
#6596 = PRODUCT_DEFINITION_FORMATION_WITH_SPECIFIED_SOURCE ( 'ANY', '', #32094, .NOT_KNOWN. ) ;
#6597 = EDGE_LOOP ( 'NONE', ( #8292, #17548 ) ) ;
#6598 = CARTESIAN_POINT ( 'NONE',  ( -10.37757302488623701, 29.52500000273118630, 31.93888565452638417 ) ) ;
#6599 = CARTESIAN_POINT ( 'NONE',  ( -34.92499999999992610, 0.000000000000000000, 0.000000000000000000 ) ) ;
#6600 = EDGE_LOOP ( 'NONE', ( #30266, #4130, #15362, #12431 ) ) ;
#6601 = CARTESIAN_POINT ( 'NONE',  ( 26.00068869287340334, 61.12760416666665719, -15.01150461594642316 ) ) ;
#6602 = CARTESIAN_POINT ( 'NONE',  ( -10.37757302488624411, 58.97500000273120691, -31.93888565452638417 ) ) ;
#6603 = CARTESIAN_POINT ( 'NONE',  ( -32.50000000000000000, 36.40000000546236691, -10.55989012756945300 ) ) ;
#6604 = CARTESIAN_POINT ( 'NONE',  ( -27.16883889988624290, 64.92500000273118133, -19.73931689729374028 ) ) ;
#6605 = CARTESIAN_POINT ( 'NONE',  ( -2.584737979205441561E-13, 26.17968750000000000, -30.02300923189239512 ) ) ;
#6606 = CARTESIAN_POINT ( 'NONE',  ( 19.82091636218621389, 8.200000000000013500, -14.40073868116559197 ) ) ;
#6607 = CARTESIAN_POINT ( 'NONE',  ( 0.000000000000000000, 16.99999999999998579, 0.000000000000000000 ) ) ;
#6608 = CARTESIAN_POINT ( 'NONE',  ( 6.486482029760649416E-15, 15.62500000273117884, 35.31076352940723240 ) ) ;
#6609 = CARTESIAN_POINT ( 'NONE',  ( 11.25946833292375793, 74.07500000273120122, -8.180482586598735395 ) ) ;
#6610 = CARTESIAN_POINT ( 'NONE',  ( 30.02300923189239867, 46.22618083240936215, -0.04044903255044467877 ) ) ;
#6611 = CARTESIAN_POINT ( 'NONE',  ( -15.00000000000000000, 81.90000000000000568, -4.873795443493594171 ) ) ;
#6612 = CARTESIAN_POINT ( 'NONE',  ( 20.50609665441005092, 61.84374999999998579, 20.50609665440969209 ) ) ;
#6613 = CARTESIAN_POINT ( 'NONE',  ( -9.270509831248419985, 74.55000000546237970, 12.75976212528060039 ) ) ;
#6614 = CARTESIAN_POINT ( 'NONE',  ( -7.570916362186215665, 5.149999994537635573, 23.30088464923126423 ) ) ;
#6615 = CARTESIAN_POINT ( 'NONE',  ( 12.13525491562420910, 77.45000000546237118, -8.816778784387098611 ) ) ;
#6616 = CARTESIAN_POINT ( 'NONE',  ( 19.09188309203661049, 12.85937500000000000, -19.09188309203694445 ) ) ;
#6617 = CARTESIAN_POINT ( 'NONE',  ( -33.58253175000000113, 37.12500000273119838, 0.000000000000000000 ) ) ;
#6618 = CARTESIAN_POINT ( 'NONE',  ( -13.91746824999999532, 74.77500000273118985, -4.522059556121115875 ) ) ;
#6619 = CARTESIAN_POINT ( 'NONE',  ( -20.75514604977248112, 51.67500000273117422, 28.56700777964554661 ) ) ;
#6620 = CARTESIAN_POINT ( 'NONE',  ( -33.58253175000000113, 27.27500000273118985, -10.91162601494193041 ) ) ;
#6621 = CARTESIAN_POINT ( 'NONE',  ( -7.570916362186215665, 17.14999999453761959, 23.30088464923126423 ) ) ;
#6622 = CARTESIAN_POINT ( 'NONE',  ( -13.97622843553588901, 28.18489583333333215, 24.20753774853756823 ) ) ;
#6623 = CARTESIAN_POINT ( 'NONE',  ( -32.50000000000000000, 18.09999999999998010, 10.55989012756946366 ) ) ;
#6624 = CARTESIAN_POINT ( 'NONE',  ( 5.147494310547426899, 33.44874571845315359, -32.50000000000000000 ) ) ;
#6625 = CARTESIAN_POINT ( 'NONE',  ( -10.04305231718578462, 68.40000000000000568, 30.90933677959249337 ) ) ;
#6626 = CARTESIAN_POINT ( 'NONE',  ( -7.236395654485763274, 14.02499999726880553, 22.27133577429736633 ) ) ;
#6627 = CARTESIAN_POINT ( 'NONE',  ( -20.53372385742107653, 20.87461833240935505, -20.47846945139867003 ) ) ;
#6628 = CARTESIAN_POINT ( 'NONE',  ( -23.41746825000000243, 4.024999997268810858, -7.608796670333730638 ) ) ;
#6629 = CARTESIAN_POINT ( 'NONE',  ( 24.22776226481265383, 36.20013916574269075, 13.94119854578893580 ) ) ;
#6630 = ADVANCED_FACE ( 'NONE', ( #6888 ), #14452, .T. ) ;
#6631 = CARTESIAN_POINT ( 'NONE',  ( -10.37757302488623701, 13.52500000273118630, 31.93888565452638417 ) ) ;
#6632 = CARTESIAN_POINT ( 'NONE',  ( -7.236395654485757944, 9.724999997268806595, -22.27133577429736988 ) ) ;
#6633 = CARTESIAN_POINT ( 'NONE',  ( -26.07999730980477437, 59.55208333333332149, 6.988114217768305103 ) ) ;
#6634 = ORIENTED_EDGE ( 'NONE', *, *, #19623, .F. ) ;
#6635 = CARTESIAN_POINT ( 'NONE',  ( -10.37757302488624411, 48.72500000273120691, -31.93888565452638417 ) ) ;
#6636 = CARTESIAN_POINT ( 'NONE',  ( -27.16883889988624290, 23.17500000273119198, -19.73931689729374028 ) ) ;
#6637 = VERTEX_POINT ( 'NONE', #17201 ) ;
#6638 = CARTESIAN_POINT ( 'NONE',  ( -20.50609665440969209, 21.45312499999999645, 20.50609665441005092 ) ) ;
#6639 = CARTESIAN_POINT ( 'NONE',  ( 26.02091320914851025, 28.19048583425731636, -14.97647472619946463 ) ) ;
#6640 = AXIS2_PLACEMENT_3D ( 'NONE', #6647, #8884, #22275 ) ;
#6641 = CARTESIAN_POINT ( 'NONE',  ( -20.08610463437156923, 72.80000000546236549, 27.64615127144130113 ) ) ;
#6642 = CARTESIAN_POINT ( 'NONE',  ( 19.82091636218621034, 13.54999999453762527, 14.40073868116559730 ) ) ;
#6643 = CARTESIAN_POINT ( 'NONE',  ( -14.47279130897151589, 5.324999997268799135, -19.92008829642072598 ) ) ;
#6644 = CARTESIAN_POINT ( 'NONE',  ( -20.75514604977248823, 25.07500000273120122, -28.56700777964554305 ) ) ;
#6645 = CARTESIAN_POINT ( 'NONE',  ( -20.08610463437156923, 24.80000000546235839, 27.64615127144130113 ) ) ;
#6646 = CARTESIAN_POINT ( 'NONE',  ( -26.29305231718578995, 72.19999999999998863, 19.10302069950538595 ) ) ;
#6647 = CARTESIAN_POINT ( 'NONE',  ( 0.000000000000000000, 102.0000000000000284, 0.000000000000000000 ) ) ;
#6648 = CARTESIAN_POINT ( 'NONE',  ( -25.33181144634176363, 67.00000000000000000, -22.15645287101984096 ) ) ;
#6649 = CARTESIAN_POINT ( 'NONE',  ( 30.02300923189239867, 52.53944416759064495, 0.04044903254992252006 ) ) ;
#6650 = CARTESIAN_POINT ( 'NONE',  ( 20.75514604977248467, 36.67500000273118843, -28.56700777964554305 ) ) ;
#6651 = CARTESIAN_POINT ( 'NONE',  ( -20.75514604977248112, 57.42500000273119554, 28.56700777964554661 ) ) ;
#6652 = CARTESIAN_POINT ( 'NONE',  ( 7.505752307972854531, 33.19791666666665719, -28.01184896238303423 ) ) ;
#6653 = CARTESIAN_POINT ( 'NONE',  ( 0.000000000000000000, 82.00000000000000000, 0.000000000000000000 ) ) ;
#6654 = CARTESIAN_POINT ( 'NONE',  ( 23.41746824999999887, 9.124999997268817609, 0.000000000000000000 ) ) ;
#6655 = CARTESIAN_POINT ( 'NONE',  ( 20.08610463437157279, 17.30000000000000782, -27.64615127144129758 ) ) ;
#6656 = CARTESIAN_POINT ( 'NONE',  ( 24.50000000000000355, 16.09999999999998366, -7.960532557706203605 ) ) ;
#6657 = CARTESIAN_POINT ( 'NONE',  ( 6.950374756619257965, 42.07253499907601935, -26.09010956794244507 ) ) ;
#6658 = CARTESIAN_POINT ( 'NONE',  ( 20.75514604977249178, 57.82500000273118701, 28.56700777964553950 ) ) ;
#6659 = CARTESIAN_POINT ( 'NONE',  ( 10.37757302488624767, 47.97500000273119269, 31.93888565452638417 ) ) ;
#6660 =( BOUNDED_CURVE ( )  B_SPLINE_CURVE ( 2, ( #28826, #15972, #2921, #10645, #23178, #4809, #329, #2412, #10815, #20953, #12878, #31402, #7385 ),
 .UNSPECIFIED., .F., .F. ) 
 B_SPLINE_CURVE_WITH_KNOTS ( ( 3, 2, 2, 2, 2, 2, 3 ),
 ( 0.9038461538461538547, 0.9051282051282051322, 0.9076923076923076872, 0.9102564102564102422, 0.9128205128205127972, 0.9153846153846153522, 0.9166666666666666297 ),
 .UNSPECIFIED. ) 
 CURVE ( )  GEOMETRIC_REPRESENTATION_ITEM ( )  RATIONAL_B_SPLINE_CURVE ( ( 0.9755282581475768211, 0.9755282581475768211, 1.000000000000000000, 0.9510565162951535312, 1.000000000000000000, 0.9510565162951535312, 1.000000000000000000, 0.9510565162951535312, 1.000000000000000000, 0.9510565162951535312, 1.000000000000000000, 0.9755282581475768211, 0.9755282581475768211 ) ) 
 REPRESENTATION_ITEM ( '' )  );
#6661 = CARTESIAN_POINT ( 'NONE',  ( -14.47279130897152299, 7.924999997268802332, 19.92008829642072243 ) ) ;
#6662 = CARTESIAN_POINT ( 'NONE',  ( 2.757615341152813402E-15, -45.51763809020504681, 0.000000000000000000 ) ) ;
#6663 = CARTESIAN_POINT ( 'NONE',  ( 33.58253175000000113, 2.125000002731192161, -4.112674001490185761E-15 ) ) ;
#6664 = CARTESIAN_POINT ( 'NONE',  ( -24.22776226481240514, 47.09673583425730214, 13.94119854578937812 ) ) ;
#6665 = CARTESIAN_POINT ( 'NONE',  ( -1.053607264507113999E-13, 63.00000000546238255, 32.50000000000000711 ) ) ;
#6666 = CARTESIAN_POINT ( 'NONE',  ( -32.50000000000000000, 52.00000000000000711, 0.000000000000000000 ) ) ;
#6667 = CARTESIAN_POINT ( 'NONE',  ( 33.58253175000000113, 22.12500000273119483, -4.112674001490185761E-15 ) ) ;
#6668 = DIRECTION ( 'NONE',  ( 0.000000000000000000, -1.000000000000000000, 0.000000000000000000 ) ) ;
#6669 = DIRECTION ( 'NONE',  ( 1.000000000000000000, 0.000000000000000000, 0.000000000000000000 ) ) ;
#6670 = CARTESIAN_POINT ( 'NONE',  ( 32.50000000000000000, 41.60000000546236976, -10.55989012756945833 ) ) ;
#6671 = CARTESIAN_POINT ( 'NONE',  ( 14.97647472619900455, 62.84076416574269786, -26.02091320914876960 ) ) ;
#6672 = CARTESIAN_POINT ( 'NONE',  ( 20.08610463437157279, 39.80000000546238681, -27.64615127144129758 ) ) ;
#6673 = CARTESIAN_POINT ( 'NONE',  ( -8.891200544363830713E-16, 71.75000000546238255, -15.00000000000000000 ) ) ;
#6674 = CARTESIAN_POINT ( 'NONE',  ( 33.58253175000000113, 32.22500000273117848, -10.91162601494193574 ) ) ;
#6675 = CARTESIAN_POINT ( 'NONE',  ( -2.428612866367529427E-13, 36.49218750000000000, -27.95245687107222921 ) ) ;
#6676 = ORIENTED_EDGE ( 'NONE', *, *, #26197, .T. ) ;
#6677 = CARTESIAN_POINT ( 'NONE',  ( 33.58253175000000113, 76.12500000273118417, -4.112674001490185761E-15 ) ) ;
#6678 = CARTESIAN_POINT ( 'NONE',  ( -7.505752307973343918, 39.78645833333332860, -28.01184896238290989 ) ) ;
#6679 = DIRECTION ( 'NONE',  ( 0.000000000000000000, 0.000000000000000000, -1.000000000000000000 ) ) ;
#6680 = EDGE_LOOP ( 'NONE', ( #29263, #8499, #24698, #8128 ) ) ;
#6681 = CARTESIAN_POINT ( 'NONE',  ( 14.97647472619947351, 46.23736083425730925, 26.02091320914850314 ) ) ;
#6682 = CARTESIAN_POINT ( 'NONE',  ( -26.29305231718578995, 12.70000000546238361, 19.10302069950538595 ) ) ;
#6683 = CARTESIAN_POINT ( 'NONE',  ( 26.00068869287367335, 65.13802083333334281, 15.01150461594596308 ) ) ;
#6684 = CARTESIAN_POINT ( 'NONE',  ( 5.779280353836490358E-15, 65.00000000546236834, 32.49999999999999289 ) ) ;
#6685 = CARTESIAN_POINT ( 'NONE',  ( -10.37757302488623701, 39.77500000273118275, 31.93888565452638417 ) ) ;
#6686 = CARTESIAN_POINT ( 'NONE',  ( 32.50000000000000000, 41.60000000546238397, -10.55989012756945833 ) ) ;
#6687 = CARTESIAN_POINT ( 'NONE',  ( -8.960552108402742093E-16, 72.87500000273118417, -14.63369212191046387 ) ) ;
#6688 = CARTESIAN_POINT ( 'NONE',  ( -2.162160676586881955E-15, 28.62500000273118062, -35.31076352940723240 ) ) ;
#6689 = CARTESIAN_POINT ( 'NONE',  ( -20.08610463437157989, 23.70000000000000639, -27.64615127144129758 ) ) ;
#6690 = CARTESIAN_POINT ( 'NONE',  ( -20.75514604977248823, 53.07500000273118701, -28.56700777964554305 ) ) ;
#6691 = CARTESIAN_POINT ( 'NONE',  ( -10.04305231718579172, 33.60000000000000142, -30.90933677959248982 ) ) ;
#6692 = CARTESIAN_POINT ( 'NONE',  ( -26.29305231718578995, 36.20000000000000995, 19.10302069950538595 ) ) ;
#6693 = CARTESIAN_POINT ( 'NONE',  ( 18.94512977948575738, 8.424999997268811214, 13.76444248337723408 ) ) ;
#6694 = EDGE_CURVE ( 'NONE', #33755, #31336, #17368, .T. ) ;
#6695 = CARTESIAN_POINT ( 'NONE',  ( 33.58253175000000113, 78.22500000273119269, -10.91162601494193751 ) ) ;
#6696 = FACE_OUTER_BOUND ( 'NONE', #2729, .T. ) ;
#6697 = CARTESIAN_POINT ( 'NONE',  ( -13.91746824999999532, 77.27500000273118985, -4.522059556121115875 ) ) ;
#6698 = CARTESIAN_POINT ( 'NONE',  ( -33.58253175000000113, 67.47500000273116427, 10.91162601494193929 ) ) ;
#6699 = CARTESIAN_POINT ( 'NONE',  ( 12.13525491562421088, 75.05000000546240813, 8.816778784387095058 ) ) ;
#6700 = EDGE_CURVE ( 'NONE', #8211, #6218, #15908, .T. ) ;
#6701 = ORIENTED_EDGE ( 'NONE', *, *, #5600, .F. ) ;
#6702 = CARTESIAN_POINT ( 'NONE',  ( 1.577395562988744260E-15, 6.249999994537619230, -25.76082449383753925 ) ) ;
#6703 = CARTESIAN_POINT ( 'NONE',  ( 14.01125832528286352, 21.02902750092397710, -24.18731323226246843 ) ) ;
#6704 = CARTESIAN_POINT ( 'NONE',  ( 15.14183272437242422, 8.049999994537621717, -20.84094480462497856 ) ) ;
#6705 = AXIS2_PLACEMENT_3D ( 'NONE', #9035, #32037, #18851 ) ;
#6706 = CARTESIAN_POINT ( 'NONE',  ( -27.16883889988623935, 43.32500000273119412, 19.73931689729374739 ) ) ;
#6707 = CARTESIAN_POINT ( 'NONE',  ( -33.58253175000000113, 5.475000002731181148, 10.91162601494193929 ) ) ;
#6708 = CARTESIAN_POINT ( 'NONE',  ( -33.58253175000000113, 53.37500000273119838, 0.000000000000000000 ) ) ;
#6709 = CARTESIAN_POINT ( 'NONE',  ( 13.97622843553633842, 55.11197916666665719, 24.20753774853730889 ) ) ;
#6710 = CARTESIAN_POINT ( 'NONE',  ( 20.47846945139902530, 42.65663166759063785, 20.53372385742071771 ) ) ;
#6711 = AXIS2_PLACEMENT_3D ( 'NONE', #16675, #18922, #13605 ) ;
#6712 = CARTESIAN_POINT ( 'NONE',  ( -7.468012846824272799, 33.47878499907601935, 28.02196122052058413 ) ) ;
#6713 = CARTESIAN_POINT ( 'NONE',  ( -10.04305231718578462, 66.90000000546238823, 30.90933677959249337 ) ) ;
#6714 = CARTESIAN_POINT ( 'NONE',  ( -8.960552108402742093E-16, 72.37500000273115575, -14.63369212191046387 ) ) ;
#6715 = CARTESIAN_POINT ( 'NONE',  ( -19.06425588902558133, 54.39024333240934794, 19.11951029504797006 ) ) ;
#6716 = CYLINDRICAL_SURFACE ( 'NONE', #12746, 24.50000000000000000 ) ;
#6717 = VERTEX_POINT ( 'NONE', #32626 ) ;
#6718 = CARTESIAN_POINT ( 'NONE',  ( -20.75514604977248823, 39.07500000273119412, -28.56700777964554305 ) ) ;
#6719 = CARTESIAN_POINT ( 'NONE',  ( -23.41746824999999887, 4.124999997268813168, -2.867812753649727150E-15 ) ) ;
#6720 = CARTESIAN_POINT ( 'NONE',  ( -32.50000000000000000, 28.40000000546235981, -10.55989012756945478 ) ) ;
#6721 = ORIENTED_EDGE ( 'NONE', *, *, #1024, .T. ) ;
#6722 = CARTESIAN_POINT ( 'NONE',  ( 15.01150461594596308, 33.34114583333332860, -26.00068869287367335 ) ) ;
#6723 = VERTEX_POINT ( 'NONE', #4314 ) ;
#6724 = LINE ( 'NONE', #6393, #23733 ) ;
#6725 = CARTESIAN_POINT ( 'NONE',  ( 20.75514604977248467, 48.42500000273119554, -28.56700777964554305 ) ) ;
#6726 = CARTESIAN_POINT ( 'NONE',  ( 26.00068869287367335, 61.70052083333331439, 15.01150461594596308 ) ) ;
#6727 = CARTESIAN_POINT ( 'NONE',  ( 32.50000000000000000, 13.60000000546239285, -10.55989012756945833 ) ) ;
#6728 = AXIS2_PLACEMENT_3D ( 'NONE', #22944, #25686, #7146 ) ;
#6729 = CARTESIAN_POINT ( 'NONE',  ( -26.29305231718578995, 8.199999999999985079, 19.10302069950538595 ) ) ;
#6730 = CARTESIAN_POINT ( 'NONE',  ( -14.47279130897152299, 14.42499999726880056, 19.92008829642072243 ) ) ;
#6731 = CARTESIAN_POINT ( 'NONE',  ( -26.29305231718578995, 54.19999999999999574, 19.10302069950538595 ) ) ;
#6732 = EDGE_CURVE ( 'NONE', #19356, #16549, #16993, .T. ) ;
#6733 = DIRECTION ( 'NONE',  ( -0.000000000000000000, -1.000000000000000000, -0.000000000000000000 ) ) ;
#6734 = CARTESIAN_POINT ( 'NONE',  ( 33.58253175000000823, 14.27500000273119340, 10.91162601494192863 ) ) ;
#6735 = CARTESIAN_POINT ( 'NONE',  ( 15.00000000000000000, 77.00000000000001421, -1.836970198721029589E-15 ) ) ;
#6736 = CARTESIAN_POINT ( 'NONE',  ( 24.22776226481265383, 22.45013916574269075, 13.94119854578893580 ) ) ;
#6737 = CARTESIAN_POINT ( 'NONE',  ( 8.601468415847516980, 76.17500000273116711, -11.83890561707634781 ) ) ;
#6738 = CARTESIAN_POINT ( 'NONE',  ( 15.14183272437242422, 8.300000000000000711, -20.84094480462497856 ) ) ;
#6739 = CARTESIAN_POINT ( 'NONE',  ( 29.16592172374795311, 52.00000000000002842, 16.79171150063938356 ) ) ;
#6740 = ADVANCED_FACE ( 'NONE', ( #26448 ), #349, .T. ) ;
#6741 = CARTESIAN_POINT ( 'NONE',  ( 26.29305231718578995, 3.199999999999994404, -19.10302069950538240 ) ) ;
#6742 = EDGE_LOOP ( 'NONE', ( #14126, #10623, #87 ) ) ;
#6743 = CARTESIAN_POINT ( 'NONE',  ( 14.47279130897151767, 9.424999997268814766, -19.92008829642072598 ) ) ;
#6744 = CARTESIAN_POINT ( 'NONE',  ( 8.601468415847520532, 71.57500000273118701, 11.83890561707634781 ) ) ;
#6745 = CARTESIAN_POINT ( 'NONE',  ( 27.95245687107222921, 44.22656249999997868, -2.463307335887066074E-13 ) ) ;
#6746 = CARTESIAN_POINT ( 'NONE',  ( -10.37757302488623701, 65.52500000273118985, 31.93888565452638417 ) ) ;
#6747 = CARTESIAN_POINT ( 'NONE',  ( 33.58253175000000823, 26.27500000273119340, 10.91162601494192863 ) ) ;
#6748 = CARTESIAN_POINT ( 'NONE',  ( -33.58253175000000113, 7.475000002731190030, 10.91162601494193929 ) ) ;
#6749 = CARTESIAN_POINT ( 'NONE',  ( 6.486482029760648627E-15, 7.875000002731192161, 35.31076352940722529 ) ) ;
#6750 = CARTESIAN_POINT ( 'NONE',  ( -0.04044903254990864921, 12.14881916759064140, 30.02300923189239867 ) ) ;
#6751 = CARTESIAN_POINT ( 'NONE',  ( -15.01150461594595775, 52.24739583333332860, 26.00068869287368756 ) ) ;
#6752 = CARTESIAN_POINT ( 'NONE',  ( -13.91746824999999532, 73.27500000273120406, -4.522059556121115875 ) ) ;
#6753 = CARTESIAN_POINT ( 'NONE',  ( 32.50000000000000000, 47.10000000000000142, -10.55989012756945833 ) ) ;
#6754 = CARTESIAN_POINT ( 'NONE',  ( 10.04305231718579705, 57.10000000546237686, 30.90933677959248982 ) ) ;
#6755 = CARTESIAN_POINT ( 'NONE',  ( -33.58253175000000113, 49.02500000273116854, -10.91162601494193041 ) ) ;
#6756 = AXIS2_PLACEMENT_3D ( 'NONE', #122, #10614, #20758 ) ;
#6757 = CARTESIAN_POINT ( 'NONE',  ( -7.236395654485757944, 3.224999997268801266, -22.27133577429736988 ) ) ;
#6758 = ORIENTED_EDGE ( 'NONE', *, *, #16049, .T. ) ;
#6759 = CARTESIAN_POINT ( 'NONE',  ( -20.75514604977248823, 59.07500000273119412, -28.56700777964554305 ) ) ;
#6760 =( BOUNDED_CURVE ( )  B_SPLINE_CURVE ( 2, ( #1648, #30650, #25169, #12642, #9553, #4920, #25001, #9724, #30478, #33403, #30826, #4405, #20032 ),
 .UNSPECIFIED., .F., .T. ) 
 B_SPLINE_CURVE_WITH_KNOTS ( ( 3, 2, 2, 2, 2, 2, 3 ),
 ( 0.3611111111111111049, 0.3666666666666666408, 0.3777777777777777679, 0.3888888888888888951, 0.4000000000000000222, 0.4111111111111110938, 0.4166666666666666852 ),
 .UNSPECIFIED. ) 
 CURVE ( )  GEOMETRIC_REPRESENTATION_ITEM ( )  RATIONAL_B_SPLINE_CURVE ( ( 0.9755282581475768211, 0.9755282581475768211, 1.000000000000000000, 0.9510565162951535312, 1.000000000000000000, 0.9510565162951535312, 1.000000000000000000, 0.9510565162951535312, 1.000000000000000000, 0.9510565162951535312, 1.000000000000000000, 0.9755282581475765991, 0.9755282581475767101 ) ) 
 REPRESENTATION_ITEM ( '' )  );
#6761 = DIRECTION ( 'NONE',  ( 0.000000000000000000, 0.000000000000000000, -1.000000000000000000 ) ) ;
#6762 = CARTESIAN_POINT ( 'NONE',  ( 14.47279130897151589, 14.32499999726880624, 19.92008829642072953 ) ) ;
#6763 = CARTESIAN_POINT ( 'NONE',  ( -26.06988505166735237, 33.77642333425730214, -7.025853678916388567 ) ) ;
#6764 = EDGE_LOOP ( 'NONE', ( #23457, #19923, #19586, #20768 ) ) ;
#6765 = CARTESIAN_POINT ( 'NONE',  ( 33.58253175000000823, 32.02500000273118275, 10.91162601494192863 ) ) ;
#6766 = ORIENTED_EDGE ( 'NONE', *, *, #8408, .T. ) ;
#6767 = CARTESIAN_POINT ( 'NONE',  ( 15.01150461594596308, 60.84114583333332860, -26.00068869287367335 ) ) ;
#6768 = CARTESIAN_POINT ( 'NONE',  ( -27.16883889988624290, 59.17500000273118133, -19.73931689729374028 ) ) ;
#6769 = CARTESIAN_POINT ( 'NONE',  ( 11.54700538379251107, 96.00000000000002842, -19.99999999999999645 ) ) ;
#6770 = CARTESIAN_POINT ( 'NONE',  ( 20.75514604977248467, 66.42500000273120975, -28.56700777964554305 ) ) ;
#6771 = CARTESIAN_POINT ( 'NONE',  ( -28.01184896238304134, 32.33854166666666430, -7.505752307972844761 ) ) ;
#6772 = CARTESIAN_POINT ( 'NONE',  ( -15.14183272437242600, 15.30000000000001137, 20.84094480462497856 ) ) ;
#6773 = CARTESIAN_POINT ( 'NONE',  ( -33.58253175000000113, 1.375000002731191495, 0.000000000000000000 ) ) ;
#6774 = CARTESIAN_POINT ( 'NONE',  ( 33.58253175000000113, 12.12500000273120193, -4.112674001490185761E-15 ) ) ;
#6775 = CARTESIAN_POINT ( 'NONE',  ( -10.04305231718578462, 0.9000000054623646939, 30.90933677959249337 ) ) ;
#6776 = CARTESIAN_POINT ( 'NONE',  ( -20.53372385742107653, 44.93711833240935505, -20.47846945139867003 ) ) ;
#6777 = CARTESIAN_POINT ( 'NONE',  ( 12.13525491562421088, 74.80000000000001137, 8.816778784387095058 ) ) ;
#6778 = AXIS2_PLACEMENT_3D ( 'NONE', #20788, #21295, #8063 ) ;
#6779 = CARTESIAN_POINT ( 'NONE',  ( -20.50609665440969209, 59.26562500000000000, 20.50609665441005092 ) ) ;
#6780 = AXIS2_PLACEMENT_3D ( 'NONE', #33203, #30630, #9706 ) ;
#6781 = CARTESIAN_POINT ( 'NONE',  ( 20.08610463437157279, 23.29999999999999005, -27.64615127144129758 ) ) ;
#6782 = CARTESIAN_POINT ( 'NONE',  ( 7.570916362186213000, 8.149999994537637349, -23.30088464923126423 ) ) ;
#6783 = CARTESIAN_POINT ( 'NONE',  ( -15.00000000000000000, 80.25000000546239676, 0.000000000000000000 ) ) ;
#6784 = CARTESIAN_POINT ( 'NONE',  ( -24.20753774853756823, 15.29427083333332504, -13.97622843553588723 ) ) ;
#6785 = CARTESIAN_POINT ( 'NONE',  ( 10.37757302488624767, 39.72500000273118559, 31.93888565452638417 ) ) ;
#6786 = CARTESIAN_POINT ( 'NONE',  ( 13.91746824999999532, 75.97500000273116427, -4.522059556121118540 ) ) ;
#6787 = CARTESIAN_POINT ( 'NONE',  ( 27.16883889988623935, 44.57500000273119412, -19.73931689729374384 ) ) ;
#6788 = CARTESIAN_POINT ( 'NONE',  ( 27.16883889988623935, 26.57500000273119056, -19.73931689729374384 ) ) ;
#6789 = CARTESIAN_POINT ( 'NONE',  ( 32.50000000000000000, 41.10000000000000853, -10.55989012756945833 ) ) ;
#6790 = APPLICATION_CONTEXT ( 'automotive_design' ) ;
#6791 = CARTESIAN_POINT ( 'NONE',  ( 7.570916362186207671, 1.599999999999990319, 23.30088464923126779 ) ) ;
#6792 = CARTESIAN_POINT ( 'NONE',  ( 26.29305231718579350, 68.80000000000001137, 19.10302069950537529 ) ) ;
#6793 = CARTESIAN_POINT ( 'NONE',  ( 7.236395654485760609, 11.02499999726880375, -22.27133577429736633 ) ) ;
#6794 = CARTESIAN_POINT ( 'NONE',  ( 28.02196122052058413, 22.30690999907601579, 7.468012846824272799 ) ) ;
#6795 = CARTESIAN_POINT ( 'NONE',  ( -18.94512977948575738, 3.924999997268807661, -13.76444248337723231 ) ) ;
#6796 = CARTESIAN_POINT ( 'NONE',  ( -24.22776226481266448, 37.91888916574269075, -13.94119854578892514 ) ) ;
#6797 = FACE_OUTER_BOUND ( 'NONE', #33883, .T. ) ;
#6798 = CARTESIAN_POINT ( 'NONE',  ( 27.16883889988623935, 14.32500000273117990, -19.73931689729374384 ) ) ;
#6799 = CARTESIAN_POINT ( 'NONE',  ( -18.94512977948575738, 9.924999997268812990, -13.76444248337723231 ) ) ;
#6800 = CARTESIAN_POINT ( 'NONE',  ( -2.428612866367529427E-13, 63.99218749999997868, -27.95245687107222921 ) ) ;
#6801 = VERTEX_POINT ( 'NONE', #29668 ) ;
#6802 = CARTESIAN_POINT ( 'NONE',  ( 33.58253175000000113, 52.22500000273117848, -10.91162601494193751 ) ) ;
#6803 = CARTESIAN_POINT ( 'NONE',  ( -27.16883889988623935, 23.57500000273120122, 19.73931689729374739 ) ) ;
#6804 = ORIENTED_EDGE ( 'NONE', *, *, #7993, .F. ) ;
#6805 = CARTESIAN_POINT ( 'NONE',  ( 15.01150461594643204, 37.92447916666666430, 26.00068869287340334 ) ) ;
#6806 = CARTESIAN_POINT ( 'NONE',  ( -28.00173670424549499, 30.33892333425730925, -7.543491769121417612 ) ) ;
#6807 = CARTESIAN_POINT ( 'NONE',  ( -24.50000000000000711, 3.099999999999989431, 7.960532557706201828 ) ) ;
#6808 = CARTESIAN_POINT ( 'NONE',  ( 19.82091636218621389, 13.94999999453763806, -14.40073868116559197 ) ) ;
#6809 = CARTESIAN_POINT ( 'NONE',  ( 23.41746825000000243, 10.52499999726880731, 7.608796670333735079 ) ) ;
#6810 = CARTESIAN_POINT ( 'NONE',  ( 10.37757302488624056, 22.77500000273119340, -31.93888565452638417 ) ) ;
#6811 = CARTESIAN_POINT ( 'NONE',  ( 20.08610463437158344, 23.20000000546238539, 27.64615127144129403 ) ) ;
#6812 = CARTESIAN_POINT ( 'NONE',  ( 20.08610463437157279, 73.29999999999996874, -27.64615127144129758 ) ) ;
#6813 = CARTESIAN_POINT ( 'NONE',  ( -26.29305231718579350, 6.300000005462380592, -19.10302069950537884 ) ) ;
#6814 = CARTESIAN_POINT ( 'NONE',  ( -13.36811651448714677, 74.00000000000004263, 6.258549183928298731 ) ) ;
#6815 = CARTESIAN_POINT ( 'NONE',  ( 26.02091320914851025, 52.25298583425730925, -14.97647472619946463 ) ) ;
#6816 = CARTESIAN_POINT ( 'NONE',  ( 33.58253175000000113, 36.37500000273119838, -4.112674001490185761E-15 ) ) ;
#6817 = CARTESIAN_POINT ( 'NONE',  ( 10.37757302488624767, 55.72500000273118559, 31.93888565452638417 ) ) ;
#6818 = CARTESIAN_POINT ( 'NONE',  ( -28.01184896238304134, 32.33854166666666430, -7.505752307972844761 ) ) ;
#6819 = CARTESIAN_POINT ( 'NONE',  ( -7.236395654485757944, 7.724999997268805707, -22.27133577429736988 ) ) ;
#6820 = CARTESIAN_POINT ( 'NONE',  ( 32.50000000000000711, 12.90000000000000036, 10.55989012756945122 ) ) ;
#6821 = CARTESIAN_POINT ( 'NONE',  ( 32.50000000000000000, 9.600000005462375086, -10.55989012756945833 ) ) ;
#6822 = CARTESIAN_POINT ( 'NONE',  ( -26.06988505166722803, 44.36420166574269075, 7.025853678916877953 ) ) ;
#6823 = CARTESIAN_POINT ( 'NONE',  ( -27.16883889988623935, 57.32500000273119412, 19.73931689729374739 ) ) ;
#6824 = CARTESIAN_POINT ( 'NONE',  ( 33.58253175000000113, 50.37500000273120548, -4.112674001490185761E-15 ) ) ;
#6825 = CARTESIAN_POINT ( 'NONE',  ( 14.47279130897151767, 14.32499999726880624, 19.92008829642072953 ) ) ;
#6826 = EDGE_CURVE ( 'NONE', #1603, #30131, #11995, .T. ) ;
#6827 = LINE ( 'NONE', #22289, #24879 ) ;
#6828 = CARTESIAN_POINT ( 'NONE',  ( -27.16883889988623935, 1.325000002731169246, 19.73931689729374739 ) ) ;
#6829 = CARTESIAN_POINT ( 'NONE',  ( -19.11951029504763611, 46.95350666759064495, 19.06425588902592239 ) ) ;
#6830 = CARTESIAN_POINT ( 'NONE',  ( -6.391981326054763102, 16.99999999999998224, -22.99215804002973940 ) ) ;
#6831 = CARTESIAN_POINT ( 'NONE',  ( 15.14183272437242067, 3.699999999999999289, 20.84094480462498211 ) ) ;
#6832 = CARTESIAN_POINT ( 'NONE',  ( -20.75514604977248823, 20.82500000273119412, -28.56700777964554305 ) ) ;
#6833 = DIRECTION ( 'NONE',  ( 0.000000000000000000, -0.000000000000000000, -1.000000000000000000 ) ) ;
#6834 = CARTESIAN_POINT ( 'NONE',  ( 5.779280353836490358E-15, 55.00000000546238965, 32.49999999999999289 ) ) ;
#6835 = ADVANCED_FACE ( 'NONE', ( #22140 ), #3605, .F. ) ;
#6836 = CARTESIAN_POINT ( 'NONE',  ( 3.980102097228898626E-15, 80.00000000000001421, 32.50000000000000000 ) ) ;
#6837 = ADVANCED_FACE ( 'NONE', ( #8747 ), #24377, .T. ) ;
#6838 = CARTESIAN_POINT ( 'NONE',  ( -14.01125832528328985, 14.14284749907602290, -24.18731323226223040 ) ) ;
#6839 = CARTESIAN_POINT ( 'NONE',  ( 32.50000000000000711, 39.40000000546236691, 10.55989012756945122 ) ) ;
#6840 = LINE ( 'NONE', #28122, #3022 ) ;
#6841 = CARTESIAN_POINT ( 'NONE',  ( 20.75514604977249178, 31.82500000273119056, 28.56700777964553950 ) ) ;
#6842 = CARTESIAN_POINT ( 'NONE',  ( 6.486482029760649416E-15, 65.87500000273119838, 35.31076352940723240 ) ) ;
#6843 = CARTESIAN_POINT ( 'NONE',  ( -26.07999730980477437, 32.05208333333332860, 6.988114217768305103 ) ) ;
#6844 = ORIENTED_EDGE ( 'NONE', *, *, #28947, .T. ) ;
#6845 = EDGE_CURVE ( 'NONE', #28463, #33921, #21228, .T. ) ;
#6846 = CARTESIAN_POINT ( 'NONE',  ( -20.75514604977248823, 70.82500000273117280, -28.56700777964554305 ) ) ;
#6847 = CARTESIAN_POINT ( 'NONE',  ( -28.01184896238304134, 42.65104166666666430, -7.505752307972844761 ) ) ;
#6848 = MECHANICAL_DESIGN_GEOMETRIC_PRESENTATION_REPRESENTATION (  '', ( #11770 ), #29846 ) ;
#6849 = CARTESIAN_POINT ( 'NONE',  ( 24.49999999999999289, -1.999999999999995337, 3.000384657911015074E-15 ) ) ;
#6850 = ORIENTED_EDGE ( 'NONE', *, *, #8451, .F. ) ;
#6851 = CARTESIAN_POINT ( 'NONE',  ( -7.543491769121417612, 60.41704833425730214, 28.00173670424549499 ) ) ;
#6852 = CARTESIAN_POINT ( 'NONE',  ( -19.11951029504763611, 57.26600666759063785, 19.06425588902592239 ) ) ;
#6853 = CARTESIAN_POINT ( 'NONE',  ( -33.58253175000000113, 11.02500000273117919, -10.91162601494193218 ) ) ;
#6854 = CARTESIAN_POINT ( 'NONE',  ( 26.00068869287367335, 61.70052083333331439, 15.01150461594596308 ) ) ;
#6855 = CARTESIAN_POINT ( 'NONE',  ( -26.29305231718579350, 64.30000000546237970, -19.10302069950537884 ) ) ;
#6856 = CARTESIAN_POINT ( 'NONE',  ( 33.58253175000000113, 42.47500000273119980, -10.91162601494193751 ) ) ;
#6857 = CARTESIAN_POINT ( 'NONE',  ( -32.50000000000000000, 46.50000000546239676, 0.000000000000000000 ) ) ;
#6858 = CARTESIAN_POINT ( 'NONE',  ( -8.601468415847515203, 75.67500000273116711, 11.83890561707634959 ) ) ;
#6859 = CARTESIAN_POINT ( 'NONE',  ( 6.486482029760649416E-15, 27.62500000273118062, 35.31076352940723240 ) ) ;
#6860 = CARTESIAN_POINT ( 'NONE',  ( -26.29305231718578995, 24.19999999999999929, 19.10302069950538595 ) ) ;
#6861 = CARTESIAN_POINT ( 'NONE',  ( 10.37757302488624056, 54.77500000273119696, -31.93888565452638417 ) ) ;
#6862 = CARTESIAN_POINT ( 'NONE',  ( 20.08610463437157279, 37.30000000000001847, -27.64615127144129758 ) ) ;
#6863 = CARTESIAN_POINT ( 'NONE',  ( -10.04305231718579172, 33.59999999999999432, -30.90933677959248982 ) ) ;
#6864 = CARTESIAN_POINT ( 'NONE',  ( 7.570916362186207671, 1.599999999999990319, 23.30088464923126779 ) ) ;
#6865 = CARTESIAN_POINT ( 'NONE',  ( -27.16883889988624290, 74.92500000273119554, -19.73931689729374028 ) ) ;
#6866 = LINE ( 'NONE', #30885, #1388 ) ;
#6867 = CARTESIAN_POINT ( 'NONE',  ( 8.601468415847520532, 76.07500000273117280, 11.83890561707634603 ) ) ;
#6868 = CARTESIAN_POINT ( 'NONE',  ( -33.58253175000000113, 69.27500000273116143, -10.91162601494193041 ) ) ;
#6869 = ORIENTED_EDGE ( 'NONE', *, *, #32222, .T. ) ;
#6870 = CARTESIAN_POINT ( 'NONE',  ( -19.82091636218621034, 8.549999994537621717, -14.40073868116559552 ) ) ;
#6871 = COLOUR_RGB ( '', 0.09019608, 0.27058824, 0.51372549) ;
#6872 = CARTESIAN_POINT ( 'NONE',  ( 13.94119854578937812, 22.17486083425730925, 24.22776226481240514 ) ) ;
#6873 = CARTESIAN_POINT ( 'NONE',  ( 7.570916362186207671, 7.349999994537615322, 23.30088464923126779 ) ) ;
#6874 = CARTESIAN_POINT ( 'NONE',  ( 27.16883889988624290, 41.92500000273118133, 19.73931689729373673 ) ) ;
#6875 = CARTESIAN_POINT ( 'NONE',  ( 33.58253175000000113, 2.375000002731192161, -4.112674001490185761E-15 ) ) ;
#6876 = CARTESIAN_POINT ( 'NONE',  ( -20.75514604977248823, 53.07500000273118701, -28.56700777964554305 ) ) ;
#6877 = CARTESIAN_POINT ( 'NONE',  ( -25.98046417659859486, 47.66965250092398065, -15.04653450569291628 ) ) ;
#6878 = CARTESIAN_POINT ( 'NONE',  ( -28.00173670424535644, 37.48920166574269075, 7.543491769121936308 ) ) ;
#6879 = CARTESIAN_POINT ( 'NONE',  ( -32.50000000000000000, 62.60000000546238397, 10.55989012756946366 ) ) ;
#6880 = CARTESIAN_POINT ( 'NONE',  ( -4.300734207923755825, 73.27500000273118985, 13.23629886949340673 ) ) ;
#6881 = VECTOR ( 'NONE', #1924, 1000.000000000000000 ) ;
#6882 = CARTESIAN_POINT ( 'NONE',  ( 0.04044903255044120238, 64.27305583240934084, 27.95245687107223276 ) ) ;
#6883 = CARTESIAN_POINT ( 'NONE',  ( 5.779280353836490358E-15, 42.49999999999999289, 32.49999999999999289 ) ) ;
#6884 = CARTESIAN_POINT ( 'NONE',  ( 10.04305231718579705, 73.10000000546237686, 30.90933677959248982 ) ) ;
#6885 = CARTESIAN_POINT ( 'NONE',  ( -28.01184896238304134, 15.15104166666666252, -7.505752307972844761 ) ) ;
#6886 = ADVANCED_FACE ( 'NONE', ( #27448 ), #14078, .F. ) ;
#6887 = CARTESIAN_POINT ( 'NONE',  ( -20.75514604977248112, 41.67500000273117422, 28.56700777964554661 ) ) ;
#6888 = FACE_OUTER_BOUND ( 'NONE', #18526, .T. ) ;
#6889 = ORIENTED_EDGE ( 'NONE', *, *, #24376, .F. ) ;
#6890 = CARTESIAN_POINT ( 'NONE',  ( -20.08610463437157989, 32.20000000546238539, -27.64615127144129758 ) ) ;
#6891 = ORIENTED_EDGE ( 'NONE', *, *, #16640, .T. ) ;
#6892 = CARTESIAN_POINT ( 'NONE',  ( 15.01150461594596308, 36.77864583333332860, -26.00068869287367335 ) ) ;
#6893 = CARTESIAN_POINT ( 'NONE',  ( 26.29305231718578995, 61.70000000546238539, -19.10302069950538240 ) ) ;
#6894 = ORIENTED_EDGE ( 'NONE', *, *, #5383, .T. ) ;
#6895 = CARTESIAN_POINT ( 'NONE',  ( 0.000000000000000000, 0.000000000000000000, 30.00000000000004974 ) ) ;
#6896 = CARTESIAN_POINT ( 'NONE',  ( -10.37757302488623701, 49.52500000273118985, 31.93888565452638417 ) ) ;
#6897 = CARTESIAN_POINT ( 'NONE',  ( 1.507698388325705758E-15, 17.12499999726880517, -24.62258325217400312 ) ) ;
#6898 = DIRECTION ( 'NONE',  ( -1.000000000000000000, 0.000000000000000000, 0.000000000000000000 ) ) ;
#6899 = CARTESIAN_POINT ( 'NONE',  ( -10.04305231718578462, 4.900000005462368691, 30.90933677959249337 ) ) ;
#6900 = CARTESIAN_POINT ( 'NONE',  ( 20.75514604977249178, 65.82500000273115859, 28.56700777964553950 ) ) ;
#6901 = CARTESIAN_POINT ( 'NONE',  ( -7.236395654485763274, 12.52499999726880375, 22.27133577429736633 ) ) ;
#6902 = CARTESIAN_POINT ( 'NONE',  ( 6.277390505771533514E-15, 52.50000000000000000, 34.17252228774368916 ) ) ;
#6903 = CARTESIAN_POINT ( 'NONE',  ( -23.41746825000000243, 1.524999997268801755, -7.608796670333730638 ) ) ;
#6904 = CARTESIAN_POINT ( 'NONE',  ( 20.75514604977248467, 16.67500000273117777, -28.56700777964554305 ) ) ;
#6905 = VECTOR ( 'NONE', #3047, 999.9999999999998863 ) ;
#6906 = CARTESIAN_POINT ( 'NONE',  ( -1.631291757790872152E-15, 111.9999999999999858, -13.32050807568876927 ) ) ;
#6907 = CARTESIAN_POINT ( 'NONE',  ( 14.01125832528330051, 29.61159749907602290, 24.18731323226221974 ) ) ;
#6908 = CARTESIAN_POINT ( 'NONE',  ( 11.25946833292375793, 74.07500000273120122, -8.180482586598735395 ) ) ;
#6909 = CARTESIAN_POINT ( 'NONE',  ( -10.17814985357208535, -45.51763809020504681, 1.246463863941915894E-15 ) ) ;
#6910 = CARTESIAN_POINT ( 'NONE',  ( -10.04305231718579172, 43.60000000000000142, -30.90933677959248982 ) ) ;
#6911 = CARTESIAN_POINT ( 'NONE',  ( 32.50000000000000000, 6.999999999999992006, -3.980102097228898626E-15 ) ) ;
#6912 = ORIENTED_EDGE ( 'NONE', *, *, #14411, .T. ) ;
#6913 = CARTESIAN_POINT ( 'NONE',  ( 18.94512977948576093, 7.324999997268822227, -13.76444248337722875 ) ) ;
#6914 = CARTESIAN_POINT ( 'NONE',  ( 19.09188309203694800, 51.53124999999999289, 19.09188309203660694 ) ) ;
#6915 = CARTESIAN_POINT ( 'NONE',  ( -33.58253175000000113, 61.22500000273118559, 10.91162601494193929 ) ) ;
#6916 = CARTESIAN_POINT ( 'NONE',  ( -27.16883889988623935, 23.57500000273120122, 19.73931689729374739 ) ) ;
#6917 = CARTESIAN_POINT ( 'NONE',  ( 10.37757302488624056, 12.77500000273117031, -31.93888565452638417 ) ) ;
#6918 = CARTESIAN_POINT ( 'NONE',  ( -5.147494310547423346, 20.44874571845315003, 32.50000000000000000 ) ) ;
#6919 = CARTESIAN_POINT ( 'NONE',  ( 25.98046417659858420, 21.88840250092397710, 15.04653450569292872 ) ) ;
#6920 = CARTESIAN_POINT ( 'NONE',  ( -7.505752307973343918, 63.84895833333332860, -28.01184896238290989 ) ) ;
#6921 = CARTESIAN_POINT ( 'NONE',  ( -20.75514604977248823, 2.825000002731177240, -28.56700777964554305 ) ) ;
#6922 = CARTESIAN_POINT ( 'NONE',  ( 32.50000000000000000, 69.09999999999998010, -10.55989012756945833 ) ) ;
#6923 = CARTESIAN_POINT ( 'NONE',  ( -32.50000000000000000, 41.89999999999999147, -10.55989012756945478 ) ) ;
#6924 = CARTESIAN_POINT ( 'NONE',  ( 33.58253175000000113, 50.22500000273118559, -10.91162601494193574 ) ) ;
#6925 = CARTESIAN_POINT ( 'NONE',  ( -7.236395654485757944, 1.224999997268799712, -22.27133577429736988 ) ) ;
#6926 = CARTESIAN_POINT ( 'NONE',  ( -12.90513655866680587, 66.99999999999998579, -31.00393344628902881 ) ) ;
#6927 = ORIENTED_EDGE ( 'NONE', *, *, #26774, .F. ) ;
#6928 = ADVANCED_FACE ( 'NONE', ( #1521, #29847 ), #21805, .T. ) ;
#6929 = CARTESIAN_POINT ( 'NONE',  ( -27.16883889988624290, 59.17500000273119554, -19.73931689729374028 ) ) ;
#6930 = CARTESIAN_POINT ( 'NONE',  ( 10.04305231718579705, 16.60000000000000497, 30.90933677959248982 ) ) ;
#6931 = CARTESIAN_POINT ( 'NONE',  ( 18.94512977948575738, 10.42499999726881299, 13.76444248337723408 ) ) ;
#6932 = CARTESIAN_POINT ( 'NONE',  ( -24.22776226481240514, 36.78423583425730214, 13.94119854578937812 ) ) ;
#6933 = EDGE_CURVE ( 'NONE', #25517, #1690, #6518, .T. ) ;
#6934 = ORIENTED_EDGE ( 'NONE', *, *, #23790, .F. ) ;
#6935 = CARTESIAN_POINT ( 'NONE',  ( 10.37757302488624767, 31.72500000273119269, 31.93888565452638417 ) ) ;
#6936 = DIRECTION ( 'NONE',  ( 0.000000000000000000, 0.000000000000000000, 1.000000000000000000 ) ) ;
#6937 = EDGE_LOOP ( 'NONE', ( #17456, #13462, #25125, #30216 ) ) ;
#6938 = CARTESIAN_POINT ( 'NONE',  ( 26.00068869287367335, 58.26302083333332149, 15.01150461594596308 ) ) ;
#6939 = FACE_OUTER_BOUND ( 'NONE', #26804, .T. ) ;
#6940 = CARTESIAN_POINT ( 'NONE',  ( -2.162160676586881955E-15, 68.62500000273119838, -35.31076352940723240 ) ) ;
#6941 = CARTESIAN_POINT ( 'NONE',  ( 2.740863092043355209E-13, 41.64843750000000000, 30.02300923189239512 ) ) ;
#6942 = CARTESIAN_POINT ( 'NONE',  ( -15.14183272437241889, 14.70000000000000107, -20.84094480462497856 ) ) ;
#6943 = CARTESIAN_POINT ( 'NONE',  ( -2.162160676586881955E-15, 4.875000002731200155, -35.31076352940723240 ) ) ;
#6944 = CARTESIAN_POINT ( 'NONE',  ( -33.58253175000000113, 11.22500000273120335, 10.91162601494193929 ) ) ;
#6945 = CARTESIAN_POINT ( 'NONE',  ( 11.25946833292375793, 71.67500000273119554, 8.180482586598731842 ) ) ;
#6946 = CARTESIAN_POINT ( 'NONE',  ( -28.02196122052058413, 54.96315999907602645, -7.468012846824272799 ) ) ;
#6947 = CARTESIAN_POINT ( 'NONE',  ( 15.00000000000000000, 77.00000000000001421, -1.836970198721029589E-15 ) ) ;
#6948 = CARTESIAN_POINT ( 'NONE',  ( 2.740863092043355209E-13, 58.83593750000000711, 30.02300923189239867 ) ) ;
#6949 = CARTESIAN_POINT ( 'NONE',  ( 5.779280353836490358E-15, 61.00000000546238255, 32.49999999999999289 ) ) ;
#6950 = CARTESIAN_POINT ( 'NONE',  ( -19.82091636218621389, 4.949999994537629178, 14.40073868116558842 ) ) ;
#6951 = CARTESIAN_POINT ( 'NONE',  ( 4.635254915624209993, 77.65000000546237402, -14.26584774442730463 ) ) ;
#6952 = CARTESIAN_POINT ( 'NONE',  ( 2.584737979205441561E-13, 21.02343749999999645, 27.95245687107222921 ) ) ;
#6953 = CARTESIAN_POINT ( 'NONE',  ( 20.75514604977249178, 35.82500000273117990, 28.56700777964553950 ) ) ;
#6954 = CARTESIAN_POINT ( 'NONE',  ( -13.91746824999999887, 70.87500000273122680, 0.000000000000000000 ) ) ;
#6955 = CARTESIAN_POINT ( 'NONE',  ( 10.37757302488624767, 39.97500000273117138, 31.93888565452638417 ) ) ;
#6956 = CARTESIAN_POINT ( 'NONE',  ( 10.37757302488624767, 21.97500000273119980, 31.93888565452638417 ) ) ;
#6957 = CARTESIAN_POINT ( 'NONE',  ( 5.147494310547426899, 41.44874571845314648, -32.50000000000000000 ) ) ;
#6958 = DIRECTION ( 'NONE',  ( 0.000000000000000000, 0.000000000000000000, -1.000000000000000000 ) ) ;
#6959 = CARTESIAN_POINT ( 'NONE',  ( 26.29305231718578995, 79.19999999999998863, -19.10302069950538240 ) ) ;
#6960 =( BOUNDED_CURVE ( )  B_SPLINE_CURVE ( 2, ( #24829, #32711, #9207, #6641, #33048, #31001, #4578, #9900, #15056, #22772, #33225, #17462, #25688 ),
 .UNSPECIFIED., .F., .T. ) 
 B_SPLINE_CURVE_WITH_KNOTS ( ( 3, 2, 2, 2, 2, 2, 3 ),
 ( 0.07051282051282051211, 0.07179487179487178961, 0.07435897435897435848, 0.07692307692307692735, 0.07948717948717948234, 0.08205128205128205121, 0.08333333333333334259 ),
 .UNSPECIFIED. ) 
 CURVE ( )  GEOMETRIC_REPRESENTATION_ITEM ( )  RATIONAL_B_SPLINE_CURVE ( ( 0.9755282581475768211, 0.9755282581475768211, 1.000000000000000000, 0.9510565162951535312, 1.000000000000000000, 0.9510565162951535312, 1.000000000000000000, 0.9510565162951535312, 1.000000000000000000, 0.9510565162951535312, 1.000000000000000000, 0.9755282581475765991, 0.9755282581475767101 ) ) 
 REPRESENTATION_ITEM ( '' )  );
#6961 = CARTESIAN_POINT ( 'NONE',  ( -32.50000000000000000, 65.99999999999998579, 0.000000000000000000 ) ) ;
#6962 = CARTESIAN_POINT ( 'NONE',  ( 7.236395654485755280, 8.224999997268806595, 22.27133577429736988 ) ) ;
#6963 = CARTESIAN_POINT ( 'NONE',  ( -7.543491769121917656, 28.03607666574268364, -28.00173670424536354 ) ) ;
#6964 = VECTOR ( 'NONE', #27967, 1000.000000000000000 ) ;
#6965 = CARTESIAN_POINT ( 'NONE',  ( 14.47279130897151589, 4.824999997268814234, 19.92008829642072953 ) ) ;
#6966 = CARTESIAN_POINT ( 'NONE',  ( 14.01125832528330051, 33.04909749907601935, 24.18731323226221974 ) ) ;
#6967 = CYLINDRICAL_SURFACE ( 'NONE', #15649, 24.50000000000000000 ) ;
#6968 = CARTESIAN_POINT ( 'NONE',  ( -10.37757302488623701, 11.52500000273118452, 31.93888565452638417 ) ) ;
#6969 = CARTESIAN_POINT ( 'NONE',  ( 23.41746824999999887, 9.124999997268817609, 0.000000000000000000 ) ) ;
#6970 = CARTESIAN_POINT ( 'NONE',  ( -27.95245687107222921, 66.57031250000000000, 2.498001805406602216E-13 ) ) ;
#6971 = ORIENTED_EDGE ( 'NONE', *, *, #6421, .F. ) ;
#6972 = CARTESIAN_POINT ( 'NONE',  ( -2.162160676586881955E-15, 46.62500000273119127, -35.31076352940723240 ) ) ;
#6973 = CARTESIAN_POINT ( 'NONE',  ( 20.75514604977249178, 24.07500000273120122, 28.56700777964553950 ) ) ;
#6974 = ADVANCED_FACE ( 'NONE', ( #30176 ), #16656, .T. ) ;
#6975 = EDGE_CURVE ( 'NONE', #16033, #32341, #14157, .T. ) ;
#6976 = VERTEX_POINT ( 'NONE', #6346 ) ;
#6977 = CARTESIAN_POINT ( 'NONE',  ( -20.50609665441004736, 29.18749999999999645, -20.50609665440969565 ) ) ;
#6978 = CARTESIAN_POINT ( 'NONE',  ( -30.02300923189239867, 33.63319416759063785, -0.04044903254991731589 ) ) ;
#6979 = CARTESIAN_POINT ( 'NONE',  ( 0.000000000000000000, 82.00000000000001421, 0.000000000000000000 ) ) ;
#6980 = CARTESIAN_POINT ( 'NONE',  ( 7.236395654485755280, 4.724999997268803043, 22.27133577429736988 ) ) ;
#6981 = CARTESIAN_POINT ( 'NONE',  ( -7.236395654485757944, 9.224999997268806595, -22.27133577429736988 ) ) ;
#6982 = CARTESIAN_POINT ( 'NONE',  ( 27.16883889988624290, 24.17500000273117777, 19.73931689729373673 ) ) ;
#6983 = CARTESIAN_POINT ( 'NONE',  ( -26.29305231718579350, 26.30000000546236905, -19.10302069950537884 ) ) ;
#6984 = CARTESIAN_POINT ( 'NONE',  ( -32.50000000000000000, 66.10000000000000853, 10.55989012756946366 ) ) ;
#6985 = CARTESIAN_POINT ( 'NONE',  ( 32.50000000000000000, 47.60000000546239818, -10.55989012756945833 ) ) ;
#6986 = CARTESIAN_POINT ( 'NONE',  ( -1.778240108872766143E-15, 4.000000005462373664, -32.49999999999999289 ) ) ;
#6987 = CARTESIAN_POINT ( 'NONE',  ( -15.04653450569291984, 63.99777750092396644, 25.98046417659859486 ) ) ;
#6988 = CARTESIAN_POINT ( 'NONE',  ( -27.16883889988624290, 37.17500000273118843, -19.73931689729374028 ) ) ;
#6989 = CARTESIAN_POINT ( 'NONE',  ( 13.91746824999999532, 80.47500000273119269, -4.522059556121118540 ) ) ;
#6990 = CARTESIAN_POINT ( 'NONE',  ( -30.02300923189239867, 28.75781249999999645, 2.654126918244514854E-13 ) ) ;
#6991 = AXIS2_PLACEMENT_3D ( 'NONE', #29401, #21525, #24753 ) ;
#6992 = CARTESIAN_POINT ( 'NONE',  ( -23.41746825000000243, 16.02499999726881086, -7.608796670333730638 ) ) ;
#6993 = CARTESIAN_POINT ( 'NONE',  ( 26.29305231718578995, 15.19999999999999218, -19.10302069950538240 ) ) ;
#6994 = CARTESIAN_POINT ( 'NONE',  ( -7.570916362186215665, 15.39999999999999680, 23.30088464923126423 ) ) ;
#6995 = CARTESIAN_POINT ( 'NONE',  ( 14.01125832528330051, 39.92409749907602645, 24.18731323226221974 ) ) ;
#6996 = CARTESIAN_POINT ( 'NONE',  ( -33.58253175000000113, 55.02500000273118985, -10.91162601494193218 ) ) ;
#6997 = CARTESIAN_POINT ( 'NONE',  ( 27.16883889988624290, 64.17500000273116711, 19.73931689729373673 ) ) ;
#6998 = CARTESIAN_POINT ( 'NONE',  ( 6.486482029760648627E-15, 49.87500000273119838, 35.31076352940722529 ) ) ;
#6999 = CARTESIAN_POINT ( 'NONE',  ( 18.94512977948575738, 14.42499999726881654, 13.76444248337723408 ) ) ;
#7000 = CARTESIAN_POINT ( 'NONE',  ( 3.245314017740486554E-15, 70.00000000000000000, -26.50000000000000355 ) ) ;
#7001 = CARTESIAN_POINT ( 'NONE',  ( -10.04305231718579172, 49.60000000000000853, -30.90933677959248982 ) ) ;
#7002 = CARTESIAN_POINT ( 'NONE',  ( 14.01125832528286352, 45.09152750092398065, -24.18731323226246843 ) ) ;
#7003 = CARTESIAN_POINT ( 'NONE',  ( 20.08610463437158344, 63.20000000546237118, 27.64615127144129403 ) ) ;
#7004 = CARTESIAN_POINT ( 'NONE',  ( 3.880418787951134707, 3.551254281546844194, 24.50000000000000000 ) ) ;
#7005 = CARTESIAN_POINT ( 'NONE',  ( -2.162160676586881955E-15, 22.62500000273119127, -35.31076352940723240 ) ) ;
#7006 = CARTESIAN_POINT ( 'NONE',  ( 26.29305231718579350, 66.79999999999999716, 19.10302069950537529 ) ) ;
#7007 = LINE ( 'NONE', #6836, #33561 ) ;
#7008 = CARTESIAN_POINT ( 'NONE',  ( 15.04653450569339945, 63.98659749907601935, 25.98046417659831775 ) ) ;
#7009 = CARTESIAN_POINT ( 'NONE',  ( -10.04305231718579172, 44.10000000546236976, -30.90933677959248982 ) ) ;
#7010 = CARTESIAN_POINT ( 'NONE',  ( 2.375766604868043252, 71.69874572391555034, -14.99999999999999822 ) ) ;
#7011 = CARTESIAN_POINT ( 'NONE',  ( -27.16883889988624290, 30.92500000273118488, -19.73931689729374028 ) ) ;
#7012 = CARTESIAN_POINT ( 'NONE',  ( -19.09188309203660694, 38.64062500000000000, 19.09188309203694800 ) ) ;
#7013 = VERTEX_POINT ( 'NONE', #8914 ) ;
#7014 = CARTESIAN_POINT ( 'NONE',  ( 33.58253175000000113, 68.12500000273118417, -4.112674001490185761E-15 ) ) ;
#7015 = CARTESIAN_POINT ( 'NONE',  ( 7.505752307973351023, 38.06770833333332860, 28.01184896238290278 ) ) ;
#7016 = CIRCLE ( 'NONE', #3191, 24.49999999999999645 ) ;
#7017 = CARTESIAN_POINT ( 'NONE',  ( 5.779280353836490358E-15, 3.000000005462374109, 32.49999999999999289 ) ) ;
#7018 = ORIENTED_EDGE ( 'NONE', *, *, #2332, .T. ) ;
#7019 = CARTESIAN_POINT ( 'NONE',  ( 30.02300923189239867, 55.97694416759064495, 0.04044903254992252006 ) ) ;
#7020 = CARTESIAN_POINT ( 'NONE',  ( -7.025853678916393008, 60.41704833425730214, 26.06988505166735592 ) ) ;
#7021 = CARTESIAN_POINT ( 'NONE',  ( -33.58253175000000113, 13.22500000273119802, 10.91162601494193929 ) ) ;
#7022 = CARTESIAN_POINT ( 'NONE',  ( 7.468012846824281681, 18.01003499907601935, -28.02196122052058058 ) ) ;
#7023 = CARTESIAN_POINT ( 'NONE',  ( 15.00000000000000000, 79.35000000546240528, -4.873795443493596835 ) ) ;
#7024 = CARTESIAN_POINT ( 'NONE',  ( 10.37757302488624767, 39.97500000273118559, 31.93888565452638417 ) ) ;
#7025 = CARTESIAN_POINT ( 'NONE',  ( -26.29305231718578995, 42.70000000546237118, 19.10302069950538595 ) ) ;
#7026 = CARTESIAN_POINT ( 'NONE',  ( 9.270509831248423538, 81.29999999999999716, -12.75976212528059861 ) ) ;
#7027 = CARTESIAN_POINT ( 'NONE',  ( 33.58253175000000113, 30.12500000273118772, -4.112674001490185761E-15 ) ) ;
#7028 = CARTESIAN_POINT ( 'NONE',  ( 7.313012447739250820E-14, 13.24999999453762456, 24.50000000000000000 ) ) ;
#7029 = CARTESIAN_POINT ( 'NONE',  ( -33.58253175000000113, 55.47500000273119980, 10.91162601494193929 ) ) ;
#7030 = CARTESIAN_POINT ( 'NONE',  ( 32.50000000000000000, 36.99999999999999289, -3.980102097228898626E-15 ) ) ;
#7031 = CARTESIAN_POINT ( 'NONE',  ( -26.29305231718578995, 34.20000000000000995, 19.10302069950538595 ) ) ;
#7032 = CARTESIAN_POINT ( 'NONE',  ( 18.94512977948575738, 16.42499999726882010, 13.76444248337723408 ) ) ;
#7033 = CARTESIAN_POINT ( 'NONE',  ( -33.58253175000000113, 77.22500000273117848, 10.91162601494193929 ) ) ;
#7034 = CARTESIAN_POINT ( 'NONE',  ( -13.17636326499370014, 67.00000000000004263, 29.96527208688299027 ) ) ;
#7035 = CARTESIAN_POINT ( 'NONE',  ( -10.04305231718579172, 20.10000000546238752, -30.90933677959248982 ) ) ;
#7036 = CARTESIAN_POINT ( 'NONE',  ( 27.16883889988624290, 66.17500000273118133, 19.73931689729373673 ) ) ;
#7037 = CARTESIAN_POINT ( 'NONE',  ( -15.00000000000000000, 80.15000000546237402, -4.873795443493594171 ) ) ;
#7038 = EDGE_CURVE ( 'NONE', #15614, #24433, #11329, .T. ) ;
#7039 = VERTEX_POINT ( 'NONE', #1349 ) ;
#7040 = CARTESIAN_POINT ( 'NONE',  ( -33.58253175000000113, 17.02500000273118985, -10.91162601494193218 ) ) ;
#7041 = CARTESIAN_POINT ( 'NONE',  ( -7.570916362186215665, 9.149999994537639125, 23.30088464923126423 ) ) ;
#7042 = CARTESIAN_POINT ( 'NONE',  ( -13.94119854578936923, 17.01861083425731280, -24.22776226481241224 ) ) ;
#7043 = CARTESIAN_POINT ( 'NONE',  ( 20.08610463437157279, 47.29999999999999005, -27.64615127144129758 ) ) ;
#7044 = CARTESIAN_POINT ( 'NONE',  ( 27.16883889988623935, 40.32500000273118701, -19.73931689729374384 ) ) ;
#7045 = CARTESIAN_POINT ( 'NONE',  ( 33.58253175000000823, 2.275000002731194293, 10.91162601494192863 ) ) ;
#7046 = CARTESIAN_POINT ( 'NONE',  ( 33.58253175000000113, 56.37500000273119838, -4.112674001490185761E-15 ) ) ;
#7047 = CARTESIAN_POINT ( 'NONE',  ( 28.00173670424549499, 45.80767333425730925, 7.543491769121417612 ) ) ;
#7048 = CARTESIAN_POINT ( 'NONE',  ( 24.50000000000000000, 15.89999999999998970, 7.960532557706212486 ) ) ;
#7049 = CARTESIAN_POINT ( 'NONE',  ( -26.02091320914878025, 37.91888916574269075, -14.97647472619899389 ) ) ;
#7050 = CARTESIAN_POINT ( 'NONE',  ( -26.29305231718578995, 62.70000000546237118, 19.10302069950538595 ) ) ;
#7051 = CARTESIAN_POINT ( 'NONE',  ( 8.601468415847516980, 74.17500000273122396, -11.83890561707634781 ) ) ;
#7052 = CARTESIAN_POINT ( 'NONE',  ( 7.025853678916867295, 64.12982666574268364, 26.06988505166722803 ) ) ;
#7053 = DIRECTION ( 'NONE',  ( 0.000000000000000000, 0.000000000000000000, 1.000000000000000000 ) ) ;
#7054 = CARTESIAN_POINT ( 'NONE',  ( -26.29305231718579350, 74.30000000546237970, -19.10302069950537884 ) ) ;
#7055 = CARTESIAN_POINT ( 'NONE',  ( 2.375766604868043252, 79.44874571845312516, -14.99999999999999822 ) ) ;
#7056 = CARTESIAN_POINT ( 'NONE',  ( 20.75514604977249178, 40.07500000273118701, 28.56700777964553950 ) ) ;
#7057 =( BOUNDED_CURVE ( )  B_SPLINE_CURVE ( 2, ( #8421, #16836, #8592, #3783, #9094, #32265, #6184, #14254, #11670, #22151, #19576, #6020, #30024 ),
 .UNSPECIFIED., .F., .T. ) 
 B_SPLINE_CURVE_WITH_KNOTS ( ( 3, 2, 2, 2, 2, 2, 3 ),
 ( 0.6388888888888889506, 0.6444444444444444864, 0.6555555555555555580, 0.6666666666666666297, 0.6777777777777778123, 0.6888888888888888840, 0.6944444444444444198 ),
 .UNSPECIFIED. ) 
 CURVE ( )  GEOMETRIC_REPRESENTATION_ITEM ( )  RATIONAL_B_SPLINE_CURVE ( ( 0.9755282581475768211, 0.9755282581475770431, 1.000000000000000000, 0.9510565162951535312, 1.000000000000000000, 0.9510565162951535312, 1.000000000000000000, 0.9510565162951535312, 1.000000000000000000, 0.9510565162951535312, 1.000000000000000000, 0.9755282581475768211, 0.9755282581475768211 ) ) 
 REPRESENTATION_ITEM ( '' )  );
#7058 = CARTESIAN_POINT ( 'NONE',  ( -14.47279130897152299, 10.42499999726881121, 19.92008829642072243 ) ) ;
#7059 = ORIENTED_EDGE ( 'NONE', *, *, #8037, .T. ) ;
#7060 = CARTESIAN_POINT ( 'NONE',  ( 10.37757302488624056, 76.77500000273118985, -31.93888565452638417 ) ) ;
#7061 = CARTESIAN_POINT ( 'NONE',  ( -32.50000000000000000, 26.40000000546236336, -10.55989012756945478 ) ) ;
#7062 = ORIENTED_EDGE ( 'NONE', *, *, #1694, .F. ) ;
#7063 = CARTESIAN_POINT ( 'NONE',  ( 26.00068869287340334, 47.37760416666666430, -15.01150461594642316 ) ) ;
#7064 = CARTESIAN_POINT ( 'NONE',  ( -20.08610463437157989, 64.20000000546238539, -27.64615127144129758 ) ) ;
#7065 = VERTEX_POINT ( 'NONE', #11829 ) ;
#7066 = CARTESIAN_POINT ( 'NONE',  ( 2.489536152421872915E-14, 74.00000000546238255, -32.49999999999999289 ) ) ;
#7067 = CARTESIAN_POINT ( 'NONE',  ( -10.37757302488624411, 50.72500000273119980, -31.93888565452638417 ) ) ;
#7068 = DIRECTION ( 'NONE',  ( -0.000000000000000000, -1.000000000000000000, -0.000000000000000000 ) ) ;
#7069 = CARTESIAN_POINT ( 'NONE',  ( 10.04305231718578817, 7.900000005462370467, -30.90933677959249337 ) ) ;
#7070 = CARTESIAN_POINT ( 'NONE',  ( -15.00000000000000000, 78.00000000000001421, 0.000000000000000000 ) ) ;
#7071 = CYLINDRICAL_SURFACE ( 'NONE', #10057, 32.50000000000000000 ) ;
#7072 = CARTESIAN_POINT ( 'NONE',  ( 6.277390505771533514E-15, 54.49999999999999289, 34.17252228774368916 ) ) ;
#7073 = CARTESIAN_POINT ( 'NONE',  ( -20.08610463437157989, 13.70000000000000462, -27.64615127144129758 ) ) ;
#7074 = CARTESIAN_POINT ( 'NONE',  ( 33.58253175000000823, 16.27500000273118630, 10.91162601494192863 ) ) ;
#7075 = CARTESIAN_POINT ( 'NONE',  ( -1.778240108872766143E-15, 62.00000000546238255, -32.49999999999999289 ) ) ;
#7076 = CARTESIAN_POINT ( 'NONE',  ( 6.950374756619257965, 28.32253499907601579, -26.09010956794244507 ) ) ;
#7077 = CARTESIAN_POINT ( 'NONE',  ( 8.601468415847520532, 76.07500000273118701, 11.83890561707634781 ) ) ;
#7078 = CARTESIAN_POINT ( 'NONE',  ( -32.50000000000000000, 55.90000000000000568, -10.55989012756945300 ) ) ;
#7079 = CARTESIAN_POINT ( 'NONE',  ( 30.20345010595902480, 52.00000000000000711, 14.84467937978581453 ) ) ;
#7080 = CARTESIAN_POINT ( 'NONE',  ( -32.50000000000000000, 6.099999999999996092, 10.55989012756946366 ) ) ;
#7081 = EDGE_LOOP ( 'NONE', ( #14832, #31510, #31038, #3606 ) ) ;
#7082 = CARTESIAN_POINT ( 'NONE',  ( -23.41746824999999887, 16.12499999726882294, -2.867812753649727150E-15 ) ) ;
#7083 = CARTESIAN_POINT ( 'NONE',  ( 13.91746825000000065, 71.77500000273120406, 4.522059556121114987 ) ) ;
#7084 = CARTESIAN_POINT ( 'NONE',  ( 24.20753774853731244, 54.25260416666666430, -13.97622843553632599 ) ) ;
#7085 = CARTESIAN_POINT ( 'NONE',  ( -33.58253175000000113, 59.02500000273120406, -10.91162601494193218 ) ) ;
#7086 = CARTESIAN_POINT ( 'NONE',  ( 33.58253175000000823, 24.27500000273120051, 10.91162601494192863 ) ) ;
#7087 = CARTESIAN_POINT ( 'NONE',  ( -10.37757302488624411, 8.975000002731201576, -31.93888565452638417 ) ) ;
#7088 = CARTESIAN_POINT ( 'NONE',  ( -27.16883889988624290, 3.175000002731187543, -19.73931689729374028 ) ) ;
#7089 = CARTESIAN_POINT ( 'NONE',  ( 7.468012846824777284, 18.88059000092397355, 28.02196122052045268 ) ) ;
#7090 = CARTESIAN_POINT ( 'NONE',  ( -20.50609665441004736, 67.00000000000000000, -20.50609665440969565 ) ) ;
#7091 = CARTESIAN_POINT ( 'NONE',  ( 10.04305231718579705, 77.10000000546239107, 30.90933677959248982 ) ) ;
#7092 = CARTESIAN_POINT ( 'NONE',  ( 3.980102097228898626E-15, 80.00000000000001421, 32.50000000000000000 ) ) ;
#7093 = CARTESIAN_POINT ( 'NONE',  ( -32.50000000000000000, 44.00000000000000000, 0.000000000000000000 ) ) ;
#7094 = CARTESIAN_POINT ( 'NONE',  ( -20.75514604977248823, 42.82500000273120122, -28.56700777964554305 ) ) ;
#7095 = CARTESIAN_POINT ( 'NONE',  ( 1.507698388325705758E-15, 3.124999997268809615, -24.62258325217400312 ) ) ;
#7096 = PRODUCT ( 'lock nut', 'lock nut', '', ( #31185 ) ) ;
#7097 = CARTESIAN_POINT ( 'NONE',  ( 9.270509831248421762, 79.30000000000003979, -12.75976212528059861 ) ) ;
#7098 = EDGE_LOOP ( 'NONE', ( #263, #21688, #16240, #27202 ) ) ;
#7099 = CARTESIAN_POINT ( 'NONE',  ( -27.16883889988623935, 61.57500000273117990, 19.73931689729374739 ) ) ;
#7100 = CARTESIAN_POINT ( 'NONE',  ( 20.08610463437157279, 43.30000000000000426, -27.64615127144129758 ) ) ;
#7101 = CARTESIAN_POINT ( 'NONE',  ( -23.41746825000000598, 9.724999997268804819, 7.608796670333726198 ) ) ;
#7102 = CARTESIAN_POINT ( 'NONE',  ( 19.06425588902592239, 35.78163166759063074, 19.11951029504763611 ) ) ;
#7103 = ORIENTED_EDGE ( 'NONE', *, *, #5280, .T. ) ;
#7104 = CARTESIAN_POINT ( 'NONE',  ( -33.58253175000000113, 31.12500000273120548, 0.000000000000000000 ) ) ;
#7105 = CARTESIAN_POINT ( 'NONE',  ( 0.000000000000000000, 80.00000000000001421, 0.000000000000000000 ) ) ;
#7106 = EDGE_LOOP ( 'NONE', ( #29800, #13825, #19104, #26534, #8996, #33088, #13540, #13742, #646, #6132, #21227, #23735, #21601, #23397, #23755, #21533, #24778, #19027, #27832, #29931, #3526, #13990 ) ) ;
#7107 = DIRECTION ( 'NONE',  ( 1.000000000000000000, 0.000000000000000000, -0.000000000000000000 ) ) ;
#7108 = CARTESIAN_POINT ( 'NONE',  ( 33.58253175000000113, 68.12500000273119838, -4.112674001490185761E-15 ) ) ;
#7109 = CARTESIAN_POINT ( 'NONE',  ( -26.00068869287340334, 42.22135416666666430, 15.01150461594643382 ) ) ;
#7110 = CARTESIAN_POINT ( 'NONE',  ( 24.50000000000000355, 11.90000000000000391, 7.960532557706212486 ) ) ;
#7111 = CARTESIAN_POINT ( 'NONE',  ( -7.236395654485763274, 4.524999997268825069, 22.27133577429736633 ) ) ;
#7112 = CARTESIAN_POINT ( 'NONE',  ( -20.75514604977248112, 7.425000002731177773, 28.56700777964554661 ) ) ;
#7113 = CARTESIAN_POINT ( 'NONE',  ( -3.880418787951127602, 6.301254276084462091, -24.50000000000000000 ) ) ;
#7114 = CARTESIAN_POINT ( 'NONE',  ( 25.98046417659831775, 52.81472249907603356, -15.04653450569338879 ) ) ;
#7115 = CARTESIAN_POINT ( 'NONE',  ( -12.13525491562421088, 73.80000000000001137, -8.816778784387096835 ) ) ;
#7116 = CARTESIAN_POINT ( 'NONE',  ( -7.505752307973343918, 60.41145833333332149, -28.01184896238290989 ) ) ;
#7117 = CARTESIAN_POINT ( 'NONE',  ( 32.50000000000000711, 54.90000000000001279, 10.55989012756945122 ) ) ;
#7118 = CARTESIAN_POINT ( 'NONE',  ( -15.00000000000000000, 74.35000000546236265, 4.873795443493597723 ) ) ;
#7119 = CARTESIAN_POINT ( 'NONE',  ( 19.82091636218621034, 11.54999999453762349, 14.40073868116559730 ) ) ;
#7120 = CARTESIAN_POINT ( 'NONE',  ( -15.00000000000000000, 80.15000000546234560, -4.873795443493594171 ) ) ;
#7121 = CARTESIAN_POINT ( 'NONE',  ( 19.09188309203694800, 20.59374999999999645, 19.09188309203660694 ) ) ;
#7122 = ADVANCED_FACE ( 'NONE', ( #22306 ), #9245, .T. ) ;
#7123 = CARTESIAN_POINT ( 'NONE',  ( 6.486482029760649416E-15, 31.62500000273119483, 35.31076352940723240 ) ) ;
#7124 = FACE_OUTER_BOUND ( 'NONE', #28383, .T. ) ;
#7125 = CARTESIAN_POINT ( 'NONE',  ( 20.75514604977248467, 42.67500000273119554, -28.56700777964554305 ) ) ;
#7126 = CARTESIAN_POINT ( 'NONE',  ( 20.75514604977248467, 24.67500000273118488, -28.56700777964554305 ) ) ;
#7127 = CARTESIAN_POINT ( 'NONE',  ( -1.137977401836464321E-14, 52.00000000000000711, 46.18802153517007270 ) ) ;
#7128 = EDGE_CURVE ( 'NONE', #8282, #7233, #24701, .T. ) ;
#7129 = CARTESIAN_POINT ( 'NONE',  ( -32.50000000000000000, 8.600000005462376862, 10.55989012756946366 ) ) ;
#7130 = CARTESIAN_POINT ( 'NONE',  ( 8.891200544363830713E-16, 81.50000000000001421, -15.00000000000000000 ) ) ;
#7131 = CARTESIAN_POINT ( 'NONE',  ( -10.04305231718579172, 59.60000000000000142, -30.90933677959248982 ) ) ;
#7132 = CARTESIAN_POINT ( 'NONE',  ( -23.41746824999999887, 11.52499999726880553, -7.608796670333730638 ) ) ;
#7133 = CARTESIAN_POINT ( 'NONE',  ( 33.58253175000000113, 66.12500000273119838, -4.112674001490185761E-15 ) ) ;
#7134 = CARTESIAN_POINT ( 'NONE',  ( 18.94512977948575738, 2.924999997268806773, 13.76444248337723408 ) ) ;
#7135 = CARTESIAN_POINT ( 'NONE',  ( -26.09010956794245217, 41.21315999907602645, -6.950374756619243755 ) ) ;
#7136 = CARTESIAN_POINT ( 'NONE',  ( -33.58253175000000113, 1.125000002731191273, 0.000000000000000000 ) ) ;
#7137 = CARTESIAN_POINT ( 'NONE',  ( 33.58253175000000113, 16.22500000273118914, -10.91162601494193574 ) ) ;
#7138 = CARTESIAN_POINT ( 'NONE',  ( -23.41746825000000598, 12.22499999726881370, 7.608796670333726198 ) ) ;
#7139 = CARTESIAN_POINT ( 'NONE',  ( -19.09188309203694445, 67.00000000000000000, -19.09188309203661049 ) ) ;
#7140 = ORIENTED_EDGE ( 'NONE', *, *, #12795, .T. ) ;
#7141 = CARTESIAN_POINT ( 'NONE',  ( 6.486482029760649416E-15, 47.62500000273118417, 35.31076352940723240 ) ) ;
#7142 = CARTESIAN_POINT ( 'NONE',  ( 27.16883889988623935, 22.57500000273120122, -19.73931689729374384 ) ) ;
#7143 = EDGE_LOOP ( 'NONE', ( #3770, #3199, #16290, #18594 ) ) ;
#7144 = CARTESIAN_POINT ( 'NONE',  ( 7.505752307972854531, 29.76041666666666430, -28.01184896238303423 ) ) ;
#7145 = CARTESIAN_POINT ( 'NONE',  ( 30.02300923189239867, 31.91444416759064495, 0.04044903254992252006 ) ) ;
#7146 = DIRECTION ( 'NONE',  ( -1.000000000000000000, 0.000000000000000000, 0.000000000000000000 ) ) ;
#7147 = CARTESIAN_POINT ( 'NONE',  ( -8.891200544363830713E-16, 77.50000000000000000, -15.00000000000000000 ) ) ;
#7148 = CARTESIAN_POINT ( 'NONE',  ( -18.94512977948576093, 2.324999997268817342, 13.76444248337722698 ) ) ;
#7149 = CARTESIAN_POINT ( 'NONE',  ( -23.41746824999999887, 11.62499999726881938, -2.867812753649727150E-15 ) ) ;
#7150 = CARTESIAN_POINT ( 'NONE',  ( -20.75514604977248823, 21.07500000273118346, -28.56700777964554305 ) ) ;
#7151 = CARTESIAN_POINT ( 'NONE',  ( 26.29305231718578995, 23.70000000546237828, -19.10302069950538240 ) ) ;
#7152 = CARTESIAN_POINT ( 'NONE',  ( 32.50000000000000000, 65.10000000000000853, -10.55989012756945833 ) ) ;
#7153 = CARTESIAN_POINT ( 'NONE',  ( 7.570916362186207671, 11.34999999453761887, 23.30088464923126779 ) ) ;
#7154 = CARTESIAN_POINT ( 'NONE',  ( -2.174791880140518163, 73.99999999999997158, 14.05554496361005334 ) ) ;
#7155 = CARTESIAN_POINT ( 'NONE',  ( 28.02196122052045268, 62.70871500092398065, -7.468012846824774620 ) ) ;
#7156 = CARTESIAN_POINT ( 'NONE',  ( -20.75514604977248823, 33.07500000273117990, -28.56700777964554305 ) ) ;
#7157 = CARTESIAN_POINT ( 'NONE',  ( -1.778240108872766143E-15, 32.00000000546237544, -32.49999999999999289 ) ) ;
#7158 = CARTESIAN_POINT ( 'NONE',  ( 28.01184896238304134, 27.18229166666666430, 7.505752307972846538 ) ) ;
#7159 = DIRECTION ( 'NONE',  ( 0.000000000000000000, 0.000000000000000000, 1.000000000000000000 ) ) ;
#7160 = CARTESIAN_POINT ( 'NONE',  ( -7.570916362186210335, 0.5999999999999894307, -23.30088464923126779 ) ) ;
#7161 = CARTESIAN_POINT ( 'NONE',  ( -10.04305231718578462, 8.400000000000018119, 30.90933677959249337 ) ) ;
#7162 = CARTESIAN_POINT ( 'NONE',  ( 24.50000000000000355, 15.89999999999999147, 7.960532557706212486 ) ) ;
#7163 = EDGE_CURVE ( 'NONE', #16413, #29502, #32254, .T. ) ;
#7164 = CARTESIAN_POINT ( 'NONE',  ( 27.95245687107223276, 53.10118083240936215, -0.04044903255042905932 ) ) ;
#7165 = CARTESIAN_POINT ( 'NONE',  ( -27.16883889988623935, 59.32500000273119412, 19.73931689729374739 ) ) ;
#7166 = CARTESIAN_POINT ( 'NONE',  ( -20.75514604977248823, 59.07500000273119412, -28.56700777964554305 ) ) ;
#7167 = CARTESIAN_POINT ( 'NONE',  ( 6.486482029760648627E-15, 43.87500000273118417, 35.31076352940722529 ) ) ;
#7168 = CARTESIAN_POINT ( 'NONE',  ( 14.47279130897151767, 16.32499999726882933, 19.92008829642072953 ) ) ;
#7169 = CARTESIAN_POINT ( 'NONE',  ( 7.570916362186207671, 9.599999999999997868, 23.30088464923126779 ) ) ;
#7170 = DIRECTION ( 'NONE',  ( -0.000000000000000000, -1.000000000000000000, -0.000000000000000000 ) ) ;
#7171 = CARTESIAN_POINT ( 'NONE',  ( -6.950374756619716266, 44.66184000092397355, -26.09010956794232428 ) ) ;
#7172 = CARTESIAN_POINT ( 'NONE',  ( -3.880418787951146697, 4.301254276084477191, -24.49999999999999645 ) ) ;
#7173 = DIRECTION ( 'NONE',  ( 0.000000000000000000, -1.000000000000000000, 0.000000000000000000 ) ) ;
#7174 = CARTESIAN_POINT ( 'NONE',  ( -20.75514604977248823, 22.82500000273118701, -28.56700777964554305 ) ) ;
#7175 = CARTESIAN_POINT ( 'NONE',  ( 0.000000000000000000, 80.00000000000001421, 0.000000000000000000 ) ) ;
#7176 = CARTESIAN_POINT ( 'NONE',  ( 32.50000000000000000, 53.09999999999998010, -10.55989012756945833 ) ) ;
#7177 = CARTESIAN_POINT ( 'NONE',  ( 40.00000000000000000, 52.00000000000000711, -23.09401076758505766 ) ) ;
#7178 = CARTESIAN_POINT ( 'NONE',  ( -14.97647472619899389, 64.55951416574268364, 26.02091320914878025 ) ) ;
#7179 = CARTESIAN_POINT ( 'NONE',  ( -32.50000000000000000, 40.60000000546239107, 10.55989012756946366 ) ) ;
#7180 = CARTESIAN_POINT ( 'NONE',  ( 0.000000000000000000, 80.00000000000001421, -32.50000000000000000 ) ) ;
#7181 = CARTESIAN_POINT ( 'NONE',  ( -33.58253175000000113, 35.12500000273119127, 0.000000000000000000 ) ) ;
#7182 = CARTESIAN_POINT ( 'NONE',  ( -20.75514604977248112, 63.67500000273116711, 28.56700777964554661 ) ) ;
#7183 = CARTESIAN_POINT ( 'NONE',  ( -13.97622843553632421, 32.76822916666666430, -24.20753774853731599 ) ) ;
#7184 = ORIENTED_EDGE ( 'NONE', *, *, #26475, .T. ) ;
#7185 = CARTESIAN_POINT ( 'NONE',  ( 10.37757302488624056, 66.52500000273118985, -31.93888565452638417 ) ) ;
#7186 = CARTESIAN_POINT ( 'NONE',  ( 2.740863092043355209E-13, 41.64843750000000000, 30.02300923189239512 ) ) ;
#7187 = DIRECTION ( 'NONE',  ( 0.000000000000000000, 1.000000000000000000, 0.000000000000000000 ) ) ;
#7188 = ORIENTED_EDGE ( 'NONE', *, *, #16049, .F. ) ;
#7189 = CARTESIAN_POINT ( 'NONE',  ( 20.53372385742072481, 55.54725666759064495, -20.47846945139902175 ) ) ;
#7190 = CARTESIAN_POINT ( 'NONE',  ( 26.06988505166735592, 62.99517333425730214, 7.025853678916393896 ) ) ;
#7191 = CARTESIAN_POINT ( 'NONE',  ( -20.75514604977248823, 12.82500000273119589, -28.56700777964554305 ) ) ;
#7192 = CARTESIAN_POINT ( 'NONE',  ( -7.468012846824272799, 19.72878499907601935, 28.02196122052058413 ) ) ;
#7193 = CARTESIAN_POINT ( 'NONE',  ( -5.147494310547430452, 45.55125428154684641, -32.49999999999999289 ) ) ;
#7194 = CARTESIAN_POINT ( 'NONE',  ( -10.37757302488623701, 41.77500000273118275, 31.93888565452638417 ) ) ;
#7195 = VECTOR ( 'NONE', #19077, 1000.000000000000000 ) ;
#7196 = CARTESIAN_POINT ( 'NONE',  ( 20.08610463437157279, 45.80000000546240102, -27.64615127144129758 ) ) ;
#7197 = CARTESIAN_POINT ( 'NONE',  ( 9.270509831248423538, 79.30000000000001137, -12.75976212528059861 ) ) ;
#7198 = CARTESIAN_POINT ( 'NONE',  ( -20.75514604977248823, 22.82500000273118701, -28.56700777964554305 ) ) ;
#7199 = CARTESIAN_POINT ( 'NONE',  ( 24.50000000000000000, 13.64999999453761781, 7.960532557706212486 ) ) ;
#7200 = CARTESIAN_POINT ( 'NONE',  ( 10.37757302488624056, 58.77500000273119696, -31.93888565452638417 ) ) ;
#7201 = CARTESIAN_POINT ( 'NONE',  ( 10.04305231718579705, 26.59999999999999787, 30.90933677959248982 ) ) ;
#7202 = CARTESIAN_POINT ( 'NONE',  ( 32.50000000000000000, 26.99999999999999645, -3.980102097228898626E-15 ) ) ;
#7203 = CARTESIAN_POINT ( 'NONE',  ( -14.47279130897151589, 17.32499999726879381, -19.92008829642072598 ) ) ;
#7204 = CARTESIAN_POINT ( 'NONE',  ( 20.75514604977249178, 73.82500000273121543, 28.56700777964553950 ) ) ;
#7205 = PLANE ( 'NONE',  #30991 ) ;
#7206 = VECTOR ( 'NONE', #27584, 1000.000000000000000 ) ;
#7207 = CARTESIAN_POINT ( 'NONE',  ( -24.50000000000000000, 15.00000000000001421, -3.000384657911015469E-15 ) ) ;
#7208 = CARTESIAN_POINT ( 'NONE',  ( 10.37757302488624056, 60.77500000273117564, -31.93888565452638417 ) ) ;
#7209 = CARTESIAN_POINT ( 'NONE',  ( 15.00000000000000000, 79.25000000546239676, -1.836970198721029589E-15 ) ) ;
#7210 = ORIENTED_EDGE ( 'NONE', *, *, #15759, .T. ) ;
#7211 = CARTESIAN_POINT ( 'NONE',  ( -27.16883889988624290, 20.92500000273117422, -19.73931689729374028 ) ) ;
#7212 = CARTESIAN_POINT ( 'NONE',  ( 24.50000000000000000, 7.749999994537626336, 0.000000000000000000 ) ) ;
#7213 = CARTESIAN_POINT ( 'NONE',  ( 27.95245687107223986, 18.16444416759064140, 0.04044903254993640479 ) ) ;
#7214 = DIRECTION ( 'NONE',  ( -0.8660254037844410391, 0.4999999999999958367, 0.000000000000000000 ) ) ;
#7215 = CARTESIAN_POINT ( 'NONE',  ( -33.58253175000000113, 39.12500000273118417, 0.000000000000000000 ) ) ;
#7216 = CARTESIAN_POINT ( 'NONE',  ( -20.75514604977248112, 3.675000002731193316, 28.56700777964554661 ) ) ;
#7217 = CARTESIAN_POINT ( 'NONE',  ( -2.162160676586882350E-15, 58.87500000273117706, -35.31076352940722529 ) ) ;
#7218 = CARTESIAN_POINT ( 'NONE',  ( -7.468012846824771955, 48.09934000092398065, -28.02196122052045624 ) ) ;
#7219 = CARTESIAN_POINT ( 'NONE',  ( 0.04044903255045854962, 40.21055583240935505, 30.02300923189239867 ) ) ;
#7220 = CARTESIAN_POINT ( 'NONE',  ( 26.29305231718579350, 59.30000000546238681, 19.10302069950537529 ) ) ;
#7221 = CARTESIAN_POINT ( 'NONE',  ( 2.688165632520823219E-15, 75.37500000273118417, 14.63369212191046387 ) ) ;
#7222 = CARTESIAN_POINT ( 'NONE',  ( -0.04044903255042732459, 62.55430583240935505, -27.95245687107223986 ) ) ;
#7223 = CARTESIAN_POINT ( 'NONE',  ( -23.41746824999999887, 2.124999997268811391, -2.867812753649727150E-15 ) ) ;
#7224 = CARTESIAN_POINT ( 'NONE',  ( -33.58253175000000113, 1.125000002731191273, 0.000000000000000000 ) ) ;
#7225 = CARTESIAN_POINT ( 'NONE',  ( 7.505752307972854531, 16.01041666666666075, -28.01184896238303423 ) ) ;
#7226 = CARTESIAN_POINT ( 'NONE',  ( 6.486482029760649416E-15, 33.87500000273118417, 35.31076352940723240 ) ) ;
#7227 = CARTESIAN_POINT ( 'NONE',  ( 18.94512977948575738, 10.92499999726881299, 13.76444248337723408 ) ) ;
#7228 = EDGE_LOOP ( 'NONE', ( #12075, #31969, #7184, #936 ) ) ;
#7229 = CARTESIAN_POINT ( 'NONE',  ( -10.37757302488623701, 77.77500000273118985, 31.93888565452638417 ) ) ;
#7230 = CARTESIAN_POINT ( 'NONE',  ( 26.29305231718578995, 25.70000000546239605, -19.10302069950538240 ) ) ;
#7231 = CARTESIAN_POINT ( 'NONE',  ( 28.01184896238304134, 47.80729166666666430, 7.505752307972846538 ) ) ;
#7232 = CARTESIAN_POINT ( 'NONE',  ( -2.092463501923844636E-15, 62.00000000546238255, -34.17252228774368916 ) ) ;
#7233 = VERTEX_POINT ( 'NONE', #6010 ) ;
#7234 = CARTESIAN_POINT ( 'NONE',  ( -33.58253175000000113, 47.02500000273116854, -10.91162601494193218 ) ) ;
#7235 = CARTESIAN_POINT ( 'NONE',  ( 7.236395654485755280, 18.22499999726881370, 22.27133577429736988 ) ) ;
#7236 = CARTESIAN_POINT ( 'NONE',  ( -20.08610463437157989, 4.200000005462371178, -27.64615127144129758 ) ) ;
#7237 = LINE ( 'NONE', #28183, #22903 ) ;
#7238 = CARTESIAN_POINT ( 'NONE',  ( 23.41746824999999887, 19.12499999726882649, 0.000000000000000000 ) ) ;
#7239 = CARTESIAN_POINT ( 'NONE',  ( -32.50000000000000000, 49.99999999999998579, 0.000000000000000000 ) ) ;
#7240 = CARTESIAN_POINT ( 'NONE',  ( 24.50000000000000000, 2.000000000000001776, 0.000000000000000000 ) ) ;
#7241 = CARTESIAN_POINT ( 'NONE',  ( -27.16883889988623935, 19.57500000273118701, 19.73931689729374739 ) ) ;
#7242 = VECTOR ( 'NONE', #6383, 1000.000000000000227 ) ;
#7243 = LINE ( 'NONE', #6906, #30440 ) ;
#7244 = CARTESIAN_POINT ( 'NONE',  ( -27.95245687107223986, 23.88243083240935505, 0.04044903255043252877 ) ) ;
#7245 = CARTESIAN_POINT ( 'NONE',  ( -13.91746824999999887, 81.37500000273118417, 0.000000000000000000 ) ) ;
#7246 = CARTESIAN_POINT ( 'NONE',  ( -1.089172066684569321E-14, 76.75000000546238255, 15.00000000000000000 ) ) ;
#7247 = CARTESIAN_POINT ( 'NONE',  ( -32.50000000000000000, 44.10000000000000142, 10.55989012756946366 ) ) ;
#7248 = CARTESIAN_POINT ( 'NONE',  ( 32.50000000000000711, 6.899999999999999467, 10.55989012756945122 ) ) ;
#7249 = ORIENTED_EDGE ( 'NONE', *, *, #33483, .T. ) ;
#7250 = CARTESIAN_POINT ( 'NONE',  ( -4.523095164977116484E-15, 16.62499999726881583, 24.62258325217400312 ) ) ;
#7251 = CARTESIAN_POINT ( 'NONE',  ( -23.41746825000000243, 5.724999997268815477, 7.608796670333725309 ) ) ;
#7252 = CARTESIAN_POINT ( 'NONE',  ( 6.988114217768294445, 48.38020833333332860, 26.07999730980477437 ) ) ;
#7253 = CARTESIAN_POINT ( 'NONE',  ( -20.75514604977248823, 58.82500000273117990, -28.56700777964554305 ) ) ;
#7254 = CARTESIAN_POINT ( 'NONE',  ( 10.37757302488624056, 22.77500000273117919, -31.93888565452638417 ) ) ;
#7255 = CARTESIAN_POINT ( 'NONE',  ( -20.75514604977248112, 9.675000002731193760, 28.56700777964554661 ) ) ;
#7256 = CARTESIAN_POINT ( 'NONE',  ( 6.988114217768294445, 27.75520833333332860, 26.07999730980477437 ) ) ;
#7257 = CARTESIAN_POINT ( 'NONE',  ( -28.02196122052045268, 16.30246500092397355, 7.468012846824790607 ) ) ;
#7258 = EDGE_CURVE ( 'NONE', #25648, #9464, #13557, .T. ) ;
#7259 = CARTESIAN_POINT ( 'NONE',  ( 20.50609665440969565, 64.42187499999998579, -20.50609665441004736 ) ) ;
#7260 = CARTESIAN_POINT ( 'NONE',  ( 32.50000000000000000, 77.60000000546239107, -10.55989012756945833 ) ) ;
#7261 =( BOUNDED_CURVE ( )  B_SPLINE_CURVE ( 2, ( #2912, #23679, #23852, #31556, #26418, #2400, #8053, #16133, #2576, #144, #13380, #5141, #316 ),
 .UNSPECIFIED., .F., .T. ) 
 B_SPLINE_CURVE_WITH_KNOTS ( ( 3, 2, 2, 2, 2, 2, 3 ),
 ( 0.03205128205128205537, 0.03333333333333333287, 0.03589743589743589480, 0.03846153846153846367, 0.04102564102564102561, 0.04358974358974358754, 0.04487179487179487197 ),
 .UNSPECIFIED. ) 
 CURVE ( )  GEOMETRIC_REPRESENTATION_ITEM ( )  RATIONAL_B_SPLINE_CURVE ( ( 0.9755282581475768211, 0.9755282581475768211, 1.000000000000000000, 0.9510565162951535312, 1.000000000000000000, 0.9510565162951535312, 1.000000000000000000, 0.9510565162951535312, 1.000000000000000000, 0.9510565162951535312, 1.000000000000000000, 0.9755282581475768211, 0.9755282581475768211 ) ) 
 REPRESENTATION_ITEM ( '' )  );
#7262 = CARTESIAN_POINT ( 'NONE',  ( 32.50000000000000711, 68.90000000000000568, 10.55989012756945122 ) ) ;
#7263 = CARTESIAN_POINT ( 'NONE',  ( -2.092463501923844636E-15, 39.50000000000000000, -34.17252228774368916 ) ) ;
#7264 = CARTESIAN_POINT ( 'NONE',  ( 33.58253175000000113, 42.12500000273116996, -4.112674001490185761E-15 ) ) ;
#7265 = CARTESIAN_POINT ( 'NONE',  ( 23.41746824999999887, 8.624999997268817609, 0.000000000000000000 ) ) ;
#7266 = ADVANCED_FACE ( 'NONE', ( #13910 ), #849, .F. ) ;
#7267 = EDGE_CURVE ( 'NONE', #26901, #24499, #7572, .T. ) ;
#7268 = CARTESIAN_POINT ( 'NONE',  ( 6.988114217768294445, 65.56770833333332860, 26.07999730980477437 ) ) ;
#7269 = EDGE_LOOP ( 'NONE', ( #26860, #29431, #13623, #3561 ) ) ;
#7270 = CARTESIAN_POINT ( 'NONE',  ( 33.58253175000000823, 52.27500000273118985, 10.91162601494192863 ) ) ;
#7271 = CARTESIAN_POINT ( 'NONE',  ( 26.29305231718579350, 42.80000000000000426, 19.10302069950537529 ) ) ;
#7272 = AXIS2_PLACEMENT_3D ( 'NONE', #23015, #21128, #7390 ) ;
#7273 = CARTESIAN_POINT ( 'NONE',  ( -6.950374756619716266, 44.66184000092397355, -26.09010956794232428 ) ) ;
#7274 = CARTESIAN_POINT ( 'NONE',  ( 33.58253175000000113, 76.37500000273116996, -4.112674001490185761E-15 ) ) ;
#7275 = EDGE_LOOP ( 'NONE', ( #1130, #10922, #15683, #27621 ) ) ;
#7276 = CARTESIAN_POINT ( 'NONE',  ( -20.75514604977248112, 31.42500000273120619, 28.56700777964554661 ) ) ;
#7277 = CARTESIAN_POINT ( 'NONE',  ( 28.01184896238290278, 13.14583333333332860, -7.505752307973347470 ) ) ;
#7278 = ORIENTED_EDGE ( 'NONE', *, *, #27657, .T. ) ;
#7279 = DIRECTION ( 'NONE',  ( -1.000000000000000000, -1.111257322145974683E-16, 0.000000000000000000 ) ) ;
#7280 = CARTESIAN_POINT ( 'NONE',  ( -33.58253175000000113, 67.22500000273117848, 10.91162601494193929 ) ) ;
#7281 = CARTESIAN_POINT ( 'NONE',  ( 15.01150461594596308, 43.65364583333332860, -26.00068869287367335 ) ) ;
#7282 = CARTESIAN_POINT ( 'NONE',  ( 7.570916362186207671, 13.60000000000000142, 23.30088464923126779 ) ) ;
#7283 = DIRECTION ( 'NONE',  ( 0.000000000000000000, 0.000000000000000000, -1.000000000000000000 ) ) ;
#7284 = CARTESIAN_POINT ( 'NONE',  ( 20.75514604977249178, 9.825000002731188786, 28.56700777964553950 ) ) ;
#7285 = FACE_OUTER_BOUND ( 'NONE', #32956, .T. ) ;
#7286 = CARTESIAN_POINT ( 'NONE',  ( 20.53372385742108008, 50.09336833240935505, 20.47846945139866648 ) ) ;
#7287 = CARTESIAN_POINT ( 'NONE',  ( 12.13525491562421088, 76.80000000000001137, 8.816778784387095058 ) ) ;
#7288 = CARTESIAN_POINT ( 'NONE',  ( 2.375766604868044141, 81.44874571845313938, -14.99999999999999822 ) ) ;
#7289 = CYLINDRICAL_SURFACE ( 'NONE', #27068, 26.50000000000000000 ) ;
#7290 = CARTESIAN_POINT ( 'NONE',  ( 20.08610463437157279, 61.80000000546237970, -27.64615127144129758 ) ) ;
#7291 = CARTESIAN_POINT ( 'NONE',  ( 24.50000000000000355, 15.64999999453761426, 7.960532557706212486 ) ) ;
#7292 = CARTESIAN_POINT ( 'NONE',  ( 12.13525491562421088, 77.05000000546239391, 8.816778784387095058 ) ) ;
#7293 = CARTESIAN_POINT ( 'NONE',  ( -13.97622843553588901, 21.30989583333331794, 24.20753774853756823 ) ) ;
#7294 = CARTESIAN_POINT ( 'NONE',  ( 20.75514604977248467, 32.42500000273116711, -28.56700777964554305 ) ) ;
#7295 = CARTESIAN_POINT ( 'NONE',  ( -10.37757302488624411, 78.72500000273117848, -31.93888565452638417 ) ) ;
#7296 = CARTESIAN_POINT ( 'NONE',  ( -10.37757302488624411, 44.97500000273117848, -31.93888565452638417 ) ) ;
#7297 = CARTESIAN_POINT ( 'NONE',  ( -33.58253175000000113, 21.47500000273120335, 10.91162601494193929 ) ) ;
#7298 = CARTESIAN_POINT ( 'NONE',  ( -20.08610463437156923, 68.29999999999998295, 27.64615127144130113 ) ) ;
#7299 = AXIS2_PLACEMENT_3D ( 'NONE', #5090, #22771, #2166 ) ;
#7300 = CARTESIAN_POINT ( 'NONE',  ( 10.37757302488624056, 76.52500000273118985, -31.93888565452638417 ) ) ;
#7301 = CARTESIAN_POINT ( 'NONE',  ( -5.147494310547430452, 65.55125428154684641, -32.49999999999999289 ) ) ;
#7302 = CARTESIAN_POINT ( 'NONE',  ( -2.092463501923844636E-15, 63.50000000000000000, -34.17252228774368916 ) ) ;
#7303 = CARTESIAN_POINT ( 'NONE',  ( 23.41746824999999887, 14.62499999726882294, 0.000000000000000000 ) ) ;
#7304 = CARTESIAN_POINT ( 'NONE',  ( -27.16883889988623935, 67.32500000273117280, 19.73931689729374739 ) ) ;
#7305 = CARTESIAN_POINT ( 'NONE',  ( 7.236395654485760609, 3.524999997268824181, -22.27133577429736633 ) ) ;
#7306 = CARTESIAN_POINT ( 'NONE',  ( 13.94119854578893580, 45.65326416574269786, -24.22776226481265383 ) ) ;
#7307 = CARTESIAN_POINT ( 'NONE',  ( 6.486482029760649416E-15, 77.87500000273118417, 35.31076352940723240 ) ) ;
#7308 = CARTESIAN_POINT ( 'NONE',  ( 20.75514604977249178, 3.825000002731174575, 28.56700777964553950 ) ) ;
#7309 = CARTESIAN_POINT ( 'NONE',  ( -23.41746824999999887, 10.12499999726881938, -2.867812753649727150E-15 ) ) ;
#7310 = CARTESIAN_POINT ( 'NONE',  ( -24.20753774853756823, 63.41927083333333570, -13.97622843553588723 ) ) ;
#7311 = ORIENTED_EDGE ( 'NONE', *, *, #9439, .F. ) ;
#7312 = CARTESIAN_POINT ( 'NONE',  ( 20.75514604977248467, 52.42500000273118133, -28.56700777964554305 ) ) ;
#7313 = ADVANCED_FACE ( 'NONE', ( #20595 ), #22849, .T. ) ;
#7314 = ORIENTED_EDGE ( 'NONE', *, *, #17702, .T. ) ;
#7315 = CARTESIAN_POINT ( 'NONE',  ( -2.584737979205441561E-13, 36.49218750000000000, -30.02300923189239512 ) ) ;
#7316 = CARTESIAN_POINT ( 'NONE',  ( 20.53372385742072481, 34.92225666759063074, -20.47846945139902175 ) ) ;
#7317 = CARTESIAN_POINT ( 'NONE',  ( 7.570916362186213000, 10.39999999999999325, -23.30088464923126423 ) ) ;
#7318 = CARTESIAN_POINT ( 'NONE',  ( -10.04305231718579172, 8.100000005462391073, -30.90933677959248982 ) ) ;
#7319 = DIRECTION ( 'NONE',  ( 0.000000000000000000, 0.000000000000000000, -1.000000000000000000 ) ) ;
#7320 = CARTESIAN_POINT ( 'NONE',  ( 14.47279130897151589, 2.824999997268819119, 19.92008829642072953 ) ) ;
#7321 = CIRCLE ( 'NONE', #29774, 27.00000000000000000 ) ;
#7322 = CARTESIAN_POINT ( 'NONE',  ( 7.236395654485760609, 11.02499999726880375, -22.27133577429736633 ) ) ;
#7323 = CARTESIAN_POINT ( 'NONE',  ( 20.75514604977248467, 14.67500000273117955, -28.56700777964554305 ) ) ;
#7324 = CARTESIAN_POINT ( 'NONE',  ( -26.29305231718578995, 26.70000000546238184, 19.10302069950538595 ) ) ;
#7325 = CARTESIAN_POINT ( 'NONE',  ( 20.08610463437158344, 68.70000000000001705, 27.64615127144129403 ) ) ;
#7326 = CARTESIAN_POINT ( 'NONE',  ( -24.50000000000000000, 4.899999999999990585, -7.960532557706207157 ) ) ;
#7327 = CARTESIAN_POINT ( 'NONE',  ( -14.92155348893272837, 73.99999999999998579, 1.191227978897531958 ) ) ;
#7328 = CARTESIAN_POINT ( 'NONE',  ( -2.584737979205441561E-13, 15.86718749999999645, -30.02300923189239512 ) ) ;
#7329 = CARTESIAN_POINT ( 'NONE',  ( 27.16883889988623935, 32.57500000273119412, -19.73931689729374384 ) ) ;
#7330 = CARTESIAN_POINT ( 'NONE',  ( 2.688165632520823219E-15, 79.87500000273118417, 14.63369212191046387 ) ) ;
#7331 = CARTESIAN_POINT ( 'NONE',  ( -30.02300923189239867, 42.50781249999998579, 2.654126918244514854E-13 ) ) ;
#7332 = PRESENTATION_STYLE_ASSIGNMENT (( #22957 ) ) ;
#7333 = CARTESIAN_POINT ( 'NONE',  ( -14.47279130897151589, 15.82499999726881335, -19.92008829642072598 ) ) ;
#7334 = CARTESIAN_POINT ( 'NONE',  ( -10.04305231718579172, 9.599999999999997868, -30.90933677959248982 ) ) ;
#7335 = CARTESIAN_POINT ( 'NONE',  ( -4.732186688966233175E-15, 17.50000000000000000, 25.76082449383753925 ) ) ;
#7336 = CARTESIAN_POINT ( 'NONE',  ( -24.18731323226221974, 54.53347249907601935, 14.01125832528330406 ) ) ;
#7337 = CARTESIAN_POINT ( 'NONE',  ( 6.486482029760649416E-15, 47.62500000273118417, 35.31076352940723240 ) ) ;
#7338 = CARTESIAN_POINT ( 'NONE',  ( 27.16883889988624290, 62.17500000273119554, 19.73931689729373673 ) ) ;
#7339 = CARTESIAN_POINT ( 'NONE',  ( -27.16883889988624290, 41.17500000273119554, -19.73931689729374028 ) ) ;
#7340 = CARTESIAN_POINT ( 'NONE',  ( 15.07600611976209848, 16.91151231482331596, -19.08983433668813134 ) ) ;
#7341 = CYLINDRICAL_SURFACE ( 'NONE', #31457, 15.00000000000000000 ) ;
#7342 = CARTESIAN_POINT ( 'NONE',  ( -32.50000000000000000, 49.89999999999999147, -10.55989012756945300 ) ) ;
#7343 = CARTESIAN_POINT ( 'NONE',  ( -14.34159108954266770, 16.99999999999999289, -19.25229178662170071 ) ) ;
#7344 = CARTESIAN_POINT ( 'NONE',  ( 26.29305231718578995, 79.20000000000000284, -19.10302069950538240 ) ) ;
#7345 = CARTESIAN_POINT ( 'NONE',  ( 6.486482029760649416E-15, 19.62500000273116996, 35.31076352940723240 ) ) ;
#7346 = DIRECTION ( 'NONE',  ( 1.000000000000000000, 0.000000000000000000, 0.000000000000000000 ) ) ;
#7347 = CARTESIAN_POINT ( 'NONE',  ( -3.880418787951104953, 13.19874571299077459, 24.50000000000000711 ) ) ;
#7348 = AXIS2_PLACEMENT_3D ( 'NONE', #5830, #16309, #26765 ) ;
#7349 = DIRECTION ( 'NONE',  ( -0.000000000000000000, 1.000000000000000000, -0.000000000000000000 ) ) ;
#7350 = CARTESIAN_POINT ( 'NONE',  ( -28.02196122052058413, 68.71315999907601224, -7.468012846824272799 ) ) ;
#7351 = CARTESIAN_POINT ( 'NONE',  ( 32.50000000000000711, 41.40000000546238823, 10.55989012756945122 ) ) ;
#7352 = CARTESIAN_POINT ( 'NONE',  ( 20.08610463437158344, 34.70000000000000995, 27.64615127144129403 ) ) ;
#7353 = CARTESIAN_POINT ( 'NONE',  ( -33.58253175000000113, 29.12500000273118772, 0.000000000000000000 ) ) ;
#7354 = CARTESIAN_POINT ( 'NONE',  ( 24.20753774853756113, 34.20052083333332860, 13.97622843553589789 ) ) ;
#7355 = VERTEX_POINT ( 'NONE', #27790 ) ;
#7356 = CARTESIAN_POINT ( 'NONE',  ( 33.58253175000000823, 72.02500000273118985, 10.91162601494192863 ) ) ;
#7357 = CARTESIAN_POINT ( 'NONE',  ( -30.02300923189239512, 42.50781249999997868, 2.654126918244515359E-13 ) ) ;
#7358 = EDGE_CURVE ( 'NONE', #12253, #29760, #3665, .T. ) ;
#7359 = FACE_OUTER_BOUND ( 'NONE', #23670, .T. ) ;
#7360 = VERTEX_POINT ( 'NONE', #25211 ) ;
#7361 = CARTESIAN_POINT ( 'NONE',  ( 15.04653450569292872, 62.27902750092396644, -25.98046417659857710 ) ) ;
#7362 = CARTESIAN_POINT ( 'NONE',  ( 13.94119854578937812, 63.42486083425730925, 24.22776226481240514 ) ) ;
#7363 = ORIENTED_EDGE ( 'NONE', *, *, #9567, .F. ) ;
#7364 = CARTESIAN_POINT ( 'NONE',  ( -10.37757302488623701, 9.525000002731195181, 31.93888565452638417 ) ) ;
#7365 =( BOUNDED_CURVE ( )  B_SPLINE_CURVE ( 2, ( #15921, #3372, #23976, #24309, #32017, #5946, #2868, #8513, #27041, #26545, #16258, #16425, #16094, #26877, #21070, #3211, #13161, #18667, #5440, #31519, #3041, #13843, #13513, #29105, #8013, #32187, #26377, #24143, #447, #29277, #10929, #5778, #21404, #18498, #13337, #26715, #23810, #611, #275, #11102, #21571, #21240, #783, #31683, #18999, #19165, #31849, #11265, #21741, #23637, #8177, #8681, #29603, #6104, #32513, #9176, #6447, #27546, #30275, #11755, #22561, #6277, #24470, #21900, #19660, #32846, #17428, #16919, #6609, #32352, #3535, #22069, #14007, #30103, #22236, #30447, #3868, #25138, #8844, #24798, #4033, #945, #22398, #3703, #17086, #4205, #14340, #27379, #11425, #17256, #27717, #14508, #6945, #32681, #14677, #19327, #1614, #11928, #14175, #20000, #1275 ),
 .UNSPECIFIED., .F., .T. ) 
 B_SPLINE_CURVE_WITH_KNOTS ( ( 3, 2, 2, 2, 2, 2, 2, 2, 2, 2, 2, 2, 2, 2, 2, 2, 2, 2, 2, 2, 2, 2, 2, 2, 2, 2, 2, 2, 2, 2, 2, 2, 2, 2, 2, 2, 2, 2, 2, 2, 2, 2, 2, 2, 2, 2, 2, 2, 2, 2, 3 ),
 ( 0.000000000000000000, 0.02000000000000000042, 0.04000000000000000083, 0.05999999999999999778, 0.08000000000000000167, 0.1000000000000000056, 0.1199999999999999956, 0.1400000000000000133, 0.1600000000000000033, 0.1799999999999999933, 0.2000000000000000111, 0.2200000000000000011, 0.2399999999999999911, 0.2600000000000000089, 0.2800000000000000266, 0.2999999999999999889, 0.3200000000000000067, 0.3400000000000000244, 0.3599999999999999867, 0.3800000000000000044, 0.4000000000000000222, 0.4199999999999999845, 0.4400000000000000022, 0.4600000000000000200, 0.4799999999999999822, 0.5000000000000000000, 0.5200000000000000178, 0.5400000000000000355, 0.5600000000000000533, 0.5799999999999999600, 0.5999999999999999778, 0.6199999999999999956, 0.6400000000000000133, 0.6600000000000000311, 0.6800000000000000488, 0.6999999999999999556, 0.7199999999999999734, 0.7399999999999999911, 0.7600000000000000089, 0.7800000000000000266, 0.8000000000000000444, 0.8199999999999999512, 0.8399999999999999689, 0.8599999999999999867, 0.8800000000000000044, 0.9000000000000000222, 0.9200000000000000400, 0.9399999999999999467, 0.9599999999999999645, 0.9799999999999999822, 1.000000000000000000 ),
 .UNSPECIFIED. ) 
 CURVE ( )  GEOMETRIC_REPRESENTATION_ITEM ( )  RATIONAL_B_SPLINE_CURVE ( ( 1.000000000000000000, 0.9510565162951535312, 1.000000000000000000, 0.9510565162951535312, 1.000000000000000000, 0.9510565162951535312, 1.000000000000000000, 0.9510565162951535312, 1.000000000000000000, 0.9510565162951535312, 1.000000000000000000, 0.9510565162951535312, 1.000000000000000000, 0.9510565162951535312, 1.000000000000000000, 0.9510565162951535312, 1.000000000000000000, 0.9510565162951535312, 1.000000000000000000, 0.9510565162951535312, 1.000000000000000000, 0.9510565162951535312, 1.000000000000000000, 0.9510565162951535312, 1.000000000000000000, 0.9510565162951535312, 1.000000000000000000, 0.9510565162951535312, 1.000000000000000000, 0.9510565162951535312, 1.000000000000000000, 0.9510565162951535312, 1.000000000000000000, 0.9510565162951535312, 1.000000000000000000, 0.9510565162951535312, 1.000000000000000000, 0.9510565162951535312, 1.000000000000000000, 0.9510565162951535312, 1.000000000000000000, 0.9510565162951535312, 1.000000000000000000, 0.9510565162951535312, 1.000000000000000000, 0.9510565162951535312, 1.000000000000000000, 0.9510565162951535312, 1.000000000000000000, 0.9510565162951535312, 1.000000000000000000, 0.9510565162951535312, 1.000000000000000000, 0.9510565162951535312, 1.000000000000000000, 0.9510565162951535312, 1.000000000000000000, 0.9510565162951535312, 1.000000000000000000, 0.9510565162951535312, 1.000000000000000000, 0.9510565162951535312, 1.000000000000000000, 0.9510565162951535312, 1.000000000000000000, 0.9510565162951535312, 1.000000000000000000, 0.9510565162951535312, 1.000000000000000000, 0.9510565162951535312, 1.000000000000000000, 0.9510565162951535312, 1.000000000000000000, 0.9510565162951535312, 1.000000000000000000, 0.9510565162951535312, 1.000000000000000000, 0.9510565162951535312, 1.000000000000000000, 0.9510565162951535312, 1.000000000000000000, 0.9510565162951535312, 1.000000000000000000, 0.9510565162951535312, 1.000000000000000000, 0.9510565162951535312, 1.000000000000000000, 0.9510565162951535312, 1.000000000000000000, 0.9510565162951535312, 1.000000000000000000, 0.9510565162951535312, 1.000000000000000000, 0.9510565162951535312, 1.000000000000000000, 0.9510565162951535312, 1.000000000000000000, 0.9510565162951535312, 1.000000000000000000, 0.9510565162951535312, 1.000000000000000000 ) ) 
 REPRESENTATION_ITEM ( '' )  );
#7366 = EDGE_CURVE ( 'NONE', #31472, #15743, #30745, .T. ) ;
#7367 = CARTESIAN_POINT ( 'NONE',  ( -15.04653450569338524, 14.14284749907602290, -25.98046417659831775 ) ) ;
#7368 = CARTESIAN_POINT ( 'NONE',  ( 33.58253175000000113, 36.47500000273119269, -10.91162601494193751 ) ) ;
#7369 =( GEOMETRIC_REPRESENTATION_CONTEXT ( 3 ) GLOBAL_UNCERTAINTY_ASSIGNED_CONTEXT ( ( #8571 ) ) GLOBAL_UNIT_ASSIGNED_CONTEXT ( ( #1661, #22785, #30662 ) ) REPRESENTATION_CONTEXT ( 'NONE', 'WORKASPACE' ) );
#7370 = CARTESIAN_POINT ( 'NONE',  ( 26.29305231718578995, 45.70000000546237118, -19.10302069950538240 ) ) ;
#7371 =( BOUNDED_CURVE ( )  B_SPLINE_CURVE ( 2, ( #19288, #29731, #14139, #16881, #16386, #22199, #6064, #11549, #26839, #16547, #22031, #11890, #6236 ),
 .UNSPECIFIED., .F., .T. ) 
 B_SPLINE_CURVE_WITH_KNOTS ( ( 3, 2, 2, 2, 2, 2, 3 ),
 ( 0.8269230769230769829, 0.8282051282051282604, 0.8307692307692308153, 0.8333333333333333703, 0.8358974358974359253, 0.8384615384615384803, 0.8397435897435897578 ),
 .UNSPECIFIED. ) 
 CURVE ( )  GEOMETRIC_REPRESENTATION_ITEM ( )  RATIONAL_B_SPLINE_CURVE ( ( 0.9755282581475768211, 0.9755282581475778203, 1.000000000000000000, 0.9510565162951535312, 1.000000000000000000, 0.9510565162951535312, 1.000000000000000000, 0.9510565162951535312, 1.000000000000000000, 0.9510565162951535312, 1.000000000000000000, 0.9755282581475768211, 0.9755282581475768211 ) ) 
 REPRESENTATION_ITEM ( '' )  );
#7372 = CARTESIAN_POINT ( 'NONE',  ( -12.13525491562421088, 79.80000000000003979, -8.816778784387096835 ) ) ;
#7373 = CARTESIAN_POINT ( 'NONE',  ( 20.75514604977249178, 23.82500000273118701, 28.56700777964553950 ) ) ;
#7374 = CARTESIAN_POINT ( 'NONE',  ( 24.50000000000000000, 13.84999999453761177, -7.960532557706203605 ) ) ;
#7375 = CARTESIAN_POINT ( 'NONE',  ( 27.16883889988624290, 46.17500000273119554, 19.73931689729373673 ) ) ;
#7376 = SURFACE_SIDE_STYLE ('',( #10130 ) ) ;
#7377 = CARTESIAN_POINT ( 'NONE',  ( -20.08610463437157989, 27.69999999999999929, -27.64615127144129758 ) ) ;
#7378 = CARTESIAN_POINT ( 'NONE',  ( -2.092463501923844636E-15, 29.49999999999999645, -34.17252228774368916 ) ) ;
#7379 = CARTESIAN_POINT ( 'NONE',  ( 1.577395562988744260E-15, 0.5000000000000133227, -25.76082449383753925 ) ) ;
#7380 = CARTESIAN_POINT ( 'NONE',  ( -10.37757302488624411, 72.72500000273119269, -31.93888565452638417 ) ) ;
#7381 = FACE_OUTER_BOUND ( 'NONE', #10798, .T. ) ;
#7382 = CARTESIAN_POINT ( 'NONE',  ( 13.91746824999999532, 74.47500000273122112, -4.522059556121118540 ) ) ;
#7383 = CARTESIAN_POINT ( 'NONE',  ( -20.75514604977248112, 57.67500000273118843, 28.56700777964554661 ) ) ;
#7384 = CARTESIAN_POINT ( 'NONE',  ( 15.00000000000000355, 77.15000000546237402, 4.873795443493592394 ) ) ;
#7385 = CARTESIAN_POINT ( 'NONE',  ( 5.779280353836490358E-15, 7.000000005462371000, 32.49999999999999289 ) ) ;
#7386 = CARTESIAN_POINT ( 'NONE',  ( -10.37757302488623701, 19.52500000273118985, 31.93888565452638417 ) ) ;
#7387 = CARTESIAN_POINT ( 'NONE',  ( -15.14183272437241889, 10.44999999453763095, -20.84094480462497856 ) ) ;
#7388 = CARTESIAN_POINT ( 'NONE',  ( -6.950374756619716266, 20.59934000092397355, -26.09010956794232428 ) ) ;
#7389 = CARTESIAN_POINT ( 'NONE',  ( -33.58253175000000113, 43.12500000273118417, 0.000000000000000000 ) ) ;
#7390 = DIRECTION ( 'NONE',  ( 1.000000000000000000, 0.000000000000000000, -0.000000000000000000 ) ) ;
#7391 = CARTESIAN_POINT ( 'NONE',  ( 33.58253175000000113, 56.47500000273116427, -10.91162601494193574 ) ) ;
#7392 = CARTESIAN_POINT ( 'NONE',  ( 14.97647472619947351, 49.67486083425730925, 26.02091320914850314 ) ) ;
#7393 = CARTESIAN_POINT ( 'NONE',  ( 24.50000000000000000, 15.99999999999998579, 0.000000000000000000 ) ) ;
#7394 = CARTESIAN_POINT ( 'NONE',  ( 15.04653450569339945, 33.04909749907601935, 25.98046417659831775 ) ) ;
#7395 = CARTESIAN_POINT ( 'NONE',  ( -10.04305231718579172, 64.10000000546239107, -30.90933677959248982 ) ) ;
#7396 = CIRCLE ( 'NONE', #16188, 24.50000000000000000 ) ;
#7397 = CARTESIAN_POINT ( 'NONE',  ( 13.91746824999999532, 73.97500000273115006, -4.522059556121118540 ) ) ;
#7398 = CARTESIAN_POINT ( 'NONE',  ( 26.29305231718579350, 57.30000000546238681, 19.10302069950537529 ) ) ;
#7399 = CARTESIAN_POINT ( 'NONE',  ( 24.22776226481265383, 67.13763916574266943, 13.94119854578893580 ) ) ;
#7400 = CARTESIAN_POINT ( 'NONE',  ( -7.236395654485763274, 2.524999997268823293, 22.27133577429736633 ) ) ;
#7401 = CARTESIAN_POINT ( 'NONE',  ( 20.08610463437158344, 73.20000000546235697, 27.64615127144129403 ) ) ;
#7402 = CARTESIAN_POINT ( 'NONE',  ( -8.891200544363830713E-16, 79.49999999999998579, -15.00000000000000000 ) ) ;
#7403 = CARTESIAN_POINT ( 'NONE',  ( -20.75514604977248112, 33.67500000273119554, 28.56700777964554661 ) ) ;
#7404 = CARTESIAN_POINT ( 'NONE',  ( 18.94512977948575738, 8.924999997268812990, 13.76444248337723408 ) ) ;
#7405 = VERTEX_POINT ( 'NONE', #23151 ) ;
#7406 = CARTESIAN_POINT ( 'NONE',  ( -10.37757302488624411, 72.97500000273119269, -31.93888565452638417 ) ) ;
#7407 = CARTESIAN_POINT ( 'NONE',  ( 26.29305231718578995, 23.70000000546239249, -19.10302069950538240 ) ) ;
#7408 = CARTESIAN_POINT ( 'NONE',  ( -20.50609665441004736, 42.93750000000000000, -20.50609665440969565 ) ) ;
#7409 = CARTESIAN_POINT ( 'NONE',  ( -33.58253175000000113, 51.47500000273118559, 10.91162601494193929 ) ) ;
#7410 = CARTESIAN_POINT ( 'NONE',  ( -2.092463501923844636E-15, 66.00000000546239676, -34.17252228774368916 ) ) ;
#7411 = VERTEX_POINT ( 'NONE', #1864 ) ;
#7412 = FACE_OUTER_BOUND ( 'NONE', #13782, .T. ) ;
#7413 = CARTESIAN_POINT ( 'NONE',  ( -33.58253175000000113, 39.02500000273118985, -10.91162601494193218 ) ) ;
#7414 = CARTESIAN_POINT ( 'NONE',  ( -18.94512977948575738, 17.42499999726882010, -13.76444248337723231 ) ) ;
#7415 = CARTESIAN_POINT ( 'NONE',  ( -20.75514604977248112, 69.67500000273119554, 28.56700777964554661 ) ) ;
#7416 = CARTESIAN_POINT ( 'NONE',  ( 26.29305231718579350, 3.300000005462377928, 19.10302069950537529 ) ) ;
#7417 = CARTESIAN_POINT ( 'NONE',  ( 33.58253175000000113, 60.12500000273117706, -4.112674001490185761E-15 ) ) ;
#7418 = DIRECTION ( 'NONE',  ( 0.000000000000000000, 0.000000000000000000, -1.000000000000000000 ) ) ;
#7419 = CARTESIAN_POINT ( 'NONE',  ( 6.277390505771533514E-15, 46.50000000000001421, 34.17252228774368916 ) ) ;
#7420 = CARTESIAN_POINT ( 'NONE',  ( 24.50000000000000000, 1.899999999999998135, 7.960532557706212486 ) ) ;
#7421 = CARTESIAN_POINT ( 'NONE',  ( -10.37757302488624411, 16.97500000273119269, -31.93888565452638417 ) ) ;
#7422 = CARTESIAN_POINT ( 'NONE',  ( 19.82091636218621389, 0.2000000000000057288, -14.40073868116559197 ) ) ;
#7423 = CARTESIAN_POINT ( 'NONE',  ( -24.18731323226221974, 23.59597249907602290, 14.01125832528330406 ) ) ;
#7424 = CARTESIAN_POINT ( 'NONE',  ( -13.91746824999999887, 77.37500000273116996, 0.000000000000000000 ) ) ;
#7425 = CARTESIAN_POINT ( 'NONE',  ( -33.58253175000000113, 77.47500000273120691, 10.91162601494193929 ) ) ;
#7426 = CARTESIAN_POINT ( 'NONE',  ( -32.50000000000000000, 52.00000000000000711, 0.000000000000000000 ) ) ;
#7427 = CARTESIAN_POINT ( 'NONE',  ( 27.16883889988623935, 72.57500000273118701, -19.73931689729374384 ) ) ;
#7428 = VERTEX_POINT ( 'NONE', #4617 ) ;
#7429 = CARTESIAN_POINT ( 'NONE',  ( 1.507698388325705758E-15, 13.62499999726882827, -24.62258325217400312 ) ) ;
#7430 = CARTESIAN_POINT ( 'NONE',  ( 18.94512977948576093, 2.824999997268817786, -13.76444248337722875 ) ) ;
#7431 = CARTESIAN_POINT ( 'NONE',  ( 24.20753774853731244, 47.37760416666666430, -13.97622843553632599 ) ) ;
#7432 = EDGE_CURVE ( 'NONE', #11746, #18278, #8847, .T. ) ;
#7433 = CIRCLE ( 'NONE', #26618, 32.50000000000000000 ) ;
#7434 = CARTESIAN_POINT ( 'NONE',  ( 6.486482029760649416E-15, 57.62500000273119127, 35.31076352940723240 ) ) ;
#7435 = CARTESIAN_POINT ( 'NONE',  ( 20.75514604977249178, 16.07500000273119412, 28.56700777964553950 ) ) ;
#7436 = CARTESIAN_POINT ( 'NONE',  ( -33.58253175000000113, 9.475000002731185589, 10.91162601494193929 ) ) ;
#7437 = CARTESIAN_POINT ( 'NONE',  ( 19.09188309203694800, 27.46875000000000000, 19.09188309203660694 ) ) ;
#7438 = UNCERTAINTY_MEASURE_WITH_UNIT (LENGTH_MEASURE( 1.000000000000000082E-05 ), #12529, 'distance_accuracy_value', 'NONE');
#7439 = VECTOR ( 'NONE', #26733, 1000.000000000000000 ) ;
#7440 = CARTESIAN_POINT ( 'NONE',  ( -14.97647472619946285, 17.01861083425731280, -26.02091320914851025 ) ) ;
#7441 = CARTESIAN_POINT ( 'NONE',  ( 26.00068869287340334, 61.12760416666665719, -15.01150461594642316 ) ) ;
#7442 = CARTESIAN_POINT ( 'NONE',  ( -27.16883889988624290, 4.925000002731189319, -19.73931689729374028 ) ) ;
#7443 = CARTESIAN_POINT ( 'NONE',  ( 13.91746824999999532, 72.47500000273119269, -4.522059556121118540 ) ) ;
#7444 = CARTESIAN_POINT ( 'NONE',  ( 32.50000000000000711, 42.90000000000001279, 10.55989012756945122 ) ) ;
#7445 = CARTESIAN_POINT ( 'NONE',  ( 10.37757302488624767, 47.72500000273119269, 31.93888565452638417 ) ) ;
#7446 = CARTESIAN_POINT ( 'NONE',  ( -14.47279130897151589, 7.324999997268822227, -19.92008829642072598 ) ) ;
#7447 = CARTESIAN_POINT ( 'NONE',  ( 7.570916362186207671, 13.60000000000000142, 23.30088464923126779 ) ) ;
#7448 = ORIENTED_EDGE ( 'NONE', *, *, #9354, .F. ) ;
#7449 = CARTESIAN_POINT ( 'NONE',  ( 33.58253175000000113, 54.37500000273119838, -4.112674001490185761E-15 ) ) ;
#7450 = CARTESIAN_POINT ( 'NONE',  ( 5.147494310547481966, 59.94874572391553613, -32.49999999999998579 ) ) ;
#7451 = CARTESIAN_POINT ( 'NONE',  ( -26.09010956794232428, 40.36496500092396644, 6.950374756619732253 ) ) ;
#7452 = CARTESIAN_POINT ( 'NONE',  ( 33.58253175000000113, 78.47500000273116427, -10.91162601494193751 ) ) ;
#7453 = ORIENTED_EDGE ( 'NONE', *, *, #14536, .F. ) ;
#7454 = APPLICATION_CONTEXT ( 'automotive_design' ) ;
#7455 = CARTESIAN_POINT ( 'NONE',  ( -20.75514604977248112, 23.42500000273119909, 28.56700777964554661 ) ) ;
#7456 = CARTESIAN_POINT ( 'NONE',  ( 28.01184896238290278, 20.02083333333332860, -7.505752307973347470 ) ) ;
#7457 = VERTEX_POINT ( 'NONE', #2856 ) ;
#7458 = AXIS2_PLACEMENT_3D ( 'NONE', #706, #11192, #20998 ) ;
#7459 = CARTESIAN_POINT ( 'NONE',  ( 4.445600272181915325E-13, 14.00000000546237544, -32.50000000000000000 ) ) ;
#7460 = CARTESIAN_POINT ( 'NONE',  ( 6.486482029760649416E-15, 59.62500000273118417, 35.31076352940723240 ) ) ;
#7461 = CARTESIAN_POINT ( 'NONE',  ( -26.00068869287368756, 39.35677083333331439, -15.01150461594595775 ) ) ;
#7462 = ADVANCED_FACE ( 'NONE', ( #22811 ), #20355, .T. ) ;
#7463 = CARTESIAN_POINT ( 'NONE',  ( 7.570916362186207671, 11.59999999999999964, 23.30088464923126779 ) ) ;
#7464 = CARTESIAN_POINT ( 'NONE',  ( 1.507698388325705758E-15, 3.624999997268822938, -24.62258325217400312 ) ) ;
#7465 = CARTESIAN_POINT ( 'NONE',  ( -33.58253175000000113, 11.02500000273117919, -10.91162601494193218 ) ) ;
#7466 = CARTESIAN_POINT ( 'NONE',  ( 5.147494310547434893, 28.55125428154685352, 32.49999999999999289 ) ) ;
#7467 = CARTESIAN_POINT ( 'NONE',  ( -7.543491769121917656, 55.53607666574269075, -28.00173670424536354 ) ) ;
#7468 = CARTESIAN_POINT ( 'NONE',  ( 10.04305231718578817, 37.39999999999999147, -30.90933677959249337 ) ) ;
#7469 = DIRECTION ( 'NONE',  ( 0.000000000000000000, 0.000000000000000000, -1.000000000000000000 ) ) ;
#7470 = CARTESIAN_POINT ( 'NONE',  ( 26.29305231718578995, 19.70000000546237473, -19.10302069950538240 ) ) ;
#7471 = ADVANCED_FACE ( 'NONE', ( #10752 ), #33270, .T. ) ;
#7472 = CARTESIAN_POINT ( 'NONE',  ( 10.04305231718579705, 16.59999999999999076, 30.90933677959248982 ) ) ;
#7473 = CARTESIAN_POINT ( 'NONE',  ( -4.732186688966233175E-15, 11.24999999453763699, 25.76082449383753925 ) ) ;
#7474 = CARTESIAN_POINT ( 'NONE',  ( 15.00000000000000000, 71.35000000546237686, -4.873795443493596835 ) ) ;
#7475 = CARTESIAN_POINT ( 'NONE',  ( -13.97622843553632421, 22.45572916666666430, -24.20753774853731599 ) ) ;
#7476 =( BOUNDED_CURVE ( )  B_SPLINE_CURVE ( 2, ( #11108, #14180, #29449, #24149, #8687, #11595, #16591, #8348, #24315, #24636, #27048, #29949, #3541 ),
 .UNSPECIFIED., .F., .F. ) 
 B_SPLINE_CURVE_WITH_KNOTS ( ( 3, 2, 2, 2, 2, 2, 3 ),
 ( 0.5064102564102563875, 0.5076923076923076650, 0.5102564102564102200, 0.5128205128205127750, 0.5153846153846153300, 0.5179487179487179960, 0.5192307692307692735 ),
 .UNSPECIFIED. ) 
 CURVE ( )  GEOMETRIC_REPRESENTATION_ITEM ( )  RATIONAL_B_SPLINE_CURVE ( ( 0.9755282581475768211, 0.9755282581475768211, 1.000000000000000000, 0.9510565162951535312, 1.000000000000000000, 0.9510565162951535312, 1.000000000000000000, 0.9510565162951535312, 1.000000000000000000, 0.9510565162951535312, 1.000000000000000000, 0.9755282581475768211, 0.9755282581475768211 ) ) 
 REPRESENTATION_ITEM ( '' )  );
#7477 = CARTESIAN_POINT ( 'NONE',  ( 33.58253175000000113, 34.12500000273119127, -4.112674001490185761E-15 ) ) ;
#7478 = FACE_OUTER_BOUND ( 'NONE', #23074, .T. ) ;
#7479 = CARTESIAN_POINT ( 'NONE',  ( -33.58253175000000113, 41.27500000273117564, -10.91162601494193218 ) ) ;
#7480 = CARTESIAN_POINT ( 'NONE',  ( -33.58253175000000113, 19.47500000273117493, 10.91162601494193929 ) ) ;
#7481 = CARTESIAN_POINT ( 'NONE',  ( -12.13525491562421088, 79.80000000000001137, -8.816778784387096835 ) ) ;
#7482 = EDGE_CURVE ( 'NONE', #31792, #24787, #18488, .T. ) ;
#7483 = CARTESIAN_POINT ( 'NONE',  ( 27.16883889988623935, 76.32500000273118701, -19.73931689729374384 ) ) ;
#7484 = CARTESIAN_POINT ( 'NONE',  ( 20.08610463437157279, 59.80000000546235839, -27.64615127144129758 ) ) ;
#7485 = CARTESIAN_POINT ( 'NONE',  ( -32.50000000000000000, 62.09999999999999432, 10.55989012756946366 ) ) ;
#7486 = CARTESIAN_POINT ( 'NONE',  ( -7.236395654485763274, 16.02499999726880731, 22.27133577429736633 ) ) ;
#7487 = CARTESIAN_POINT ( 'NONE',  ( -20.75514604977248112, 67.42500000273118133, 28.56700777964554661 ) ) ;
#7488 = CARTESIAN_POINT ( 'NONE',  ( 14.47279130897151767, 11.42499999726880944, -19.92008829642072598 ) ) ;
#7489 = CARTESIAN_POINT ( 'NONE',  ( 33.58253175000000113, 72.47500000273119269, -10.91162601494193751 ) ) ;
#7490 = CARTESIAN_POINT ( 'NONE',  ( -33.58253175000000113, 5.225000002731188253, 10.91162601494193929 ) ) ;
#7491 = CARTESIAN_POINT ( 'NONE',  ( 23.41746825000000243, 2.524999997268798868, 7.608796670333735079 ) ) ;
#7492 = CARTESIAN_POINT ( 'NONE',  ( 19.11951029504763611, 17.73475666759064140, -19.06425588902591173 ) ) ;
#7493 = ORIENTED_EDGE ( 'NONE', *, *, #15171, .T. ) ;
#7494 = CARTESIAN_POINT ( 'NONE',  ( 20.75514604977248467, 42.42500000273117422, -28.56700777964554305 ) ) ;
#7495 = VERTEX_POINT ( 'NONE', #25561 ) ;
#7496 = CARTESIAN_POINT ( 'NONE',  ( -26.00068869287368756, 32.48177083333332860, -15.01150461594595775 ) ) ;
#7497 = CARTESIAN_POINT ( 'NONE',  ( -5.147494310547427787, 79.55125428154684641, -32.49999999999999289 ) ) ;
#7498 = CARTESIAN_POINT ( 'NONE',  ( -32.50000000000000000, 4.400000005462378461, -10.55989012756945478 ) ) ;
#7499 = CARTESIAN_POINT ( 'NONE',  ( 7.236395654485755280, 2.724999997268801266, 22.27133577429736988 ) ) ;
#7500 = CARTESIAN_POINT ( 'NONE',  ( 14.47279130897151767, 12.92499999726881832, -19.92008829642072598 ) ) ;
#7501 = CARTESIAN_POINT ( 'NONE',  ( -10.37757302488624411, 12.97500000273119092, -31.93888565452638417 ) ) ;
#7502 = CARTESIAN_POINT ( 'NONE',  ( -2.092463501923844636E-15, 20.00000000546236834, -34.17252228774368916 ) ) ;
#7503 = CARTESIAN_POINT ( 'NONE',  ( 20.08610463437158344, 66.69999999999997442, 27.64615127144129403 ) ) ;
#7504 = CARTESIAN_POINT ( 'NONE',  ( 4.635254915624212657, 76.85000000546237686, 14.26584774442730286 ) ) ;
#7505 = CARTESIAN_POINT ( 'NONE',  ( -8.891200544363830713E-16, 77.75000000546235412, -15.00000000000000000 ) ) ;
#7506 = CARTESIAN_POINT ( 'NONE',  ( 30.02300923189239512, 13.28906249999999289, -2.619432448724977703E-13 ) ) ;
#7507 = CARTESIAN_POINT ( 'NONE',  ( -20.75514604977248823, 31.07500000273118701, -28.56700777964554305 ) ) ;
#7508 = CARTESIAN_POINT ( 'NONE',  ( 5.147494310547434893, 43.05125428700922185, 32.49999999999999289 ) ) ;
#7509 = CARTESIAN_POINT ( 'NONE',  ( -28.01184896238290278, 35.48958333333332860, 7.505752307973363457 ) ) ;
#7510 = AXIS2_PLACEMENT_3D ( 'NONE', #23474, #21076, #31689 ) ;
#7511 = CARTESIAN_POINT ( 'NONE',  ( -4.523095164977116484E-15, 16.62499999726881583, 24.62258325217400312 ) ) ;
#7512 = CARTESIAN_POINT ( 'NONE',  ( 6.277390505771533514E-15, 6.499999999999998224, 34.17252228774368916 ) ) ;
#7513 = DIRECTION ( 'NONE',  ( 0.000000000000000000, 0.000000000000000000, -1.000000000000000000 ) ) ;
#7514 = CARTESIAN_POINT ( 'NONE',  ( -13.94119854578892514, 54.24701416574269075, 24.22776226481266448 ) ) ;
#7515 = CARTESIAN_POINT ( 'NONE',  ( 27.16883889988624290, 49.92500000273120264, 19.73931689729373673 ) ) ;
#7516 = CARTESIAN_POINT ( 'NONE',  ( -20.75514604977248823, 65.07500000273118701, -28.56700777964554305 ) ) ;
#7517 = CARTESIAN_POINT ( 'NONE',  ( 10.37757302488624767, 39.97500000273118559, 31.93888565452638417 ) ) ;
#7518 = CARTESIAN_POINT ( 'NONE',  ( 10.04305231718578817, 45.39999999999999858, -30.90933677959249337 ) ) ;
#7519 = AXIS2_PLACEMENT_3D ( 'NONE', #3773, #19565, #27281 ) ;
#7520 = CARTESIAN_POINT ( 'NONE',  ( -26.07999730980490583, 15.15104166666666252, -6.988114217767815717 ) ) ;
#7521 = CARTESIAN_POINT ( 'NONE',  ( -24.50000000000000711, 9.100000000000003197, 7.960532557706201828 ) ) ;
#7522 = CARTESIAN_POINT ( 'NONE',  ( -5.147494310547430452, 22.05125428700922185, -32.49999999999999289 ) ) ;
#7523 = CARTESIAN_POINT ( 'NONE',  ( 20.08610463437158344, 76.70000000000000284, 27.64615127144129403 ) ) ;
#7524 = CARTESIAN_POINT ( 'NONE',  ( -33.58253175000000113, 13.22500000273119802, 10.91162601494193929 ) ) ;
#7525 = CARTESIAN_POINT ( 'NONE',  ( 0.000000000000000000, 0.000000000000000000, 0.000000000000000000 ) ) ;
#7526 = DIRECTION ( 'NONE',  ( 0.000000000000000000, -1.000000000000000000, 0.000000000000000000 ) ) ;
#7527 = CYLINDRICAL_SURFACE ( 'NONE', #17053, 32.50000000000000000 ) ;
#7528 = CARTESIAN_POINT ( 'NONE',  ( -24.22776226481266448, 20.73138916574268720, -13.94119854578892514 ) ) ;
#7529 = CARTESIAN_POINT ( 'NONE',  ( 32.50000000000000000, 33.60000000546237686, -10.55989012756945833 ) ) ;
#7530 = CARTESIAN_POINT ( 'NONE',  ( -10.04305231718578462, 66.40000000000000568, 30.90933677959249337 ) ) ;
#7531 = CARTESIAN_POINT ( 'NONE',  ( -33.58253175000000113, 25.12500000273118417, 0.000000000000000000 ) ) ;
#7532 = CARTESIAN_POINT ( 'NONE',  ( 27.95245687107222921, 47.66406249999998579, -2.463307335887066074E-13 ) ) ;
#7533 = EDGE_LOOP ( 'NONE', ( #12921, #21559, #5131, #12948 ) ) ;
#7534 = CARTESIAN_POINT ( 'NONE',  ( 27.16883889988623935, 68.32500000273118701, -19.73931689729374384 ) ) ;
#7535 = CARTESIAN_POINT ( 'NONE',  ( -28.01184896238304134, 46.08854166666666430, -7.505752307972844761 ) ) ;
#7536 = VERTEX_POINT ( 'NONE', #7017 ) ;
#7537 = CARTESIAN_POINT ( 'NONE',  ( 20.47846945139902530, 56.40663166759065206, 20.53372385742071771 ) ) ;
#7538 = CARTESIAN_POINT ( 'NONE',  ( 24.18731323226247554, 56.26340250092398065, 14.01125832528285997 ) ) ;
#7539 = CARTESIAN_POINT ( 'NONE',  ( 20.75514604977248467, 12.42500000273117777, -28.56700777964554305 ) ) ;
#7540 = CARTESIAN_POINT ( 'NONE',  ( -28.00173670424535644, 16.86420166574268720, 7.543491769121936308 ) ) ;
#7541 = DIRECTION ( 'NONE',  ( 0.000000000000000000, -0.000000000000000000, -1.000000000000000000 ) ) ;
#7542 = CARTESIAN_POINT ( 'NONE',  ( 20.75514604977248467, 34.67500000273118843, -28.56700777964554305 ) ) ;
#7543 = CARTESIAN_POINT ( 'NONE',  ( -32.50000000000000000, 34.40000000546236691, -10.55989012756945478 ) ) ;
#7544 = CARTESIAN_POINT ( 'NONE',  ( 12.13525491562421088, 76.80000000000003979, 8.816778784387095058 ) ) ;
#7545 = CARTESIAN_POINT ( 'NONE',  ( -26.00068869287340334, 66.28385416666662877, 15.01150461594643382 ) ) ;
#7546 = CARTESIAN_POINT ( 'NONE',  ( 33.58253175000000113, 22.12500000273118062, -4.112674001490185761E-15 ) ) ;
#7547 = CARTESIAN_POINT ( 'NONE',  ( -2.375766604868044141, 81.55125428154683220, -14.99999999999999822 ) ) ;
#7548 = CARTESIAN_POINT ( 'NONE',  ( -33.58253175000000113, 47.37500000273120548, 0.000000000000000000 ) ) ;
#7549 = APPLICATION_PROTOCOL_DEFINITION ( 'draft international standard', 'automotive_design', 1998, #31353 ) ;
#7550 = CARTESIAN_POINT ( 'NONE',  ( -10.04305231718578462, 30.39999999999999503, 30.90933677959249337 ) ) ;
#7551 = CARTESIAN_POINT ( 'NONE',  ( 32.50000000000000711, 28.89999999999998792, 10.55989012756945122 ) ) ;
#7552 = CARTESIAN_POINT ( 'NONE',  ( -7.570916362186210335, 0.5999999999999894307, -23.30088464923126779 ) ) ;
#7553 = CARTESIAN_POINT ( 'NONE',  ( -20.75514604977248112, 71.42500000273119554, 28.56700777964554661 ) ) ;
#7554 = DIRECTION ( 'NONE',  ( -0.000000000000000000, -1.000000000000000000, -0.000000000000000000 ) ) ;
#7555 = CARTESIAN_POINT ( 'NONE',  ( 4.023268246324634798E-14, 10.24999999453763166, -24.50000000000000355 ) ) ;
#7556 = CARTESIAN_POINT ( 'NONE',  ( -10.37757302488624411, 62.97500000273120691, -31.93888565452638417 ) ) ;
#7557 = CARTESIAN_POINT ( 'NONE',  ( -26.29305231718579350, 40.30000000546237970, -19.10302069950537884 ) ) ;
#7558 = CARTESIAN_POINT ( 'NONE',  ( 33.58253175000000113, 14.12500000273120193, -4.112674001490185761E-15 ) ) ;
#7559 = CARTESIAN_POINT ( 'NONE',  ( -14.01125832528285109, 33.06027750092398776, 24.18731323226248264 ) ) ;
#7560 = ADVANCED_FACE ( 'NONE', ( #7359 ), #8003, .T. ) ;
#7561 = CARTESIAN_POINT ( 'NONE',  ( 27.48632242023158767, 66.99999999999998579, -17.98641839608171011 ) ) ;
#7562 = CARTESIAN_POINT ( 'NONE',  ( -33.58253175000000113, 37.22500000273119980, 10.91162601494193929 ) ) ;
#7563 = DIRECTION ( 'NONE',  ( 0.4999999999999998890, -0.000000000000000000, 0.8660254037844387076 ) ) ;
#7564 = CARTESIAN_POINT ( 'NONE',  ( 26.29305231718579350, 18.79999999999998295, 19.10302069950537529 ) ) ;
#7565 = EDGE_CURVE ( 'NONE', #33921, #28463, #1137, .T. ) ;
#7566 = CARTESIAN_POINT ( 'NONE',  ( 7.570916362186213000, 6.399999999999988809, -23.30088464923126423 ) ) ;
#7567 = CARTESIAN_POINT ( 'NONE',  ( 20.53372385742108008, 46.65586833240934794, 20.47846945139866648 ) ) ;
#7568 = CARTESIAN_POINT ( 'NONE',  ( 20.08610463437157279, 63.80000000546237970, -27.64615127144129758 ) ) ;
#7569 = CARTESIAN_POINT ( 'NONE',  ( 8.601468415847520532, 74.07500000273121543, 11.83890561707634781 ) ) ;
#7570 = FILL_AREA_STYLE ('',( #2934 ) ) ;
#7571 = CARTESIAN_POINT ( 'NONE',  ( -13.94119854578892514, 64.55951416574268364, 24.22776226481266448 ) ) ;
#7572 =( BOUNDED_CURVE ( )  B_SPLINE_CURVE ( 2, ( #33616, #14749, #15911, #14920, #20075, #28130, #12516, #22983, #25387, #17499, #20415, #17668, #4786 ),
 .UNSPECIFIED., .F., .T. ) 
 B_SPLINE_CURVE_WITH_KNOTS ( ( 3, 2, 2, 2, 2, 2, 3 ),
 ( 0.7884615384615384359, 0.7897435897435897134, 0.7923076923076922684, 0.7948717948717948234, 0.7974358974358974894, 0.8000000000000000444, 0.8012820512820513219 ),
 .UNSPECIFIED. ) 
 CURVE ( )  GEOMETRIC_REPRESENTATION_ITEM ( )  RATIONAL_B_SPLINE_CURVE ( ( 0.9755282581475768211, 0.9755282581475768211, 1.000000000000000000, 0.9510565162951535312, 1.000000000000000000, 0.9510565162951535312, 1.000000000000000000, 0.9510565162951535312, 1.000000000000000000, 0.9510565162951535312, 1.000000000000000000, 0.9755282581475768211, 0.9755282581475768211 ) ) 
 REPRESENTATION_ITEM ( '' )  );
#7573 = DIRECTION ( 'NONE',  ( 0.000000000000000000, 0.000000000000000000, -1.000000000000000000 ) ) ;
#7574 = CARTESIAN_POINT ( 'NONE',  ( -26.29305231718578995, 76.70000000546239960, 19.10302069950538595 ) ) ;
#7575 = CARTESIAN_POINT ( 'NONE',  ( -20.50609665441004736, 22.31250000000000000, -20.50609665440969565 ) ) ;
#7576 = CARTESIAN_POINT ( 'NONE',  ( -2.162160676586881955E-15, 36.87500000273116996, -35.31076352940723240 ) ) ;
#7577 =( BOUNDED_CURVE ( )  B_SPLINE_CURVE ( 2, ( #10755, #21233, #16418, #31676, #16085, #13835, #776, #11258, #21734, #32179, #8674, #26200, #25035, #25206, #1683, #33086, #5083, #29378, #19257, #6036, #21668, #11031, #16683, #16515, #11358, #5877, #21500, #32614, #8441, #29875, #24730, #13770, #16355, #9111, #3634, #24402, #6375, #6203, #29698, #32114, #16853, #30040, #21836, #11686, #26967, #18932, #3468, #29533, #13938, #878, #24895, #31948, #27140, #32281, #8774, #26810, #3305, #19592, #24240, #27310, #1205, #19425, #14108, #19095, #17018, #24565, #3801, #1038, #11518, #21998, #32446, #22170, #711, #8947, #11197, #8612, #14273, #6545, #27478, #14440, #3967, #17190, #33471, #7217, #27648, #30722, #14951, #20104, #33299, #33120, #17528, #15295, #28328, #30206, #4816, #1548, #27820, #14611, #25067, #12371, #1895, #9623, #9971, #27989, #9799, #4303, #1381, #7391, #7046, #4476, #20447, #12197, #25417, #4646, #22839, #4136, #17876, #14778, #30897, #12024, #15126, #30550, #25243, #20275, #22493, #17700, #11855, #28160, #25589, #22334, #2069, #12545, #32944, #23016, #9273, #9445, #32779, #19757, #6708, #19929, #30375, #6876, #17356, #1718, #22668, #25755, #10822, #31409, #13399, #2928, #23869, #29000, #162 ),
 .UNSPECIFIED., .F., .T. ) 
 B_SPLINE_CURVE_WITH_KNOTS ( ( 3, 2, 2, 2, 2, 2, 2, 2, 2, 2, 2, 2, 2, 2, 2, 2, 2, 2, 2, 2, 2, 2, 2, 2, 2, 2, 2, 2, 2, 2, 2, 2, 2, 2, 2, 2, 2, 2, 2, 2, 2, 2, 2, 2, 2, 2, 2, 2, 2, 2, 2, 2, 2, 2, 2, 2, 2, 2, 2, 2, 2, 2, 2, 2, 2, 2, 2, 2, 2, 2, 2, 2, 2, 2, 2, 2, 3 ),
 ( 0.1586432617944051326, 0.1589743589743589647, 0.1615384615384615474, 0.1641025641025641024, 0.1666666666666666574, 0.1692307692307692402, 0.1717948717948717952, 0.1743589743589743501, 0.1769230769230769329, 0.1794871794871794879, 0.1820512820512820429, 0.1846153846153846256, 0.1871794871794871806, 0.1897435897435897356, 0.1923076923076923184, 0.1948717948717948734, 0.1974358974358974284, 0.2000000000000000111, 0.2025641025641025661, 0.2051282051282051211, 0.2076923076923077038, 0.2102564102564102588, 0.2128205128205128138, 0.2153846153846153966, 0.2179487179487179516, 0.2205128205128205066, 0.2230769230769230893, 0.2256410256410256443, 0.2282051282051281993, 0.2307692307692307820, 0.2333333333333333370, 0.2358974358974358920, 0.2384615384615384748, 0.2410256410256410298, 0.2435897435897435848, 0.2461538461538461675, 0.2487179487179487225, 0.2512820512820512775, 0.2538461538461538325, 0.2564102564102563875, 0.2589743589743589980, 0.2615384615384615530, 0.2641025641025641080, 0.2666666666666666630, 0.2692307692307692180, 0.2717948717948717730, 0.2743589743589743835, 0.2769230769230769384, 0.2794871794871794934, 0.2820512820512820484, 0.2846153846153846034, 0.2871794871794871584, 0.2897435897435897689, 0.2923076923076923239, 0.2948717948717948789, 0.2974358974358974339, 0.2999999999999999889, 0.3025641025641025439, 0.3051282051282051544, 0.3076923076923077094, 0.3102564102564102644, 0.3128205128205128194, 0.3153846153846153744, 0.3179487179487179294, 0.3205128205128205399, 0.3230769230769230949, 0.3256410256410257054, 0.3282051282051282048, 0.3307692307692307598, 0.3333333333333333148, 0.3358974358974358698, 0.3384615384615384803, 0.3410256410256410353, 0.3435897435897435903, 0.3461538461538461453, 0.3487179487179487003, 0.3509509541020974233 ),
 .UNSPECIFIED. ) 
 CURVE ( )  GEOMETRIC_REPRESENTATION_ITEM ( )  RATIONAL_B_SPLINE_CURVE ( ( 0.9889922301674716199, 0.9936800307216014927, 1.000000000000000000, 0.9510565162951535312, 1.000000000000000000, 0.9510565162951535312, 1.000000000000000000, 0.9510565162951535312, 1.000000000000000000, 0.9510565162951535312, 1.000000000000000000, 0.9510565162951535312, 1.000000000000000000, 0.9510565162951535312, 1.000000000000000000, 0.9510565162951535312, 1.000000000000000000, 0.9510565162951535312, 1.000000000000000000, 0.9510565162951535312, 1.000000000000000000, 0.9510565162951535312, 1.000000000000000000, 0.9510565162951535312, 1.000000000000000000, 0.9510565162951535312, 1.000000000000000000, 0.9510565162951535312, 1.000000000000000000, 0.9510565162951535312, 1.000000000000000000, 0.9510565162951535312, 1.000000000000000000, 0.9510565162951535312, 1.000000000000000000, 0.9510565162951535312, 1.000000000000000000, 0.9510565162951535312, 1.000000000000000000, 0.9510565162951535312, 1.000000000000000000, 0.9510565162951535312, 1.000000000000000000, 0.9510565162951535312, 1.000000000000000000, 0.9510565162951535312, 1.000000000000000000, 0.9510565162951535312, 1.000000000000000000, 0.9510565162951535312, 1.000000000000000000, 0.9510565162951535312, 1.000000000000000000, 0.9510565162951535312, 1.000000000000000000, 0.9510565162951535312, 1.000000000000000000, 0.9510565162951535312, 1.000000000000000000, 0.9510565162951535312, 1.000000000000000000, 0.9510565162951535312, 1.000000000000000000, 0.9510565162951535312, 1.000000000000000000, 0.9510565162951535312, 1.000000000000000000, 0.9510565162951535312, 1.000000000000000000, 0.9510565162951535312, 1.000000000000000000, 0.9510565162951535312, 1.000000000000000000, 0.9510565162951535312, 1.000000000000000000, 0.9510565162951535312, 1.000000000000000000, 0.9510565162951535312, 1.000000000000000000, 0.9510565162951535312, 1.000000000000000000, 0.9510565162951535312, 1.000000000000000000, 0.9510565162951535312, 1.000000000000000000, 0.9510565162951535312, 1.000000000000000000, 0.9510565162951535312, 1.000000000000000000, 0.9510565162951535312, 1.000000000000000000, 0.9510565162951535312, 1.000000000000000000, 0.9510565162951535312, 1.000000000000000000, 0.9510565162951535312, 1.000000000000000000, 0.9510565162951535312, 1.000000000000000000, 0.9510565162951535312, 1.000000000000000000, 0.9510565162951535312, 1.000000000000000000, 0.9510565162951535312, 1.000000000000000000, 0.9510565162951535312, 1.000000000000000000, 0.9510565162951535312, 1.000000000000000000, 0.9510565162951535312, 1.000000000000000000, 0.9510565162951535312, 1.000000000000000000, 0.9510565162951535312, 1.000000000000000000, 0.9510565162951535312, 1.000000000000000000, 0.9510565162951535312, 1.000000000000000000, 0.9510565162951535312, 1.000000000000000000, 0.9510565162951535312, 1.000000000000000000, 0.9510565162951535312, 1.000000000000000000, 0.9510565162951535312, 1.000000000000000000, 0.9510565162951535312, 1.000000000000000000, 0.9510565162951535312, 1.000000000000000000, 0.9510565162951535312, 1.000000000000000000, 0.9510565162951535312, 1.000000000000000000, 0.9510565162951535312, 1.000000000000000000, 0.9510565162951535312, 1.000000000000000000, 0.9510565162951535312, 1.000000000000000000, 0.9510565162951535312, 1.000000000000000000, 0.9510565162951535312, 1.000000000000000000, 0.9510565162951535312, 1.000000000000000000, 0.9510565162951535312, 1.000000000000000000, 0.9510565162951535312, 1.000000000000000000, 0.9573764855735520385, 0.9889922301674716199 ) ) 
 REPRESENTATION_ITEM ( '' )  );
#7578 = CARTESIAN_POINT ( 'NONE',  ( 18.94512977948575738, 4.924999997268808549, 13.76444248337723408 ) ) ;
#7579 = ORIENTED_EDGE ( 'NONE', *, *, #20795, .F. ) ;
#7580 = CARTESIAN_POINT ( 'NONE',  ( 10.37757302488624767, 73.97500000273119269, 31.93888565452638417 ) ) ;
#7581 = TOROIDAL_SURFACE ( 'NONE', #28853, 30.16025403784430736, 3.500000000000010658 ) ;
#7582 = CARTESIAN_POINT ( 'NONE',  ( -2.092463501923844636E-15, 26.00000000546237899, -34.17252228774368916 ) ) ;
#7583 = CARTESIAN_POINT ( 'NONE',  ( -30.02300923189239512, 45.94531249999997868, 2.654126918244515359E-13 ) ) ;
#7584 = CARTESIAN_POINT ( 'NONE',  ( 2.740863092043355209E-13, 58.83593750000000000, 30.02300923189239512 ) ) ;
#7585 = CARTESIAN_POINT ( 'NONE',  ( 10.37757302488624056, 54.77500000273119696, -31.93888565452638417 ) ) ;
#7586 = CARTESIAN_POINT ( 'NONE',  ( 32.50000000000000000, 63.50000000546238255, -3.980102097228898626E-15 ) ) ;
#7587 = CARTESIAN_POINT ( 'NONE',  ( -32.50000000000000000, 10.40000000546237757, -10.55989012756945300 ) ) ;
#7588 = CARTESIAN_POINT ( 'NONE',  ( 20.75514604977249178, 41.82500000273119412, 28.56700777964553950 ) ) ;
#7589 = CARTESIAN_POINT ( 'NONE',  ( 32.50000000000000711, 54.90000000000001279, 10.55989012756945122 ) ) ;
#7590 = CARTESIAN_POINT ( 'NONE',  ( 6.486482029760649416E-15, 67.87500000273116996, 35.31076352940723240 ) ) ;
#7591 = CARTESIAN_POINT ( 'NONE',  ( 20.08610463437158344, 3.200000005462373398, 27.64615127144129403 ) ) ;
#7592 = CARTESIAN_POINT ( 'NONE',  ( 20.75514604977249178, 63.82500000273119412, 28.56700777964553950 ) ) ;
#7593 = CARTESIAN_POINT ( 'NONE',  ( -4.523095164977117273E-15, 18.62499999726881583, 24.62258325217400312 ) ) ;
#7594 = CARTESIAN_POINT ( 'NONE',  ( -10.04305231718578462, 44.39999999999999147, 30.90933677959249337 ) ) ;
#7595 = DIRECTION ( 'NONE',  ( -0.000000000000000000, 1.000000000000000000, -0.000000000000000000 ) ) ;
#7596 = CARTESIAN_POINT ( 'NONE',  ( 27.16883889988623935, 10.57500000273120477, -19.73931689729374384 ) ) ;
#7597 = CARTESIAN_POINT ( 'NONE',  ( -13.94119854578892514, 30.18451416574268720, 24.22776226481266448 ) ) ;
#7598 = CARTESIAN_POINT ( 'NONE',  ( -8.960552108402742093E-16, 80.87500000273116996, -14.63369212191046387 ) ) ;
#7599 = CARTESIAN_POINT ( 'NONE',  ( 10.37757302488624056, 76.77500000273118985, -31.93888565452638417 ) ) ;
#7600 = CARTESIAN_POINT ( 'NONE',  ( -20.75514604977248112, 77.67500000273119554, 28.56700777964554661 ) ) ;
#7601 = EDGE_LOOP ( 'NONE', ( #10702, #30997, #10575, #15483 ) ) ;
#7602 = CARTESIAN_POINT ( 'NONE',  ( -7.236395654485757944, 11.72499999726880837, -22.27133577429736988 ) ) ;
#7603 = CARTESIAN_POINT ( 'NONE',  ( 1.507698388325705758E-15, 3.124999997268809615, -24.62258325217400312 ) ) ;
#7604 = CARTESIAN_POINT ( 'NONE',  ( -6.988114217767819270, 48.66666666666666430, 26.07999730980490583 ) ) ;
#7605 = CARTESIAN_POINT ( 'NONE',  ( -27.16883889988624290, 60.92500000273119554, -19.73931689729374028 ) ) ;
#7606 = CARTESIAN_POINT ( 'NONE',  ( -33.58253175000000113, 15.37500000273118950, 0.000000000000000000 ) ) ;
#7607 = CARTESIAN_POINT ( 'NONE',  ( 20.75514604977249178, 2.075000002731186122, 28.56700777964553950 ) ) ;
#7608 = CARTESIAN_POINT ( 'NONE',  ( 27.95245687107223276, 33.91406249999998579, -2.463307335887066074E-13 ) ) ;
#7609 = CARTESIAN_POINT ( 'NONE',  ( 26.02091320914851025, 24.75298583425730925, -14.97647472619946463 ) ) ;
#7610 = CARTESIAN_POINT ( 'NONE',  ( -26.00068869287340334, 66.28385416666662877, 15.01150461594643382 ) ) ;
#7611 = CARTESIAN_POINT ( 'NONE',  ( -2.162160676586881955E-15, 4.625000002731192161, -35.31076352940723240 ) ) ;
#7612 = CARTESIAN_POINT ( 'NONE',  ( 21.77128556259169656, 51.99999999999997868, -24.67464075869979112 ) ) ;
#7613 = CARTESIAN_POINT ( 'NONE',  ( -26.29305231718578995, 40.20000000000000284, 19.10302069950538595 ) ) ;
#7614 = CARTESIAN_POINT ( 'NONE',  ( -20.75514604977248823, 44.82500000273118701, -28.56700777964554305 ) ) ;
#7615 = CARTESIAN_POINT ( 'NONE',  ( 7.236395654485755280, 10.22499999726880837, 22.27133577429736988 ) ) ;
#7616 = CARTESIAN_POINT ( 'NONE',  ( 20.08610463437158344, 21.20000000546238894, 27.64615127144129403 ) ) ;
#7617 = VERTEX_POINT ( 'NONE', #6849 ) ;
#7618 = CARTESIAN_POINT ( 'NONE',  ( -27.16883889988624290, 57.17500000273119554, -19.73931689729374028 ) ) ;
#7619 = CARTESIAN_POINT ( 'NONE',  ( -32.50000000000000000, 4.400000005462393560, -10.55989012756945300 ) ) ;
#7620 = CARTESIAN_POINT ( 'NONE',  ( -19.06425588902591173, 44.37538166759063785, -19.11951029504763611 ) ) ;
#7621 = CARTESIAN_POINT ( 'NONE',  ( 10.37757302488624056, 78.77500000273118985, -31.93888565452638417 ) ) ;
#7622 = ORIENTED_EDGE ( 'NONE', *, *, #765, .T. ) ;
#7623 = CARTESIAN_POINT ( 'NONE',  ( -27.16883889988623935, 25.32500000273117635, 19.73931689729374739 ) ) ;
#7624 = CARTESIAN_POINT ( 'NONE',  ( -2.584737979205441561E-13, 15.86718749999999645, -30.02300923189239512 ) ) ;
#7625 = ORIENTED_EDGE ( 'NONE', *, *, #17634, .T. ) ;
#7626 = CARTESIAN_POINT ( 'NONE',  ( 5.147494310547434893, 29.05125428700921475, 32.49999999999999289 ) ) ;
#7627 = CARTESIAN_POINT ( 'NONE',  ( 33.58253175000000113, 62.12500000273119127, -4.112674001490185761E-15 ) ) ;
#7628 = CARTESIAN_POINT ( 'NONE',  ( -20.50609665441004736, 42.93750000000000000, -20.50609665440969565 ) ) ;
#7629 = LINE ( 'NONE', #8297, #24513 ) ;
#7630 = CARTESIAN_POINT ( 'NONE',  ( 23.41746824999999887, 5.124999997268814056, 0.000000000000000000 ) ) ;
#7631 = CARTESIAN_POINT ( 'NONE',  ( -20.75514604977248112, 3.425000002731186655, 28.56700777964554661 ) ) ;
#7632 = SURFACE_STYLE_USAGE ( .BOTH. , #25489 ) ;
#7633 = CARTESIAN_POINT ( 'NONE',  ( 0.04044903255045854962, 57.39805583240935505, 30.02300923189239867 ) ) ;
#7634 = CARTESIAN_POINT ( 'NONE',  ( 0.000000000000000000, 80.00000000000001421, 0.000000000000000000 ) ) ;
#7635 = CARTESIAN_POINT ( 'NONE',  ( -28.01184896238304134, 63.27604166666667140, -7.505752307972844761 ) ) ;
#7636 = CARTESIAN_POINT ( 'NONE',  ( 4.023268246324634798E-14, 8.499999999999992895, -24.50000000000000355 ) ) ;
#7637 = CARTESIAN_POINT ( 'NONE',  ( 32.50000000000000711, 18.90000000000001634, 10.55989012756945122 ) ) ;
#7638 = CARTESIAN_POINT ( 'NONE',  ( -6.988114217768288228, 63.84895833333332860, -26.07999730980477437 ) ) ;
#7639 = CARTESIAN_POINT ( 'NONE',  ( 24.50000000000000000, 11.74999999453762989, 0.000000000000000000 ) ) ;
#7640 = CARTESIAN_POINT ( 'NONE',  ( -9.270509831248421762, 70.55000000546237970, 12.75976212528060039 ) ) ;
#7641 = CARTESIAN_POINT ( 'NONE',  ( 19.09188309203661049, 23.17187499999999289, -19.09188309203694445 ) ) ;
#7642 = CARTESIAN_POINT ( 'NONE',  ( -27.16883889988624290, 28.92500000273118133, -19.73931689729374028 ) ) ;
#7643 = CARTESIAN_POINT ( 'NONE',  ( -2.162160676586881955E-15, 78.62500000273115575, -35.31076352940723240 ) ) ;
#7644 = CARTESIAN_POINT ( 'NONE',  ( 10.37757302488624056, 34.77500000273118985, -31.93888565452638417 ) ) ;
#7645 = CARTESIAN_POINT ( 'NONE',  ( -27.16883889988623935, 21.57500000273118701, 19.73931689729374739 ) ) ;
#7646 = PRODUCT_DEFINITION ( 'UNKNOWN', '', #19203, #13396 ) ;
#7647 = CARTESIAN_POINT ( 'NONE',  ( -15.14183272437242067, 6.699999999999991296, -20.84094480462497856 ) ) ;
#7648 = CARTESIAN_POINT ( 'NONE',  ( -10.37757302488623701, 75.52500000273118985, 31.93888565452638417 ) ) ;
#7649 = CARTESIAN_POINT ( 'NONE',  ( -20.08610463437156923, 26.80000000546238326, 27.64615127144130113 ) ) ;
#7650 = CARTESIAN_POINT ( 'NONE',  ( 26.29305231718578995, 59.20000000000001705, -19.10302069950538240 ) ) ;
#7651 = DIRECTION ( 'NONE',  ( -0.000000000000000000, -1.000000000000000000, -0.000000000000000000 ) ) ;
#7652 = CARTESIAN_POINT ( 'NONE',  ( 20.75514604977248467, 66.42500000273119554, -28.56700777964554305 ) ) ;
#7653 = CARTESIAN_POINT ( 'NONE',  ( -14.47279130897151589, 11.82499999726882578, -19.92008829642072598 ) ) ;
#7654 = CARTESIAN_POINT ( 'NONE',  ( -20.75514604977248823, 75.07500000273118701, -28.56700777964554305 ) ) ;
#7655 = CARTESIAN_POINT ( 'NONE',  ( 10.37757302488624767, 9.725000002731187365, 31.93888565452638417 ) ) ;
#7656 = CARTESIAN_POINT ( 'NONE',  ( 7.236395654485760609, 17.52499999726880731, -22.27133577429736633 ) ) ;
#7657 = CARTESIAN_POINT ( 'NONE',  ( -7.025853678916393008, 19.16704833425730570, 26.06988505166735592 ) ) ;
#7658 = VERTEX_POINT ( 'NONE', #17326 ) ;
#7659 = CARTESIAN_POINT ( 'NONE',  ( 27.16883889988623935, 44.32500000273119412, -19.73931689729374384 ) ) ;
#7660 = VERTEX_POINT ( 'NONE', #4275 ) ;
#7661 = CARTESIAN_POINT ( 'NONE',  ( -26.00068869287368756, 39.35677083333331439, -15.01150461594595775 ) ) ;
#7662 = CARTESIAN_POINT ( 'NONE',  ( 2.667360163309149608E-15, 79.50000000000001421, -32.50000000000000000 ) ) ;
#7663 = CARTESIAN_POINT ( 'NONE',  ( -32.50000000000000000, 2.400000005462383790, -10.55989012756945478 ) ) ;
#7664 = CARTESIAN_POINT ( 'NONE',  ( 27.16883889988624290, 77.92500000273116711, 19.73931689729373673 ) ) ;
#7665 = CARTESIAN_POINT ( 'NONE',  ( 18.94512977948575738, 4.924999997268808549, 13.76444248337723408 ) ) ;
#7666 = CARTESIAN_POINT ( 'NONE',  ( 14.47279130897151767, 16.92499999726880944, -19.92008829642072598 ) ) ;
#7667 = CARTESIAN_POINT ( 'NONE',  ( 10.37757302488624767, 13.97500000273119092, 31.93888565452638417 ) ) ;
#7668 = CARTESIAN_POINT ( 'NONE',  ( 10.04305231718579705, 17.10000000546238397, 30.90933677959248982 ) ) ;
#7669 =( BOUNDED_CURVE ( )  B_SPLINE_CURVE ( 2, ( #18724, #11315, #8900, #3590, #13897, #8230, #21626 ),
 .UNSPECIFIED., .F., .T. ) 
 B_SPLINE_CURVE_WITH_KNOTS ( ( 3, 2, 2, 3 ),
 ( 0.000000000000000000, 0.01111111111111111154, 0.02222222222222222307, 0.02777777777777777971 ),
 .UNSPECIFIED. ) 
 CURVE ( )  GEOMETRIC_REPRESENTATION_ITEM ( )  RATIONAL_B_SPLINE_CURVE ( ( 1.000000000000000000, 0.9510565162951535312, 1.000000000000000000, 0.9510565162951535312, 1.000000000000000000, 0.9755282581475768211, 0.9755282581475768211 ) ) 
 REPRESENTATION_ITEM ( '' )  );
#7670 = CARTESIAN_POINT ( 'NONE',  ( 6.277390505771533514E-15, 68.50000000000002842, 34.17252228774368916 ) ) ;
#7671 = CARTESIAN_POINT ( 'NONE',  ( 4.635254915624209993, 77.65000000546237402, -14.26584774442730463 ) ) ;
#7672 = LINE ( 'NONE', #15232, #9934 ) ;
#7673 = CARTESIAN_POINT ( 'NONE',  ( -7.543491769121417612, 63.85454833425732346, 28.00173670424549499 ) ) ;
#7674 = CARTESIAN_POINT ( 'NONE',  ( 0.000000000000000000, 80.00000000000001421, 0.000000000000000000 ) ) ;
#7675 = CARTESIAN_POINT ( 'NONE',  ( -2.584737979205442066E-13, 43.36718749999999289, -30.02300923189239867 ) ) ;
#7676 = SHAPE_DEFINITION_REPRESENTATION ( #23580, #22108 ) ;
#7677 = CARTESIAN_POINT ( 'NONE',  ( 6.054684311146244891E-15, -72.44024934668307480, 0.000000000000000000 ) ) ;
#7678 = CARTESIAN_POINT ( 'NONE',  ( 23.41746824999999887, 15.12499999726882294, 0.000000000000000000 ) ) ;
#7679 = CARTESIAN_POINT ( 'NONE',  ( -32.50000000000000000, 9.899999999999979039, -10.55989012756945478 ) ) ;
#7680 = DIRECTION ( 'NONE',  ( -1.000000000000000000, 0.000000000000000000, 0.000000000000000000 ) ) ;
#7681 = CARTESIAN_POINT ( 'NONE',  ( -6.950374756619247307, 50.66628499907601935, 26.09010956794245217 ) ) ;
#7682 = CARTESIAN_POINT ( 'NONE',  ( -10.37757302488624411, 48.72500000273119269, -31.93888565452638417 ) ) ;
#7683 = CARTESIAN_POINT ( 'NONE',  ( -27.16883889988623935, 53.57500000273117280, 19.73931689729374739 ) ) ;
#7684 = CARTESIAN_POINT ( 'NONE',  ( 27.16883889988623935, 40.57500000273117280, -19.73931689729374384 ) ) ;
#7685 = CARTESIAN_POINT ( 'NONE',  ( 10.04305231718578817, 23.90000000546238468, -30.90933677959249337 ) ) ;
#7686 = CARTESIAN_POINT ( 'NONE',  ( -2.428612866367529427E-13, 12.42968749999999822, -27.95245687107223276 ) ) ;
#7687 = CARTESIAN_POINT ( 'NONE',  ( -24.50000000000000000, 9.000000000000007105, -3.000384657911015469E-15 ) ) ;
#7688 = EDGE_CURVE ( 'NONE', #23106, #2254, #12165, .T. ) ;
#7689 = FACE_OUTER_BOUND ( 'NONE', #32083, .T. ) ;
#7690 = CARTESIAN_POINT ( 'NONE',  ( 10.04305231718578817, 77.40000000000000568, -30.90933677959249337 ) ) ;
#7691 = CARTESIAN_POINT ( 'NONE',  ( 33.58253175000000113, 16.12500000273119127, -4.112674001490185761E-15 ) ) ;
#7692 = FACE_OUTER_BOUND ( 'NONE', #16866, .T. ) ;
#7693 = CARTESIAN_POINT ( 'NONE',  ( -7.570916362186215665, 13.14999999453761426, 23.30088464923126423 ) ) ;
#7694 = CARTESIAN_POINT ( 'NONE',  ( 0.000000000000000000, -20.99999999999998934, -24.50000000000000000 ) ) ;
#7695 = CARTESIAN_POINT ( 'NONE',  ( 19.11951029504797006, 22.59336833240935505, 19.06425588902558133 ) ) ;
#7696 = CARTESIAN_POINT ( 'NONE',  ( -20.08610463437156923, 36.80000000546239391, 27.64615127144130113 ) ) ;
#7697 = CYLINDRICAL_SURFACE ( 'NONE', #10687, 32.50000000000000000 ) ;
#7698 = CARTESIAN_POINT ( 'NONE',  ( -2.162160676586882350E-15, 28.62500000273117706, -35.31076352940722529 ) ) ;
#7699 = CARTESIAN_POINT ( 'NONE',  ( -24.20753774853730889, 42.22135416666666430, 13.97622843553633842 ) ) ;
#7700 = ORIENTED_EDGE ( 'NONE', *, *, #19161, .F. ) ;
#7701 = CARTESIAN_POINT ( 'NONE',  ( 10.37757302488624767, 63.72500000273119269, 31.93888565452638417 ) ) ;
#7702 = EDGE_CURVE ( 'NONE', #1605, #24457, #31673, .T. ) ;
#7703 = CARTESIAN_POINT ( 'NONE',  ( -7.505752307973343918, 46.66145833333332860, -28.01184896238290989 ) ) ;
#7704 = VERTEX_POINT ( 'NONE', #6093 ) ;
#7705 = CARTESIAN_POINT ( 'NONE',  ( 30.02300923189239512, 16.72656249999999645, -2.619432448724977703E-13 ) ) ;
#7706 = CARTESIAN_POINT ( 'NONE',  ( 26.02091320914851025, 11.00298583425731103, -14.97647472619946463 ) ) ;
#7707 = EDGE_LOOP ( 'NONE', ( #19523, #8826, #10165, #21519, #10914, #6095, #27150, #19146 ) ) ;
#7708 = CARTESIAN_POINT ( 'NONE',  ( 10.37757302488624767, 7.725000002731172266, 31.93888565452638417 ) ) ;
#7709 = CARTESIAN_POINT ( 'NONE',  ( 4.635254915624209993, 79.65000000546234560, -14.26584774442730463 ) ) ;
#7710 = CARTESIAN_POINT ( 'NONE',  ( 33.58253175000000113, 34.37500000273119127, -4.112674001490185761E-15 ) ) ;
#7711 = CARTESIAN_POINT ( 'NONE',  ( -32.50000000000000000, 38.50000000546238965, 0.000000000000000000 ) ) ;
#7712 = CARTESIAN_POINT ( 'NONE',  ( 12.13525491562421088, 74.80000000000003979, 8.816778784387095058 ) ) ;
#7713 = CARTESIAN_POINT ( 'NONE',  ( -28.01184896238304134, 66.71354166666665719, -7.505752307972844761 ) ) ;
#7714 = CARTESIAN_POINT ( 'NONE',  ( 33.58253175000000823, 24.02500000273117564, 10.91162601494192863 ) ) ;
#7715 = CARTESIAN_POINT ( 'NONE',  ( 40.00000000000000000, 66.99999999999998579, -23.09401076758505766 ) ) ;
#7716 = CARTESIAN_POINT ( 'NONE',  ( -20.75514604977248823, 49.07500000273117280, -28.56700777964554305 ) ) ;
#7717 = PRODUCT_CONTEXT ( 'NONE', #2651, 'mechanical' ) ;
#7718 = CARTESIAN_POINT ( 'NONE',  ( 10.04305231718579705, 32.60000000000000142, 30.90933677959248982 ) ) ;
#7719 = CARTESIAN_POINT ( 'NONE',  ( -26.29305231718578995, 26.20000000000000284, 19.10302069950538595 ) ) ;
#7720 = CARTESIAN_POINT ( 'NONE',  ( 24.50000000000000000, 8.000000000000007105, 0.000000000000000000 ) ) ;
#7721 = CARTESIAN_POINT ( 'NONE',  ( -10.37757302488623701, 71.52500000273120406, 31.93888565452638417 ) ) ;
#7722 = CARTESIAN_POINT ( 'NONE',  ( 24.50000000000000355, 1.849999994537612436, -7.960532557706203605 ) ) ;
#7723 = CARTESIAN_POINT ( 'NONE',  ( -20.08610463437156923, 38.29999999999999005, 27.64615127144130113 ) ) ;
#7724 = CARTESIAN_POINT ( 'NONE',  ( -2.162160676586882350E-15, 58.87500000273117706, -35.31076352940722529 ) ) ;
#7725 = PLANE ( 'NONE',  #6778 ) ;
#7726 = CARTESIAN_POINT ( 'NONE',  ( 27.16883889988624290, 11.92500000273116711, 19.73931689729373673 ) ) ;
#7727 = CARTESIAN_POINT ( 'NONE',  ( 0.04044903254993986036, 27.61756916759064140, -27.95245687107223986 ) ) ;
#7728 = CARTESIAN_POINT ( 'NONE',  ( -12.90513655866680587, 66.99999999999998579, -31.00393344628902881 ) ) ;
#7729 = CARTESIAN_POINT ( 'NONE',  ( -27.16883889988623935, 3.575000002731199000, 19.73931689729374739 ) ) ;
#7730 = CARTESIAN_POINT ( 'NONE',  ( 10.37757302488624056, 32.52500000273118985, -31.93888565452638417 ) ) ;
#7731 = CARTESIAN_POINT ( 'NONE',  ( 5.147494310547426899, 45.94874572391552903, -32.50000000000000000 ) ) ;
#7732 = CARTESIAN_POINT ( 'NONE',  ( 11.25946833292375793, 78.07500000273121543, -8.180482586598735395 ) ) ;
#7733 = CARTESIAN_POINT ( 'NONE',  ( -15.04653450569338524, 48.51784749907601935, -25.98046417659831775 ) ) ;
#7734 = CARTESIAN_POINT ( 'NONE',  ( -26.29305231718578995, 56.70000000546236407, 19.10302069950538595 ) ) ;
#7735 = CARTESIAN_POINT ( 'NONE',  ( -11.25946833292375793, 79.57500000273121543, 8.180482586598737171 ) ) ;
#7736 = CARTESIAN_POINT ( 'NONE',  ( 20.08610463437157279, 61.30000000000001137, -27.64615127144129758 ) ) ;
#7737 = CARTESIAN_POINT ( 'NONE',  ( -26.07999730980490583, 18.58854166666666430, -6.988114217767815717 ) ) ;
#7738 = CARTESIAN_POINT ( 'NONE',  ( 23.41746824999999887, 1.124999997268810725, 0.000000000000000000 ) ) ;
#7739 = CARTESIAN_POINT ( 'NONE',  ( -32.50000000000000000, 68.60000000546237686, 10.55989012756946366 ) ) ;
#7740 = CARTESIAN_POINT ( 'NONE',  ( -28.01184896238304134, 25.46354166666666430, -7.505752307972844761 ) ) ;
#7741 = CARTESIAN_POINT ( 'NONE',  ( 33.58253175000000113, 36.37500000273118417, -4.112674001490185761E-15 ) ) ;
#7742 = CARTESIAN_POINT ( 'NONE',  ( -23.41746825000000243, 10.22499999726881725, 7.608796670333725309 ) ) ;
#7743 = VERTEX_POINT ( 'NONE', #24459 ) ;
#7744 = CARTESIAN_POINT ( 'NONE',  ( 7.468012846824777284, 42.94309000092397355, 28.02196122052045268 ) ) ;
#7745 = CARTESIAN_POINT ( 'NONE',  ( 26.29305231718579350, 21.30000000546237970, 19.10302069950537529 ) ) ;
#7746 = CARTESIAN_POINT ( 'NONE',  ( -7.505752307973343918, 43.22395833333332860, -28.01184896238290989 ) ) ;
#7747 = CARTESIAN_POINT ( 'NONE',  ( -20.50609665441004736, 63.56249999999999289, -20.50609665440969565 ) ) ;
#7748 = CARTESIAN_POINT ( 'NONE',  ( -20.75514604977248823, 51.07500000273116569, -28.56700777964554305 ) ) ;
#7749 = CARTESIAN_POINT ( 'NONE',  ( 32.50000000000000000, 59.60000000546236976, -10.55989012756945833 ) ) ;
#7750 = ADVANCED_FACE ( 'NONE', ( #5599 ), #16415, .F. ) ;
#7751 = DIRECTION ( 'NONE',  ( -1.000000000000000000, -1.224646799147353454E-16, 0.000000000000000000 ) ) ;
#7752 = AXIS2_PLACEMENT_3D ( 'NONE', #17729, #25954, #33327 ) ;
#7753 = CARTESIAN_POINT ( 'NONE',  ( -2.162160676586881955E-15, 44.62500000273119838, -35.31076352940723240 ) ) ;
#7754 = CARTESIAN_POINT ( 'NONE',  ( -8.891200544363830713E-16, 75.75000000546238255, -15.00000000000000000 ) ) ;
#7755 = CARTESIAN_POINT ( 'NONE',  ( -33.58253175000000113, 65.47500000273117848, 10.91162601494193929 ) ) ;
#7756 = EDGE_CURVE ( 'NONE', #14241, #12812, #18989, .T. ) ;
#7757 = CARTESIAN_POINT ( 'NONE',  ( 20.08610463437157279, 1.800000005462388364, -27.64615127144129758 ) ) ;
#7758 = CARTESIAN_POINT ( 'NONE',  ( -10.37757302488623701, 63.52500000273118985, 31.93888565452638417 ) ) ;
#7759 = CARTESIAN_POINT ( 'NONE',  ( -28.01184896238304134, 15.15104166666666252, -7.505752307972844761 ) ) ;
#7760 = CARTESIAN_POINT ( 'NONE',  ( -32.50000000000000000, 43.90000000000001279, -10.55989012756945478 ) ) ;
#7761 = CARTESIAN_POINT ( 'NONE',  ( -14.47279130897152122, 5.924999997268808549, 19.92008829642072243 ) ) ;
#7762 = CARTESIAN_POINT ( 'NONE',  ( -27.16883889988624290, 9.175000002731191984, -19.73931689729374028 ) ) ;
#7763 = CYLINDRICAL_SURFACE ( 'NONE', #4142, 26.50000000000000355 ) ;
#7764 = CARTESIAN_POINT ( 'NONE',  ( -14.01125832528328985, 31.33034749907602290, -24.18731323226223040 ) ) ;
#7765 = CARTESIAN_POINT ( 'NONE',  ( 2.688165632520823219E-15, 71.37500000273119838, 14.63369212191046387 ) ) ;
#7766 = CARTESIAN_POINT ( 'NONE',  ( 9.270509831248425314, 74.95000000546237118, 12.75976212528059683 ) ) ;
#7767 = CYLINDRICAL_SURFACE ( 'NONE', #7893, 32.50000000000000000 ) ;
#7768 = CARTESIAN_POINT ( 'NONE',  ( -10.37757302488624411, 76.97500000273120691, -31.93888565452638417 ) ) ;
#7769 = ORIENTED_EDGE ( 'NONE', *, *, #1644, .F. ) ;
#7770 = CARTESIAN_POINT ( 'NONE',  ( 7.236395654485755280, 14.72499999726881192, 22.27133577429736988 ) ) ;
#7771 = CARTESIAN_POINT ( 'NONE',  ( -6.988114217768288228, 56.97395833333333570, -26.07999730980477437 ) ) ;
#7772 = CARTESIAN_POINT ( 'NONE',  ( -33.58253175000000113, 53.02500000273118985, -10.91162601494193218 ) ) ;
#7773 = CARTESIAN_POINT ( 'NONE',  ( -27.16883889988623935, 17.57500000273119767, 19.73931689729374739 ) ) ;
#7774 = CARTESIAN_POINT ( 'NONE',  ( 33.58253175000000113, 2.475000002731187809, -10.91162601494193751 ) ) ;
#7775 = CARTESIAN_POINT ( 'NONE',  ( 13.97622843553633842, 37.92447916666666430, 24.20753774853730889 ) ) ;
#7776 = CARTESIAN_POINT ( 'NONE',  ( 7.468012846824777284, 29.19309000092397000, 28.02196122052045268 ) ) ;
#7777 = CARTESIAN_POINT ( 'NONE',  ( 28.02196122052058413, 22.30690999907601579, 7.468012846824272799 ) ) ;
#7778 = CARTESIAN_POINT ( 'NONE',  ( 10.04305231718578817, 73.90000000546235981, -30.90933677959249337 ) ) ;
#7779 = CARTESIAN_POINT ( 'NONE',  ( 31.95463953835039206, 52.00000000000002842, 10.27070314127458772 ) ) ;
#7780 = AXIS2_PLACEMENT_3D ( 'NONE', #25350, #12307, #15584 ) ;
#7781 = CARTESIAN_POINT ( 'NONE',  ( -10.37757302488623701, 43.52500000273118275, 31.93888565452638417 ) ) ;
#7782 = CARTESIAN_POINT ( 'NONE',  ( -18.94512977948576093, 9.824999997268824004, 13.76444248337722698 ) ) ;
#7783 = CARTESIAN_POINT ( 'NONE',  ( -32.50000000000000000, 2.500000005462382546, 0.000000000000000000 ) ) ;
#7784 = ORIENTED_EDGE ( 'NONE', *, *, #10090, .T. ) ;
#7785 = CARTESIAN_POINT ( 'NONE',  ( 27.16883889988623935, 54.57500000273117280, -19.73931689729374384 ) ) ;
#7786 = CARTESIAN_POINT ( 'NONE',  ( 19.11951029504763611, 38.35975666759064495, -19.06425588902591173 ) ) ;
#7787 = CARTESIAN_POINT ( 'NONE',  ( 10.37757302488624767, 75.97500000273119269, 31.93888565452638417 ) ) ;
#7788 = EDGE_LOOP ( 'NONE', ( #3565, #9159, #26412, #199 ) ) ;
#7789 = CARTESIAN_POINT ( 'NONE',  ( 33.58253175000000823, 22.02500000273117919, 10.91162601494192863 ) ) ;
#7790 = CARTESIAN_POINT ( 'NONE',  ( 7.505752307972854531, 19.44791666666666075, -28.01184896238303423 ) ) ;
#7791 = EDGE_CURVE ( 'NONE', #2565, #12293, #4964, .T. ) ;
#7792 = ORIENTED_EDGE ( 'NONE', *, *, #6314, .T. ) ;
#7793 = FACE_BOUND ( 'NONE', #20692, .T. ) ;
#7794 = CARTESIAN_POINT ( 'NONE',  ( -33.58253175000000113, 61.02500000273118985, -10.91162601494193218 ) ) ;
#7795 = CARTESIAN_POINT ( 'NONE',  ( 20.50609665441005092, 51.53124999999999289, 20.50609665440969209 ) ) ;
#7796 = EDGE_CURVE ( 'NONE', #18361, #12435, #33209, .T. ) ;
#7797 = PLANE ( 'NONE',  #8634 ) ;
#7798 = CARTESIAN_POINT ( 'NONE',  ( -14.47279130897151767, 1.824999997268821783, -19.92008829642072598 ) ) ;
#7799 = CARTESIAN_POINT ( 'NONE',  ( 33.58253175000000823, 2.025000002731202287, 10.91162601494192863 ) ) ;
#7800 =( LENGTH_UNIT ( ) NAMED_UNIT ( * ) SI_UNIT ( .MILLI., .METRE. ) );
#7801 = CARTESIAN_POINT ( 'NONE',  ( -25.98046417659831420, 57.97097249907601935, 15.04653450569339945 ) ) ;
#7802 = CARTESIAN_POINT ( 'NONE',  ( 5.147494310547434893, 36.55125428154683220, 32.49999999999999289 ) ) ;
#7803 = CARTESIAN_POINT ( 'NONE',  ( -30.02300923189239867, 66.57031250000000000, 2.654126918244514854E-13 ) ) ;
#7804 = CARTESIAN_POINT ( 'NONE',  ( 26.29305231718579350, 75.30000000546237970, 19.10302069950537529 ) ) ;
#7805 = CARTESIAN_POINT ( 'NONE',  ( -20.08610463437156923, 14.29999999999998472, 27.64615127144130113 ) ) ;
#7806 = CARTESIAN_POINT ( 'NONE',  ( 6.988114217767829928, 57.26041666666666430, -26.07999730980489872 ) ) ;
#7807 = CARTESIAN_POINT ( 'NONE',  ( 24.50000000000000355, 11.64999999453762314, 7.960532557706212486 ) ) ;
#7808 = CARTESIAN_POINT ( 'NONE',  ( 15.00000000000000000, 71.25000000546238255, -1.836970198721029589E-15 ) ) ;
#7809 = CARTESIAN_POINT ( 'NONE',  ( 2.584737979205441561E-13, 31.33593749999999289, 27.95245687107222921 ) ) ;
#7810 = CARTESIAN_POINT ( 'NONE',  ( 33.58253175000000113, 34.22500000273117848, -10.91162601494193751 ) ) ;
#7811 = CARTESIAN_POINT ( 'NONE',  ( -20.75514604977248823, 74.82500000273115859, -28.56700777964554305 ) ) ;
#7812 = CARTESIAN_POINT ( 'NONE',  ( -27.16883889988623935, 33.57500000273118701, 19.73931689729374739 ) ) ;
#7813 = CARTESIAN_POINT ( 'NONE',  ( -33.58253175000000113, 13.37500000273117351, 0.000000000000000000 ) ) ;
#7814 = CARTESIAN_POINT ( 'NONE',  ( -10.04305231718578462, 64.40000000000000568, 30.90933677959249337 ) ) ;
#7815 = CARTESIAN_POINT ( 'NONE',  ( -27.95245687107223986, 50.82069416759063785, -0.04044903254993292840 ) ) ;
#7816 = CARTESIAN_POINT ( 'NONE',  ( -20.75514604977248112, 75.42500000273120975, 28.56700777964554661 ) ) ;
#7817 = CARTESIAN_POINT ( 'NONE',  ( -5.147494310547423346, 26.94874572391553613, 32.50000000000000000 ) ) ;
#7818 = VECTOR ( 'NONE', #1335, 1000.000000000000114 ) ;
#7819 = CARTESIAN_POINT ( 'NONE',  ( -32.50000000000000000, 57.89999999999999858, -10.55989012756945478 ) ) ;
#7820 = FACE_OUTER_BOUND ( 'NONE', #12602, .T. ) ;
#7821 = CARTESIAN_POINT ( 'NONE',  ( -10.37757302488623701, 61.52500000273120406, 31.93888565452638417 ) ) ;
#7822 = CIRCLE ( 'NONE', #16072, 31.22091420962414787 ) ;
#7823 = CARTESIAN_POINT ( 'NONE',  ( -18.94512977948575738, 7.924999997268811214, -13.76444248337723231 ) ) ;
#7824 = CARTESIAN_POINT ( 'NONE',  ( 20.75514604977249178, 76.07500000273118701, 28.56700777964553950 ) ) ;
#7825 = CARTESIAN_POINT ( 'NONE',  ( 6.486482029760648627E-15, 7.625000002731170845, 35.31076352940722529 ) ) ;
#7826 = CARTESIAN_POINT ( 'NONE',  ( -4.523095164977116484E-15, 2.124999997268812280, 24.62258325217400312 ) ) ;
#7827 = CARTESIAN_POINT ( 'NONE',  ( -24.18731323226248264, 16.73215250092398065, -14.01125832528284931 ) ) ;
#7828 = EDGE_LOOP ( 'NONE', ( #373, #24739 ) ) ;
#7829 = CARTESIAN_POINT ( 'NONE',  ( 33.58253175000000823, 42.02500000273118985, 10.91162601494192863 ) ) ;
#7830 = ORIENTED_EDGE ( 'NONE', *, *, #16499, .T. ) ;
#7831 = CARTESIAN_POINT ( 'NONE',  ( -20.50609665440969209, 38.64062500000000000, 20.50609665441005092 ) ) ;
#7832 = CARTESIAN_POINT ( 'NONE',  ( 24.50000000000000000, 10.10000000000000142, -7.960532557706203605 ) ) ;
#7833 = CARTESIAN_POINT ( 'NONE',  ( 20.08610463437157279, 1.800000005462373709, -27.64615127144129758 ) ) ;
#7834 = CARTESIAN_POINT ( 'NONE',  ( 32.50000000000000000, 27.60000000546238752, -10.55989012756945833 ) ) ;
#7835 = CARTESIAN_POINT ( 'NONE',  ( 7.505752307973351023, 24.31770833333332504, 28.01184896238290278 ) ) ;
#7836 = CARTESIAN_POINT ( 'NONE',  ( -23.41746825000000243, 17.52499999726881796, -7.608796670333730638 ) ) ;
#7837 = CARTESIAN_POINT ( 'NONE',  ( 27.16883889988624290, 14.17500000273119731, 19.73931689729373673 ) ) ;
#7838 = TOROIDAL_SURFACE ( 'NONE', #27017, 12.11000150615021553, 1.999999999999992228 ) ;
#7839 = CARTESIAN_POINT ( 'NONE',  ( 6.277390505771533514E-15, 62.50000000000000000, 34.17252228774368916 ) ) ;
#7840 = CARTESIAN_POINT ( 'NONE',  ( 2.375766604868040144, 76.80125428700922896, 15.00000000000000178 ) ) ;
#7841 = FACE_OUTER_BOUND ( 'NONE', #11089, .T. ) ;
#7842 = CARTESIAN_POINT ( 'NONE',  ( -26.02091320914878025, 31.04388916574268364, -14.97647472619899389 ) ) ;
#7843 = CARTESIAN_POINT ( 'NONE',  ( -13.91746824999999887, 79.37500000273118417, 0.000000000000000000 ) ) ;
#7844 = CARTESIAN_POINT ( 'NONE',  ( 7.505752307972854531, 40.07291666666666430, -28.01184896238303423 ) ) ;
#7845 = AXIS2_PLACEMENT_3D ( 'NONE', #33545, #28231, #5233 ) ;
#7846 = DIRECTION ( 'NONE',  ( -1.224646799147353454E-16, 1.000000000000000000, -0.000000000000000000 ) ) ;
#7847 = CARTESIAN_POINT ( 'NONE',  ( 15.14183272437242067, 15.69999999999999929, 20.84094480462498211 ) ) ;
#7848 = CARTESIAN_POINT ( 'NONE',  ( 26.29305231718578995, 5.199999999999982414, -19.10302069950538240 ) ) ;
#7849 = DIRECTION ( 'NONE',  ( -1.000000000000000000, 0.000000000000000000, 0.000000000000000000 ) ) ;
#7850 = CARTESIAN_POINT ( 'NONE',  ( 26.06988505166722803, 52.95795166574269075, -7.025853678916862854 ) ) ;
#7851 = CARTESIAN_POINT ( 'NONE',  ( -10.37757302488623701, 49.52500000273118985, 31.93888565452638417 ) ) ;
#7852 = CARTESIAN_POINT ( 'NONE',  ( 6.486482029760649416E-15, 53.87500000273118417, 35.31076352940723240 ) ) ;
#7853 = CARTESIAN_POINT ( 'NONE',  ( -2.162160676586882350E-15, 38.87500000273120548, -35.31076352940722529 ) ) ;
#7854 = DIRECTION ( 'NONE',  ( 0.000000000000000000, 0.000000000000000000, 1.000000000000000000 ) ) ;
#7855 = CARTESIAN_POINT ( 'NONE',  ( 13.97622843553589966, 16.15364583333333215, -24.20753774853756113 ) ) ;
#7856 = FACE_OUTER_BOUND ( 'NONE', #25257, .T. ) ;
#7857 = CARTESIAN_POINT ( 'NONE',  ( -31.22091420962414787, -23.06066017177981919, 0.000000000000000000 ) ) ;
#7858 = CARTESIAN_POINT ( 'NONE',  ( -33.58253175000000113, 15.12500000273118950, 0.000000000000000000 ) ) ;
#7859 = DIRECTION ( 'NONE',  ( 0.000000000000000000, 1.000000000000000000, 0.000000000000000000 ) ) ;
#7860 = CARTESIAN_POINT ( 'NONE',  ( -7.570916362186210335, 12.34999999453761887, -23.30088464923126779 ) ) ;
#7861 = CARTESIAN_POINT ( 'NONE',  ( -1.778240108872766143E-15, 2.000000005462374997, -32.49999999999999289 ) ) ;
#7862 = CARTESIAN_POINT ( 'NONE',  ( 26.06988505166722803, 22.02045166574269075, -7.025853678916862854 ) ) ;
#7863 = CARTESIAN_POINT ( 'NONE',  ( -20.08610463437157989, 34.20000000546238539, -27.64615127144129758 ) ) ;
#7864 = CARTESIAN_POINT ( 'NONE',  ( 3.880418787951178228, 18.19874571299077104, -24.49999999999998224 ) ) ;
#7865 = CARTESIAN_POINT ( 'NONE',  ( 33.58253175000000823, 26.02500000273120406, 10.91162601494192685 ) ) ;
#7866 = CARTESIAN_POINT ( 'NONE',  ( 26.07999730980490227, 44.36979166666666430, 6.988114217767821046 ) ) ;
#7867 = EDGE_LOOP ( 'NONE', ( #26364, #32979 ) ) ;
#7868 = CARTESIAN_POINT ( 'NONE',  ( -33.58253175000000113, 65.22500000273117848, 10.91162601494193929 ) ) ;
#7869 = CARTESIAN_POINT ( 'NONE',  ( 20.50609665441005092, 44.65624999999999289, 20.50609665440969209 ) ) ;
#7870 =( BOUNDED_CURVE ( )  B_SPLINE_CURVE ( 2, ( #9534, #6624, #20016, #1629, #20190, #32859, #1983, #27732, #12107, #30633, #4388, #15039, #22579 ),
 .UNSPECIFIED., .F., .T. ) 
 B_SPLINE_CURVE_WITH_KNOTS ( ( 3, 2, 2, 2, 2, 2, 3 ),
 ( 0.5961538461538461453, 0.5974358974358974228, 0.5999999999999999778, 0.6025641025641025328, 0.6051282051282050878, 0.6076923076923076428, 0.6089743589743590313 ),
 .UNSPECIFIED. ) 
 CURVE ( )  GEOMETRIC_REPRESENTATION_ITEM ( )  RATIONAL_B_SPLINE_CURVE ( ( 0.9755282581475768211, 0.9755282581475768211, 1.000000000000000000, 0.9510565162951535312, 1.000000000000000000, 0.9510565162951535312, 1.000000000000000000, 0.9510565162951535312, 1.000000000000000000, 0.9510565162951535312, 1.000000000000000000, 0.9755282581475757109, 0.9755282581475768211 ) ) 
 REPRESENTATION_ITEM ( '' )  );
#7871 = ORIENTED_EDGE ( 'NONE', *, *, #9567, .T. ) ;
#7872 = CARTESIAN_POINT ( 'NONE',  ( 28.01184896238290278, 16.58333333333333215, -7.505752307973347470 ) ) ;
#7873 = CARTESIAN_POINT ( 'NONE',  ( 25.98046417659858420, 15.01340250092397888, 15.04653450569292872 ) ) ;
#7874 = EDGE_LOOP ( 'NONE', ( #5423, #14037, #6758, #31965 ) ) ;
#7875 = CARTESIAN_POINT ( 'NONE',  ( 27.16883889988624290, 3.925000002731188431, 19.73931689729373673 ) ) ;
#7876 = CARTESIAN_POINT ( 'NONE',  ( 7.236395654485760609, 1.024999997268821739, -22.27133577429736633 ) ) ;
#7877 = CARTESIAN_POINT ( 'NONE',  ( -33.58253175000000113, 37.27500000273119696, -10.91162601494193218 ) ) ;
#7878 = CARTESIAN_POINT ( 'NONE',  ( -26.29305231718579350, 36.30000000546237970, -19.10302069950537884 ) ) ;
#7879 = CARTESIAN_POINT ( 'NONE',  ( -20.08610463437157989, 75.69999999999998863, -27.64615127144129758 ) ) ;
#7880 = CARTESIAN_POINT ( 'NONE',  ( 2.740863092043355209E-13, 65.71093749999997158, 30.02300923189239512 ) ) ;
#7881 = CARTESIAN_POINT ( 'NONE',  ( 27.16883889988624290, 19.92500000273117422, 19.73931689729373673 ) ) ;
#7882 = CARTESIAN_POINT ( 'NONE',  ( 3.880418787951150694, 6.198745712990782586, -24.49999999999999645 ) ) ;
#7883 = CARTESIAN_POINT ( 'NONE',  ( -33.58253175000000113, 51.47500000273118559, 10.91162601494193929 ) ) ;
#7884 = EDGE_CURVE ( 'NONE', #9893, #24093, #27312, .T. ) ;
#7885 = CARTESIAN_POINT ( 'NONE',  ( -20.08610463437157989, 21.69999999999998153, -27.64615127144129758 ) ) ;
#7886 = CARTESIAN_POINT ( 'NONE',  ( 26.29305231718579350, 28.79999999999999361, 19.10302069950537529 ) ) ;
#7887 = CARTESIAN_POINT ( 'NONE',  ( -24.50000000000000355, 6.900000000000014566, -7.960532557706207157 ) ) ;
#7888 = CARTESIAN_POINT ( 'NONE',  ( -20.75514604977248112, 67.42500000273118133, 28.56700777964554661 ) ) ;
#7889 = CARTESIAN_POINT ( 'NONE',  ( -24.50000000000001066, 2.849999994537639303, 7.960532557706201828 ) ) ;
#7890 = AXIS2_PLACEMENT_3D ( 'NONE', #31624, #8122, #16032 ) ;
#7891 = CARTESIAN_POINT ( 'NONE',  ( -3.859555026111434639, 74.00000000000001421, -14.20191393030580151 ) ) ;
#7892 = CARTESIAN_POINT ( 'NONE',  ( 10.37757302488624767, 59.97500000273120691, 31.93888565452638417 ) ) ;
#7893 = AXIS2_PLACEMENT_3D ( 'NONE', #10517, #18253, #18424 ) ;
#7894 = EDGE_CURVE ( 'NONE', #18620, #6224, #31838, .T. ) ;
#7895 = ADVANCED_FACE ( 'NONE', ( #26704, #3201 ), #8501, .T. ) ;
#7896 = CARTESIAN_POINT ( 'NONE',  ( -1.778240108872766143E-15, 36.00000000546238255, -32.49999999999999289 ) ) ;
#7897 = CARTESIAN_POINT ( 'NONE',  ( -20.75514604977248112, 11.42500000273116711, 28.56700777964554661 ) ) ;
#7898 = CARTESIAN_POINT ( 'NONE',  ( 19.11951029504763611, 28.04725666759063429, -19.06425588902591173 ) ) ;
#7899 = CARTESIAN_POINT ( 'NONE',  ( -33.58253175000000113, 5.475000002731180260, 10.91162601494193929 ) ) ;
#7900 = CARTESIAN_POINT ( 'NONE',  ( 33.58253175000000113, 36.22500000273119980, -10.91162601494193751 ) ) ;
#7901 = CYLINDRICAL_SURFACE ( 'NONE', #8375, 32.50000000000000000 ) ;
#7902 = DIRECTION ( 'NONE',  ( 1.000000000000000000, 0.000000000000000000, 0.000000000000000000 ) ) ;
#7903 = ADVANCED_FACE ( 'NONE', ( #4196 ), #14881, .T. ) ;
#7904 = CARTESIAN_POINT ( 'NONE',  ( 12.86449124955741041, 74.00000000000001421, -5.310441354522136947 ) ) ;
#7905 = CARTESIAN_POINT ( 'NONE',  ( 28.02196122052058413, 49.80690999907602645, 7.468012846824272799 ) ) ;
#7906 = CARTESIAN_POINT ( 'NONE',  ( 26.29305231718578995, 55.70000000546236407, -19.10302069950538240 ) ) ;
#7907 = CARTESIAN_POINT ( 'NONE',  ( 13.91746825000000065, 78.27500000273118985, 4.522059556121114987 ) ) ;
#7908 = PRESENTATION_STYLE_ASSIGNMENT (( #24042 ) ) ;
#7909 = CARTESIAN_POINT ( 'NONE',  ( -13.97622843553588901, 21.30989583333331794, 24.20753774853756823 ) ) ;
#7910 = CARTESIAN_POINT ( 'NONE',  ( 23.41746825000000243, 1.224999997268811480, -7.608796670333727974 ) ) ;
#7911 = CARTESIAN_POINT ( 'NONE',  ( -32.50000000000000000, 68.40000000546237402, -10.55989012756945478 ) ) ;
#7912 = CARTESIAN_POINT ( 'NONE',  ( 2.740863092043355209E-13, 24.46093749999999645, 30.02300923189239512 ) ) ;
#7913 = CARTESIAN_POINT ( 'NONE',  ( -10.37757302488623701, 31.77500000273118630, 31.93888565452638417 ) ) ;
#7914 = CARTESIAN_POINT ( 'NONE',  ( -23.41746824999999887, 14.02499999726881263, -7.608796670333730638 ) ) ;
#7915 = EDGE_LOOP ( 'NONE', ( #1051, #15161, #19943, #28255 ) ) ;
#7916 = CARTESIAN_POINT ( 'NONE',  ( -28.02196122052045268, 36.92746500092395934, 7.468012846824790607 ) ) ;
#7917 = CARTESIAN_POINT ( 'NONE',  ( -32.50000000000000000, 18.40000000546238823, -10.55989012756945478 ) ) ;
#7918 = CARTESIAN_POINT ( 'NONE',  ( 2.740863092043355209E-13, 55.39843749999999289, 30.02300923189239512 ) ) ;
#7919 = CYLINDRICAL_SURFACE ( 'NONE', #933, 32.50000000000000000 ) ;
#7920 = CARTESIAN_POINT ( 'NONE',  ( 27.16883889988623935, 56.57500000273118701, -19.73931689729374384 ) ) ;
#7921 = CARTESIAN_POINT ( 'NONE',  ( 32.50000000000000711, 59.40000000546237402, 10.55989012756945122 ) ) ;
#7922 = CARTESIAN_POINT ( 'NONE',  ( 12.11000150615021909, -45.00000000000000000, 1.483047458217648827E-15 ) ) ;
#7923 = CARTESIAN_POINT ( 'NONE',  ( -10.37757302488623701, 41.52500000273118275, 31.93888565452638417 ) ) ;
#7924 = CARTESIAN_POINT ( 'NONE',  ( 26.29305231718579350, 54.80000000000001847, 19.10302069950537529 ) ) ;
#7925 = CARTESIAN_POINT ( 'NONE',  ( 20.75514604977248467, 70.67500000273118133, -28.56700777964554305 ) ) ;
#7926 = CARTESIAN_POINT ( 'NONE',  ( 8.122944958617804190, 74.00000000000000000, 11.31021757173031972 ) ) ;
#7927 = CARTESIAN_POINT ( 'NONE',  ( 27.16883889988624290, 61.92500000273119554, 19.73931689729373673 ) ) ;
#7928 = CARTESIAN_POINT ( 'NONE',  ( -20.50609665440969209, 24.89062500000000000, 20.50609665441005092 ) ) ;
#7929 = CARTESIAN_POINT ( 'NONE',  ( 10.04305231718579705, 46.60000000000000142, 30.90933677959248982 ) ) ;
#7930 = CARTESIAN_POINT ( 'NONE',  ( 7.236395654485760609, 7.024999997268826846, -22.27133577429736633 ) ) ;
#7931 = CARTESIAN_POINT ( 'NONE',  ( -33.58253175000000113, 9.375000002731169957, 0.000000000000000000 ) ) ;
#7932 = LINE ( 'NONE', #18420, #8532 ) ;
#7933 = CARTESIAN_POINT ( 'NONE',  ( -26.06988505166722803, 30.61420166574267654, 7.025853678916877953 ) ) ;
#7934 = DIRECTION ( 'NONE',  ( -3.169619151431772337E-17, -0.9659258262890680902, -0.2588190451025213501 ) ) ;
#7935 = CARTESIAN_POINT ( 'NONE',  ( 0.000000000000000000, -21.99999999999999645, 0.000000000000000000 ) ) ;
#7936 = LINE ( 'NONE', #26638, #11116 ) ;
#7937 = CARTESIAN_POINT ( 'NONE',  ( -33.58253175000000113, 75.37500000273118417, 0.000000000000000000 ) ) ;
#7938 = VERTEX_POINT ( 'NONE', #27880 ) ;
#7939 = LINE ( 'NONE', #14435, #31018 ) ;
#7940 =( GEOMETRIC_REPRESENTATION_CONTEXT ( 3 ) GLOBAL_UNCERTAINTY_ASSIGNED_CONTEXT ( ( #21957 ) ) GLOBAL_UNIT_ASSIGNED_CONTEXT ( ( #13404, #23535, #13226 ) ) REPRESENTATION_CONTEXT ( 'NONE', 'WORKASPACE' ) );
#7941 = CARTESIAN_POINT ( 'NONE',  ( -26.07999730980477437, 62.98958333333332149, 6.988114217768305103 ) ) ;
#7942 = CARTESIAN_POINT ( 'NONE',  ( 33.58253175000000823, 56.02500000273117564, 10.91162601494192863 ) ) ;
#7943 = CARTESIAN_POINT ( 'NONE',  ( 27.16883889988623935, 16.57500000273119767, -19.73931689729374384 ) ) ;
#7944 = CARTESIAN_POINT ( 'NONE',  ( 20.75514604977249178, 4.075000002731181681, 28.56700777964553950 ) ) ;
#7945 = CARTESIAN_POINT ( 'NONE',  ( -13.97622843553632777, 39.64322916666667140, -24.20753774853731599 ) ) ;
#7946 = CARTESIAN_POINT ( 'NONE',  ( -28.02196122052045268, 26.61496500092397355, 7.468012846824790607 ) ) ;
#7947 = CARTESIAN_POINT ( 'NONE',  ( -26.02091320914878025, 20.73138916574268720, -14.97647472619899389 ) ) ;
#7948 = CARTESIAN_POINT ( 'NONE',  ( -32.50000000000000000, 74.50000000546238255, 0.000000000000000000 ) ) ;
#7949 = EDGE_CURVE ( 'NONE', #8542, #17164, #15010, .T. ) ;
#7950 = CARTESIAN_POINT ( 'NONE',  ( 31.08180318173147327, 52.00000000000001421, -11.59917702625707214 ) ) ;
#7951 = CARTESIAN_POINT ( 'NONE',  ( 20.75514604977249178, 39.82500000273116569, 28.56700777964553950 ) ) ;
#7952 = CARTESIAN_POINT ( 'NONE',  ( 24.22776226481265383, 46.51263916574269786, 13.94119854578893580 ) ) ;
#7953 = CARTESIAN_POINT ( 'NONE',  ( -7.236395654485757944, 11.22499999726880837, -22.27133577429736988 ) ) ;
#7954 = CARTESIAN_POINT ( 'NONE',  ( -4.223320258572819786E-15, 3.499999999999996891, 24.50000000000000000 ) ) ;
#7955 = VERTEX_POINT ( 'NONE', #30609 ) ;
#7956 = CARTESIAN_POINT ( 'NONE',  ( -20.75514604977248112, 53.67500000273119554, 28.56700777964554661 ) ) ;
#7957 = CARTESIAN_POINT ( 'NONE',  ( -26.29305231718578995, 50.70000000546237828, 19.10302069950538595 ) ) ;
#7958 = CARTESIAN_POINT ( 'NONE',  ( 27.95245687107223986, 42.22694416759065206, 0.04044903254993640479 ) ) ;
#7959 = CARTESIAN_POINT ( 'NONE',  ( -27.16883889988624290, 75.17500000273119554, -19.73931689729374028 ) ) ;
#7960 = EDGE_LOOP ( 'NONE', ( #9858, #8046, #27487, #896 ) ) ;
#7961 = CARTESIAN_POINT ( 'NONE',  ( 20.75514604977249178, 21.82500000273119056, 28.56700777964553950 ) ) ;
#7962 = CARTESIAN_POINT ( 'NONE',  ( -20.50609665440969209, 18.01562499999999645, 20.50609665441005092 ) ) ;
#7963 = VECTOR ( 'NONE', #22596, 1000.000000000000000 ) ;
#7964 = ORIENTED_EDGE ( 'NONE', *, *, #10518, .T. ) ;
#7965 = CARTESIAN_POINT ( 'NONE',  ( 32.50000000000000000, 29.50000000546237899, -3.980102097228898626E-15 ) ) ;
#7966 = CARTESIAN_POINT ( 'NONE',  ( 33.58253175000000113, 58.22500000273116427, -10.91162601494193751 ) ) ;
#7967 = CARTESIAN_POINT ( 'NONE',  ( 26.00068869287367335, 51.38802083333332149, 15.01150461594596308 ) ) ;
#7968 = CARTESIAN_POINT ( 'NONE',  ( -24.50000000000000355, 16.89999999999998437, -7.960532557706207157 ) ) ;
#7969 = CARTESIAN_POINT ( 'NONE',  ( -23.41746825000000243, 8.224999997268822582, 7.608796670333725309 ) ) ;
#7970 = CARTESIAN_POINT ( 'NONE',  ( 33.58253175000000113, 4.225000002731190030, -10.91162601494193751 ) ) ;
#7971 = CARTESIAN_POINT ( 'NONE',  ( -0.04044903255044120238, 59.11680583240937636, -30.02300923189239867 ) ) ;
#7972 = CARTESIAN_POINT ( 'NONE',  ( 20.08610463437158344, 36.70000000000000284, 27.64615127144129403 ) ) ;
#7973 = CARTESIAN_POINT ( 'NONE',  ( 0.000000000000000000, -12.99999999999999822, 0.000000000000000000 ) ) ;
#7974 = CARTESIAN_POINT ( 'NONE',  ( 26.29305231718578995, 9.199999999999985079, -19.10302069950538240 ) ) ;
#7975 = CARTESIAN_POINT ( 'NONE',  ( -2.092463501923844636E-15, 13.50000000000001066, -34.17252228774368916 ) ) ;
#7976 = CARTESIAN_POINT ( 'NONE',  ( -24.20753774853756823, 59.98177083333332860, -13.97622843553588723 ) ) ;
#7977 = CARTESIAN_POINT ( 'NONE',  ( -14.47279130897151589, 1.824999997268821339, -19.92008829642072598 ) ) ;
#7978 = CARTESIAN_POINT ( 'NONE',  ( -9.270509831248425314, 73.95000000546238539, -12.75976212528059861 ) ) ;
#7979 = CARTESIAN_POINT ( 'NONE',  ( -2.428612866367529427E-13, 36.49218750000000000, -27.95245687107222921 ) ) ;
#7980 = CARTESIAN_POINT ( 'NONE',  ( 33.58253175000000113, 24.12500000273118417, -4.112674001490185761E-15 ) ) ;
#7981 = CARTESIAN_POINT ( 'NONE',  ( 33.58253175000000113, 70.12500000273118417, -4.112674001490185761E-15 ) ) ;
#7982 = CARTESIAN_POINT ( 'NONE',  ( 10.37757302488624056, 38.77500000273119696, -31.93888565452638417 ) ) ;
#7983 = CARTESIAN_POINT ( 'NONE',  ( 27.16883889988623935, 14.57500000273120833, -19.73931689729374384 ) ) ;
#7984 = CARTESIAN_POINT ( 'NONE',  ( 1.555960095263670572E-15, 6.499999999999994671, -24.50000000000000000 ) ) ;
#7985 = CARTESIAN_POINT ( 'NONE',  ( 7.025853678916403666, 58.69829833425730925, -26.06988505166735237 ) ) ;
#7986 = CARTESIAN_POINT ( 'NONE',  ( -33.58253175000000113, 79.12500000273119838, 0.000000000000000000 ) ) ;
#7987 =( GEOMETRIC_REPRESENTATION_CONTEXT ( 3 ) GLOBAL_UNCERTAINTY_ASSIGNED_CONTEXT ( ( #18089 ) ) GLOBAL_UNIT_ASSIGNED_CONTEXT ( ( #1877, #9779, #20430 ) ) REPRESENTATION_CONTEXT ( 'NONE', 'WORKASPACE' ) );
#7988 = CARTESIAN_POINT ( 'NONE',  ( 7.570916362186207671, 7.599999999999996092, 23.30088464923126779 ) ) ;
#7989 = ADVANCED_FACE ( 'NONE', ( #27706 ), #3856, .T. ) ;
#7990 = CARTESIAN_POINT ( 'NONE',  ( -10.04305231718579172, 53.60000000000002274, -30.90933677959248982 ) ) ;
#7991 = CARTESIAN_POINT ( 'NONE',  ( -18.94512977948576093, 17.82499999726880446, 13.76444248337722698 ) ) ;
#7992 = CARTESIAN_POINT ( 'NONE',  ( -10.37757302488623701, 57.52500000273119696, 31.93888565452638417 ) ) ;
#7993 = EDGE_CURVE ( 'NONE', #25120, #4231, #15506, .T. ) ;
#7994 = CARTESIAN_POINT ( 'NONE',  ( 18.94512977948576093, 7.324999997268822227, -13.76444248337722875 ) ) ;
#7995 = ORIENTED_EDGE ( 'NONE', *, *, #20351, .F. ) ;
#7996 = CARTESIAN_POINT ( 'NONE',  ( 33.58253175000000823, 76.27500000273118985, 10.91162601494192863 ) ) ;
#7997 = CARTESIAN_POINT ( 'NONE',  ( 10.37757302488624056, 4.525000002731205839, -31.93888565452638417 ) ) ;
#7998 = AXIS2_PLACEMENT_3D ( 'NONE', #32435, #29863, #16842 ) ;
#7999 = CARTESIAN_POINT ( 'NONE',  ( 18.94512977948575738, 16.92499999726882010, 13.76444248337723408 ) ) ;
#8000 = CARTESIAN_POINT ( 'NONE',  ( -6.950374756619716266, 17.16184000092397000, -26.09010956794232428 ) ) ;
#8001 = ORIENTED_EDGE ( 'NONE', *, *, #22244, .F. ) ;
#8002 = CARTESIAN_POINT ( 'NONE',  ( -27.16883889988623935, 41.32500000273119412, 19.73931689729374739 ) ) ;
#8003 = CYLINDRICAL_SURFACE ( 'NONE', #30195, 15.00000000000000000 ) ;
#8004 = EDGE_LOOP ( 'NONE', ( #27492, #23500, #28300, #4322, #32708, #32999, #17114, #25849, #17588, #2038, #14746, #20765, #14705, #25472, #4318, #20484, #27329, #15784, #9811, #31943, #14328 ) ) ;
#8005 = CARTESIAN_POINT ( 'NONE',  ( -15.01150461594642138, 43.08072916666666430, -26.00068869287340334 ) ) ;
#8006 = LINE ( 'NONE', #18660, #18812 ) ;
#8007 = CARTESIAN_POINT ( 'NONE',  ( -2.092463501923844636E-15, 4.000000005462377217, -34.17252228774368916 ) ) ;
#8008 = CARTESIAN_POINT ( 'NONE',  ( 26.29305231718579350, 27.30000000546237260, 19.10302069950537529 ) ) ;
#8009 = CARTESIAN_POINT ( 'NONE',  ( -15.01150461594595775, 21.30989583333331794, 26.00068869287368756 ) ) ;
#8010 = CARTESIAN_POINT ( 'NONE',  ( 14.47279130897151589, 16.32499999726879736, 19.92008829642072953 ) ) ;
#8011 = CARTESIAN_POINT ( 'NONE',  ( 33.58253175000000823, 6.275000002731184523, 10.91162601494192863 ) ) ;
#8012 = CARTESIAN_POINT ( 'NONE',  ( 20.08610463437158344, 60.70000000000000284, 27.64615127144129403 ) ) ;
#8013 = CARTESIAN_POINT ( 'NONE',  ( -4.300734207923759378, 78.47500000273119269, -13.23629886949340495 ) ) ;
#8014 = CARTESIAN_POINT ( 'NONE',  ( 10.04305231718579705, 73.10000000546237686, 30.90933677959248982 ) ) ;
#8015 = CARTESIAN_POINT ( 'NONE',  ( -7.543491769121917656, 34.91107666574267654, -28.00173670424536354 ) ) ;
#8016 = CARTESIAN_POINT ( 'NONE',  ( -13.91746824999999532, 73.47500000273117848, 4.522059556121122093 ) ) ;
#8017 = CARTESIAN_POINT ( 'NONE',  ( -28.01184896238290278, 42.36458333333332860, 7.505752307973363457 ) ) ;
#8018 = CONTEXT_DEPENDENT_SHAPE_REPRESENTATION ( #19728, #1596 ) ;
#8019 = CARTESIAN_POINT ( 'NONE',  ( -15.14183272437242778, 13.29999999999998650, 20.84094480462497856 ) ) ;
#8020 = CARTESIAN_POINT ( 'NONE',  ( -26.29305231718579350, 3.799999999999998046, -19.10302069950537884 ) ) ;
#8021 = CARTESIAN_POINT ( 'NONE',  ( 5.814984965855610735E-15, -70.48295565631028126, 0.000000000000000000 ) ) ;
#8022 = CARTESIAN_POINT ( 'NONE',  ( 0.04044903255044120238, 64.27305583240934084, 27.95245687107223276 ) ) ;
#8023 = CARTESIAN_POINT ( 'NONE',  ( 33.58253175000000823, 52.02500000273118985, 10.91162601494192863 ) ) ;
#8024 = CARTESIAN_POINT ( 'NONE',  ( -15.00000000000000000, 70.25000000546238255, 0.000000000000000000 ) ) ;
#8025 = CARTESIAN_POINT ( 'NONE',  ( -2.162160676586881955E-15, 58.87500000273117706, -35.31076352940723240 ) ) ;
#8026 = CARTESIAN_POINT ( 'NONE',  ( 27.16883889988624290, 32.17500000273118843, 19.73931689729373673 ) ) ;
#8027 = CARTESIAN_POINT ( 'NONE',  ( 5.147494310547434893, 24.55125428154685707, 32.49999999999999289 ) ) ;
#8028 = LINE ( 'NONE', #31363, #13921 ) ;
#8029 = CARTESIAN_POINT ( 'NONE',  ( 10.04305231718578817, 15.90000000546237757, -30.90933677959249337 ) ) ;
#8030 = CARTESIAN_POINT ( 'NONE',  ( -10.04305231718578462, 22.90000000546238468, 30.90933677959249337 ) ) ;
#8031 = CARTESIAN_POINT ( 'NONE',  ( -32.50000000000000000, 74.10000000000002274, 10.55989012756946366 ) ) ;
#8032 = CARTESIAN_POINT ( 'NONE',  ( 33.58253175000000823, 14.02500000273117209, 10.91162601494192863 ) ) ;
#8033 = CARTESIAN_POINT ( 'NONE',  ( 23.41746824999999887, 0.7249999972688272454, -7.608796670333727974 ) ) ;
#8034 = CARTESIAN_POINT ( 'NONE',  ( -13.94119854578892514, 16.43451416574268720, 24.22776226481266448 ) ) ;
#8035 = ADVANCED_FACE ( 'NONE', ( #14330 ), #1776, .F. ) ;
#8036 = CARTESIAN_POINT ( 'NONE',  ( -26.29305231718579350, 34.30000000546239391, -19.10302069950537884 ) ) ;
#8037 = EDGE_CURVE ( 'NONE', #23284, #15393, #27510, .T. ) ;
#8038 = CARTESIAN_POINT ( 'NONE',  ( -27.16883889988623935, 23.32500000273118701, 19.73931689729374739 ) ) ;
#8039 = CARTESIAN_POINT ( 'NONE',  ( 19.09188309203661049, 47.23437499999999289, -19.09188309203694445 ) ) ;
#8040 = ORIENTED_EDGE ( 'NONE', *, *, #16915, .T. ) ;
#8041 = CARTESIAN_POINT ( 'NONE',  ( -20.75514604977248823, 64.82500000273120122, -28.56700777964554305 ) ) ;
#8042 = EDGE_LOOP ( 'NONE', ( #4534, #24009, #8001, #1886 ) ) ;
#8043 = CARTESIAN_POINT ( 'NONE',  ( 20.50609665440969565, 12.85937500000000000, -20.50609665441004736 ) ) ;
#8044 = CARTESIAN_POINT ( 'NONE',  ( -28.02196122052045268, 16.30246500092397355, 7.468012846824790607 ) ) ;
#8045 = CARTESIAN_POINT ( 'NONE',  ( 6.486482029760649416E-15, 3.625000002731194826, 35.31076352940723240 ) ) ;
#8046 = ORIENTED_EDGE ( 'NONE', *, *, #7796, .T. ) ;
#8047 = CYLINDRICAL_SURFACE ( 'NONE', #5338, 32.50000000000000000 ) ;
#8048 = AXIS2_PLACEMENT_3D ( 'NONE', #2875, #10428, #15413 ) ;
#8049 = CARTESIAN_POINT ( 'NONE',  ( 27.16883889988624290, 32.17500000273118843, 19.73931689729373673 ) ) ;
#8050 = CARTESIAN_POINT ( 'NONE',  ( 32.50000000000000000, 35.50000000546238255, -3.980102097228898626E-15 ) ) ;
#8051 = CARTESIAN_POINT ( 'NONE',  ( 15.00000000000000355, 72.90000000000001990, 4.873795443493592394 ) ) ;
#8052 = DIRECTION ( 'NONE',  ( 0.000000000000000000, 1.000000000000000000, 0.000000000000000000 ) ) ;
#8053 = CARTESIAN_POINT ( 'NONE',  ( 32.50000000000000000, 77.00000000000001421, -3.980102097228898626E-15 ) ) ;
#8054 = CARTESIAN_POINT ( 'NONE',  ( -33.58253175000000113, 47.27500000273116143, -10.91162601494193218 ) ) ;
#8055 = VECTOR ( 'NONE', #27113, 1000.000000000000000 ) ;
#8056 = CARTESIAN_POINT ( 'NONE',  ( -20.08610463437156923, 24.29999999999999005, 27.64615127144130113 ) ) ;
#8057 = CARTESIAN_POINT ( 'NONE',  ( -10.04305231718579172, 21.60000000000000853, -30.90933677959248982 ) ) ;
#8058 = CARTESIAN_POINT ( 'NONE',  ( 24.50000000000000000, 6.000000000000005329, 0.000000000000000000 ) ) ;
#8059 = CARTESIAN_POINT ( 'NONE',  ( -27.16883889988624290, 66.92500000273119554, -19.73931689729374028 ) ) ;
#8060 = CARTESIAN_POINT ( 'NONE',  ( -23.28634348215024730, 66.99999999999997158, 23.32808161240111389 ) ) ;
#8061 = CARTESIAN_POINT ( 'NONE',  ( -2.986717648272234182, 74.00000000000000000, -14.37702829354413581 ) ) ;
#8062 = CARTESIAN_POINT ( 'NONE',  ( -33.58253175000000113, 55.27500000273121117, -10.91162601494193041 ) ) ;
#8063 = DIRECTION ( 'NONE',  ( 1.000000000000000000, 0.000000000000000000, -0.000000000000000000 ) ) ;
#8064 = CARTESIAN_POINT ( 'NONE',  ( 6.486482029760649416E-15, 9.625000002731196602, 35.31076352940723240 ) ) ;
#8065 = CARTESIAN_POINT ( 'NONE',  ( 6.950374756619721595, 32.63059000092395934, 26.09010956794232428 ) ) ;
#8066 = CARTESIAN_POINT ( 'NONE',  ( 8.342407680043388396, 66.99999999999997158, -32.16802901964491213 ) ) ;
#8067 = CARTESIAN_POINT ( 'NONE',  ( -10.37757302488624411, 4.975000002731183812, -31.93888565452638417 ) ) ;
#8068 = CARTESIAN_POINT ( 'NONE',  ( 10.37757302488624767, 35.72500000273119980, 31.93888565452638417 ) ) ;
#8069 = CARTESIAN_POINT ( 'NONE',  ( 32.50000000000000711, 45.40000000546237402, 10.55989012756945122 ) ) ;
#8070 = CARTESIAN_POINT ( 'NONE',  ( 0.000000000000000000, 86.00000000000001421, 0.000000000000000000 ) ) ;
#8071 = CARTESIAN_POINT ( 'NONE',  ( 11.25946833292375793, 75.67500000273119554, 8.180482586598731842 ) ) ;
#8072 = CARTESIAN_POINT ( 'NONE',  ( 14.97647472619900455, 45.65326416574269786, -26.02091320914876960 ) ) ;
#8073 = CARTESIAN_POINT ( 'NONE',  ( 26.29305231718578995, 51.70000000546236407, -19.10302069950538240 ) ) ;
#8074 = CARTESIAN_POINT ( 'NONE',  ( 13.91746824999999887, 78.37500000273116996, -1.704398294459741270E-15 ) ) ;
#8075 = SHAPE_REPRESENTATION ( 'Linear Compliance Spring & Shaft', ( #1376 ), #13943 ) ;
#8076 = CARTESIAN_POINT ( 'NONE',  ( 26.29305231718579350, 60.79999999999999005, 19.10302069950537529 ) ) ;
#8077 = CARTESIAN_POINT ( 'NONE',  ( 26.07999730980477437, 16.58333333333333215, -6.988114217768290004 ) ) ;
#8078 = CARTESIAN_POINT ( 'NONE',  ( -23.41746824999999887, 8.124999997268817609, -2.867812753649727150E-15 ) ) ;
#8079 = AXIS2_PLACEMENT_3D ( 'NONE', #16861, #27321, #20637 ) ;
#8080 = CARTESIAN_POINT ( 'NONE',  ( 10.04305231718579705, 67.10000000546237686, 30.90933677959248982 ) ) ;
#8081 = CARTESIAN_POINT ( 'NONE',  ( -2.584737979205441561E-13, 19.30468749999999645, -30.02300923189239512 ) ) ;
#8082 = CARTESIAN_POINT ( 'NONE',  ( 27.16883889988623935, 28.57500000273117990, -19.73931689729374384 ) ) ;
#8083 = CARTESIAN_POINT ( 'NONE',  ( -14.47279130897151767, 15.82499999726881512, -19.92008829642072598 ) ) ;
#8084 = EDGE_LOOP ( 'NONE', ( #1415, #5974, #24260, #1815 ) ) ;
#8085 = CARTESIAN_POINT ( 'NONE',  ( -20.47846945139902175, 40.93788166759063785, -20.53372385742072481 ) ) ;
#8086 = CARTESIAN_POINT ( 'NONE',  ( 6.277390505771533514E-15, 19.00000000546236834, 34.17252228774368916 ) ) ;
#8087 = CARTESIAN_POINT ( 'NONE',  ( 26.00068869287367335, 51.38802083333332149, 15.01150461594596308 ) ) ;
#8088 = CARTESIAN_POINT ( 'NONE',  ( -32.50000000000000000, 36.00000000000000711, 0.000000000000000000 ) ) ;
#8089 = CARTESIAN_POINT ( 'NONE',  ( 20.75514604977248467, 52.67500000273116711, -28.56700777964554305 ) ) ;
#8090 = CARTESIAN_POINT ( 'NONE',  ( -32.50000000000000000, 58.40000000546237402, -10.55989012756945478 ) ) ;
#8091 = CARTESIAN_POINT ( 'NONE',  ( -4.300734207923755825, 77.77500000273118985, 13.23629886949340673 ) ) ;
#8092 = CARTESIAN_POINT ( 'NONE',  ( -33.58253175000000113, 39.22500000273119269, 10.91162601494193929 ) ) ;
#8093 = CARTESIAN_POINT ( 'NONE',  ( 0.000000000000000000, 80.00000000000001421, 0.000000000000000000 ) ) ;
#8094 = CARTESIAN_POINT ( 'NONE',  ( 27.16883889988624290, 68.17500000273119554, 19.73931689729373673 ) ) ;
#8095 = CARTESIAN_POINT ( 'NONE',  ( 12.86449124955741041, 74.00000000000001421, -5.310441354522136947 ) ) ;
#8096 = CARTESIAN_POINT ( 'NONE',  ( 27.16883889988624290, 59.92500000273119554, 19.73931689729373673 ) ) ;
#8097 = CARTESIAN_POINT ( 'NONE',  ( 15.01150461594596486, 23.02864583333332504, -26.00068869287367690 ) ) ;
#8098 = CARTESIAN_POINT ( 'NONE',  ( -10.04305231718579172, 47.60000000000000142, -30.90933677959248982 ) ) ;
#8099 = CARTESIAN_POINT ( 'NONE',  ( 18.94512977948576093, 6.824999997268821339, -13.76444248337722875 ) ) ;
#8100 = CARTESIAN_POINT ( 'NONE',  ( -10.37757302488624411, 8.975000002731187365, -31.93888565452638417 ) ) ;
#8101 = CARTESIAN_POINT ( 'NONE',  ( 20.08610463437158344, 35.20000000546238539, 27.64615127144129403 ) ) ;
#8102 = CARTESIAN_POINT ( 'NONE',  ( 14.01125832528330051, 33.04909749907601935, 24.18731323226221974 ) ) ;
#8103 = CARTESIAN_POINT ( 'NONE',  ( -13.91746824999999532, 71.47500000273119269, 4.522059556121122093 ) ) ;
#8104 = CARTESIAN_POINT ( 'NONE',  ( 33.58253175000000113, 78.37500000273116996, -4.112674001490185761E-15 ) ) ;
#8105 = CARTESIAN_POINT ( 'NONE',  ( -1.631291757790872152E-15, 111.9999999999999858, -13.32050807568876927 ) ) ;
#8106 = CARTESIAN_POINT ( 'NONE',  ( -10.37757302488624411, 72.97500000273120691, -31.93888565452638417 ) ) ;
#8107 = ORIENTED_EDGE ( 'NONE', *, *, #19434, .F. ) ;
#8108 = CYLINDRICAL_SURFACE ( 'NONE', #23366, 15.00000000000000000 ) ;
#8109 = CARTESIAN_POINT ( 'NONE',  ( 24.20753774853731244, 57.69010416666667140, -13.97622843553632599 ) ) ;
#8110 = CARTESIAN_POINT ( 'NONE',  ( -10.37757302488623701, 55.52500000273118275, 31.93888565452638417 ) ) ;
#8111 = CARTESIAN_POINT ( 'NONE',  ( 27.16883889988624290, 20.17500000273118843, 19.73931689729373673 ) ) ;
#8112 = CARTESIAN_POINT ( 'NONE',  ( -20.75514604977248823, 78.82500000273120122, -28.56700777964554305 ) ) ;
#8113 = CARTESIAN_POINT ( 'NONE',  ( 2.584737979205442066E-13, 45.08593750000000000, 27.95245687107223276 ) ) ;
#8114 = CARTESIAN_POINT ( 'NONE',  ( -20.47846945139902175, 27.18788166759063785, -20.53372385742072481 ) ) ;
#8115 = CARTESIAN_POINT ( 'NONE',  ( 20.53372385742108008, 19.15586833240934794, 20.47846945139866648 ) ) ;
#8116 = CARTESIAN_POINT ( 'NONE',  ( -32.50000000000000000, 70.60000000546234844, 10.55989012756946366 ) ) ;
#8117 = EDGE_CURVE ( 'NONE', #21143, #33174, #11578, .T. ) ;
#8118 = CARTESIAN_POINT ( 'NONE',  ( -20.08610463437156923, 56.80000000546240102, 27.64615127144130113 ) ) ;
#8119 = CARTESIAN_POINT ( 'NONE',  ( 10.37757302488624767, 41.72500000273118559, 31.93888565452638417 ) ) ;
#8120 = CARTESIAN_POINT ( 'NONE',  ( 14.01125832528330051, 46.79909749907603356, 24.18731323226221974 ) ) ;
#8121 = CARTESIAN_POINT ( 'NONE',  ( 18.94512977948575738, 18.42499999726882010, 13.76444248337723408 ) ) ;
#8122 = DIRECTION ( 'NONE',  ( -0.000000000000000000, -1.000000000000000000, -0.000000000000000000 ) ) ;
#8123 = ORIENTED_EDGE ( 'NONE', *, *, #4947, .F. ) ;
#8124 = CARTESIAN_POINT ( 'NONE',  ( 27.16883889988623935, 50.57500000273117280, -19.73931689729374384 ) ) ;
#8125 = CARTESIAN_POINT ( 'NONE',  ( -32.50000000000000000, 50.40000000546236691, -10.55989012756945300 ) ) ;
#8126 = CARTESIAN_POINT ( 'NONE',  ( -26.06988505166735237, 47.52642333425731636, -7.025853678916388567 ) ) ;
#8127 = CARTESIAN_POINT ( 'NONE',  ( 10.37757302488624767, 69.97500000273119269, 31.93888565452638417 ) ) ;
#8128 = ORIENTED_EDGE ( 'NONE', *, *, #17702, .F. ) ;
#8129 = CARTESIAN_POINT ( 'NONE',  ( 20.75514604977248467, 22.42500000273119909, -28.56700777964554305 ) ) ;
#8130 = CARTESIAN_POINT ( 'NONE',  ( -26.00068869287368756, 29.04427083333332504, -15.01150461594595775 ) ) ;
#8131 = VECTOR ( 'NONE', #23794, 1000.000000000000000 ) ;
#8132 = ORIENTED_EDGE ( 'NONE', *, *, #5517, .F. ) ;
#8133 = CARTESIAN_POINT ( 'NONE',  ( -20.08610463437157989, 48.20000000546237118, -27.64615127144129758 ) ) ;
#8134 = CARTESIAN_POINT ( 'NONE',  ( 6.486482029760649416E-15, 63.62500000273117706, 35.31076352940723240 ) ) ;
#8135 = CARTESIAN_POINT ( 'NONE',  ( 20.50609665440969565, 47.23437499999999289, -20.50609665441004736 ) ) ;
#8136 = CARTESIAN_POINT ( 'NONE',  ( -26.29305231718578995, 66.70000000546238539, 19.10302069950538595 ) ) ;
#8137 = CARTESIAN_POINT ( 'NONE',  ( -23.41746824999999887, 10.12499999726881938, -2.867812753649727150E-15 ) ) ;
#8138 = CARTESIAN_POINT ( 'NONE',  ( -33.58253175000000113, 5.025000002731194293, -10.91162601494193218 ) ) ;
#8139 = CARTESIAN_POINT ( 'NONE',  ( 33.58253175000000823, 28.27500000273118985, 10.91162601494192863 ) ) ;
#8140 =( NAMED_UNIT ( * ) SI_UNIT ( $, .STERADIAN. ) SOLID_ANGLE_UNIT ( ) );
#8141 = CARTESIAN_POINT ( 'NONE',  ( -7.468012846824272799, 64.41628499907602645, 28.02196122052058413 ) ) ;
#8142 = CARTESIAN_POINT ( 'NONE',  ( 8.891200544363830713E-16, 79.75000000546236834, -15.00000000000000000 ) ) ;
#8143 = CARTESIAN_POINT ( 'NONE',  ( -1.778240108872766143E-15, 31.49999999999998579, -32.49999999999999289 ) ) ;
#8144 = CARTESIAN_POINT ( 'NONE',  ( -5.147494310547430452, 59.55125428154684641, -32.49999999999999289 ) ) ;
#8145 = CARTESIAN_POINT ( 'NONE',  ( -32.50000000000000000, 15.89999999999999147, -10.55989012756945478 ) ) ;
#8146 = CARTESIAN_POINT ( 'NONE',  ( -27.95245687107223276, 59.69531250000000711, 2.498001805406602216E-13 ) ) ;
#8147 = CARTESIAN_POINT ( 'NONE',  ( 23.41746824999999887, 3.124999997268812280, 0.000000000000000000 ) ) ;
#8148 = CARTESIAN_POINT ( 'NONE',  ( -13.91746824999999887, 78.87500000273118417, 0.000000000000000000 ) ) ;
#8149 = CARTESIAN_POINT ( 'NONE',  ( -24.20753774853730889, 28.47135416666666075, 13.97622843553633842 ) ) ;
#8150 = CARTESIAN_POINT ( 'NONE',  ( 33.58253175000000823, 22.02500000273117919, 10.91162601494192863 ) ) ;
#8151 = CARTESIAN_POINT ( 'NONE',  ( -10.37757302488623701, 73.52500000273120406, 31.93888565452638417 ) ) ;
#8152 = CARTESIAN_POINT ( 'NONE',  ( 27.16883889988623935, 36.57500000273118701, -19.73931689729374384 ) ) ;
#8153 = CARTESIAN_POINT ( 'NONE',  ( 33.58253175000000113, 16.37500000273117706, -4.112674001490185761E-15 ) ) ;
#8154 = CARTESIAN_POINT ( 'NONE',  ( -13.94119854578936923, 61.70611083425731636, -24.22776226481241224 ) ) ;
#8155 = CARTESIAN_POINT ( 'NONE',  ( 33.58253175000000113, 68.22500000273116427, -10.91162601494193574 ) ) ;
#8156 = DIRECTION ( 'NONE',  ( 0.2583678462756386907, 0.9660466117175132705, 3.164093559440564356E-17 ) ) ;
#8157 = CARTESIAN_POINT ( 'NONE',  ( 26.29305231718578995, 55.20000000000000995, -19.10302069950538240 ) ) ;
#8158 = CARTESIAN_POINT ( 'NONE',  ( -27.16883889988623935, 57.32500000273119412, 19.73931689729374739 ) ) ;
#8159 = CARTESIAN_POINT ( 'NONE',  ( 23.41746825000000243, 7.024999997268802865, 7.608796670333735079 ) ) ;
#8160 = ORIENTED_EDGE ( 'NONE', *, *, #30246, .T. ) ;
#8161 = CARTESIAN_POINT ( 'NONE',  ( -10.37757302488623701, 63.77500000273118985, 31.93888565452638417 ) ) ;
#8162 = CARTESIAN_POINT ( 'NONE',  ( -27.16883889988623935, 1.325000002731169246, 19.73931689729374739 ) ) ;
#8163 = CARTESIAN_POINT ( 'NONE',  ( 14.47279130897151589, 2.324999997268805796, 19.92008829642072953 ) ) ;
#8164 = CARTESIAN_POINT ( 'NONE',  ( 26.09010956794232428, 14.58371500092397710, -6.950374756619718042 ) ) ;
#8165 = ORIENTED_EDGE ( 'NONE', *, *, #21677, .T. ) ;
#8166 = CARTESIAN_POINT ( 'NONE',  ( -10.37757302488623701, 43.52500000273119696, 31.93888565452638417 ) ) ;
#8167 = CARTESIAN_POINT ( 'NONE',  ( -5.147494310547423346, 42.94874572391552192, 32.50000000000000000 ) ) ;
#8168 = ORIENTED_EDGE ( 'NONE', *, *, #16781, .F. ) ;
#8169 = CARTESIAN_POINT ( 'NONE',  ( 30.02300923189239512, 40.78906249999998579, -2.619432448724977703E-13 ) ) ;
#8170 = CARTESIAN_POINT ( 'NONE',  ( 6.277390505771533514E-15, 5.000000005462374553, 34.17252228774368916 ) ) ;
#8171 = CARTESIAN_POINT ( 'NONE',  ( 27.16883889988623935, 78.32500000273118701, -19.73931689729374384 ) ) ;
#8172 = CARTESIAN_POINT ( 'NONE',  ( -30.02300923189239512, 18.44531249999999645, 2.654126918244515359E-13 ) ) ;
#8173 = CARTESIAN_POINT ( 'NONE',  ( -14.47279130897151589, 15.32499999726880269, -19.92008829642072598 ) ) ;
#8174 = CARTESIAN_POINT ( 'NONE',  ( 27.16883889988623935, 10.57500000273120477, -19.73931689729374384 ) ) ;
#8175 = EDGE_CURVE ( 'NONE', #3689, #3647, #9327, .T. ) ;
#8176 = CARTESIAN_POINT ( 'NONE',  ( -10.04305231718579172, 59.59999999999998721, -30.90933677959248982 ) ) ;
#8177 = CARTESIAN_POINT ( 'NONE',  ( 13.91746824999999887, 75.87500000273116996, -1.704398294459741270E-15 ) ) ;
#8178 = CARTESIAN_POINT ( 'NONE',  ( 19.82091636218621034, 1.799999999999996048, 14.40073868116559730 ) ) ;
#8179 = CARTESIAN_POINT ( 'NONE',  ( 14.97647472619900455, 35.34076416574268364, -26.02091320914876960 ) ) ;
#8180 = CARTESIAN_POINT ( 'NONE',  ( -11.25946833292375793, 75.17500000273119554, -8.180482586598733619 ) ) ;
#8181 = CARTESIAN_POINT ( 'NONE',  ( -7.505752307973343918, 53.53645833333332860, -28.01184896238290989 ) ) ;
#8182 = EDGE_CURVE ( 'NONE', #21850, #1559, #11088, .T. ) ;
#8183 = DIRECTION ( 'NONE',  ( -1.000000000000000000, -1.087251435804610394E-16, 0.000000000000000000 ) ) ;
#8184 = CARTESIAN_POINT ( 'NONE',  ( 24.50000000000000000, 16.00000000000001421, 0.000000000000000000 ) ) ;
#8185 = CARTESIAN_POINT ( 'NONE',  ( 10.04305231718578817, 3.400000000000014122, -30.90933677959249337 ) ) ;
#8186 = CARTESIAN_POINT ( 'NONE',  ( 32.50000000000000711, 17.40000000546238823, 10.55989012756945122 ) ) ;
#8187 = CARTESIAN_POINT ( 'NONE',  ( 26.09010956794244507, 60.11940999907602645, 6.950374756619249084 ) ) ;
#8188 = CARTESIAN_POINT ( 'NONE',  ( 33.58253175000000113, 44.12500000273117706, -4.112674001490185761E-15 ) ) ;
#8189 = CARTESIAN_POINT ( 'NONE',  ( 12.13525491562420910, 73.45000000546237118, -8.816778784387098611 ) ) ;
#8190 = CARTESIAN_POINT ( 'NONE',  ( -20.75514604977248112, 57.67500000273118133, 28.56700777964554661 ) ) ;
#8191 = CARTESIAN_POINT ( 'NONE',  ( 10.37757302488624056, 34.77500000273120406, -31.93888565452638417 ) ) ;
#8192 = CARTESIAN_POINT ( 'NONE',  ( 0.000000000000000000, 52.00000000000000711, 32.50000000000000000 ) ) ;
#8193 = CARTESIAN_POINT ( 'NONE',  ( -13.97622843553632777, 22.45572916666666430, -24.20753774853731599 ) ) ;
#8194 = CARTESIAN_POINT ( 'NONE',  ( 19.82091636218621034, 11.54999999453762349, 14.40073868116559730 ) ) ;
#8195 = DIRECTION ( 'NONE',  ( -1.224646799147353454E-16, 1.000000000000000000, -0.000000000000000000 ) ) ;
#8196 = CARTESIAN_POINT ( 'NONE',  ( 6.277390505771533514E-15, 72.50000000000001421, 34.17252228774368916 ) ) ;
#8197 = CARTESIAN_POINT ( 'NONE',  ( -27.16883889988623935, 13.32500000273119412, 19.73931689729374739 ) ) ;
#8198 = CARTESIAN_POINT ( 'NONE',  ( 1.507698388325705758E-15, 5.124999997268805174, -24.62258325217400312 ) ) ;
#8199 = CARTESIAN_POINT ( 'NONE',  ( -5.147494310547423346, 40.44874571845314648, 32.50000000000000000 ) ) ;
#8200 = CARTESIAN_POINT ( 'NONE',  ( -13.94119854578892514, 23.30951416574269075, 24.22776226481266448 ) ) ;
#8201 = CARTESIAN_POINT ( 'NONE',  ( -10.04305231718579172, 34.10000000546238397, -30.90933677959248982 ) ) ;
#8202 = CARTESIAN_POINT ( 'NONE',  ( -20.08610463437156923, 12.29999999999999183, 27.64615127144130113 ) ) ;
#8203 = CARTESIAN_POINT ( 'NONE',  ( -20.75514604977248112, 19.42500000273117777, 28.56700777964554661 ) ) ;
#8204 = CARTESIAN_POINT ( 'NONE',  ( 6.988114217768294445, 44.94270833333332860, 26.07999730980477437 ) ) ;
#8205 = ORIENTED_EDGE ( 'NONE', *, *, #31314, .F. ) ;
#8206 = CARTESIAN_POINT ( 'NONE',  ( 20.75514604977248467, 60.42500000273118133, -28.56700777964554305 ) ) ;
#8207 = ORIENTED_EDGE ( 'NONE', *, *, #31700, .T. ) ;
#8208 = CARTESIAN_POINT ( 'NONE',  ( -20.50609665440969209, 18.01562499999999645, 20.50609665441005092 ) ) ;
#8209 = CARTESIAN_POINT ( 'NONE',  ( 25.98046417659858420, 18.45090250092397355, 15.04653450569292872 ) ) ;
#8210 = CARTESIAN_POINT ( 'NONE',  ( 33.58253175000000113, 6.225000002731185589, -10.91162601494193751 ) ) ;
#8211 = VERTEX_POINT ( 'NONE', #11916 ) ;
#8212 = CARTESIAN_POINT ( 'NONE',  ( -33.58253175000000113, 27.27500000273119340, -10.91162601494193218 ) ) ;
#8213 = CARTESIAN_POINT ( 'NONE',  ( 10.04305231718578817, 39.90000000546237402, -30.90933677959249337 ) ) ;
#8214 = EDGE_CURVE ( 'NONE', #30646, #2692, #32934, .T. ) ;
#8215 = CARTESIAN_POINT ( 'NONE',  ( -26.29305231718578995, 78.19999999999998863, 19.10302069950538595 ) ) ;
#8216 = CARTESIAN_POINT ( 'NONE',  ( -5.147494310547423346, 52.94874572391553613, 32.50000000000000000 ) ) ;
#8217 = CARTESIAN_POINT ( 'NONE',  ( -10.37757302488623701, 39.77500000273118275, 31.93888565452638417 ) ) ;
#8218 = CARTESIAN_POINT ( 'NONE',  ( -32.50000000000000000, 26.00000000000001066, 0.000000000000000000 ) ) ;
#8219 = CARTESIAN_POINT ( 'NONE',  ( -20.08610463437156923, 20.30000000000000071, 27.64615127144130113 ) ) ;
#8220 = CARTESIAN_POINT ( 'NONE',  ( 1.577395562988744260E-15, 2.500000000000008882, -25.76082449383753925 ) ) ;
#8221 = CARTESIAN_POINT ( 'NONE',  ( -10.37757302488624411, 64.72500000273117848, -31.93888565452638417 ) ) ;
#8222 = CARTESIAN_POINT ( 'NONE',  ( -29.99227890624900894, 66.99999999999998579, 14.07346378240356266 ) ) ;
#8223 = CARTESIAN_POINT ( 'NONE',  ( -5.147494310547418017, 76.05125428700922896, -32.50000000000000000 ) ) ;
#8224 = CARTESIAN_POINT ( 'NONE',  ( -2.162160676586882350E-15, 52.87500000273119838, -35.31076352940722529 ) ) ;
#8225 = CARTESIAN_POINT ( 'NONE',  ( 23.41746824999999887, 6.524999997268818852, 7.608796670333735079 ) ) ;
#8226 = CARTESIAN_POINT ( 'NONE',  ( -24.50000000000000000, 8.900000000000011013, -7.960532557706207157 ) ) ;
#8227 = CARTESIAN_POINT ( 'NONE',  ( -20.75514604977248112, 13.42500000273119198, 28.56700777964554661 ) ) ;
#8228 = CARTESIAN_POINT ( 'NONE',  ( -24.18731323226248264, 33.91965250092398065, -14.01125832528284931 ) ) ;
#8229 = CARTESIAN_POINT ( 'NONE',  ( 19.82091636218621034, 9.549999994537621717, 14.40073868116559730 ) ) ;
#8230 = CARTESIAN_POINT ( 'NONE',  ( 3.880418787951139148, 2.198745712990784806, -24.50000000000000000 ) ) ;
#8231 = CARTESIAN_POINT ( 'NONE',  ( 33.58253175000000823, 34.02500000273118275, 10.91162601494192863 ) ) ;
#8232 = CARTESIAN_POINT ( 'NONE',  ( -5.147494310547430452, 18.05125428700922541, -32.49999999999999289 ) ) ;
#8233 = CYLINDRICAL_SURFACE ( 'NONE', #33050, 24.50000000000000000 ) ;
#8234 = CARTESIAN_POINT ( 'NONE',  ( 13.91746824999999887, 79.87500000273118417, -1.704398294459741270E-15 ) ) ;
#8235 = CARTESIAN_POINT ( 'NONE',  ( -20.47846945139866648, 44.07774333240935505, 20.53372385742108008 ) ) ;
#8236 = CARTESIAN_POINT ( 'NONE',  ( -10.04305231718578462, 52.90000000546239534, 30.90933677959249337 ) ) ;
#8237 = CARTESIAN_POINT ( 'NONE',  ( -4.300734207923755825, 73.77500000273118985, 13.23629886949340673 ) ) ;
#8238 = CARTESIAN_POINT ( 'NONE',  ( -8.446640517145639571E-15, 77.00000000546236834, 32.49999999999999289 ) ) ;
#8239 = CARTESIAN_POINT ( 'NONE',  ( -19.09188309203694445, 18.87499999999999645, -19.09188309203661049 ) ) ;
#8240 = CARTESIAN_POINT ( 'NONE',  ( 32.50000000000000711, 71.40000000546241665, 10.55989012756945122 ) ) ;
#8241 = CARTESIAN_POINT ( 'NONE',  ( -15.01150461594642138, 22.45572916666666430, -26.00068869287340334 ) ) ;
#8242 = CARTESIAN_POINT ( 'NONE',  ( -27.16883889988624290, 31.17500000273119909, -19.73931689729374028 ) ) ;
#8243 = CARTESIAN_POINT ( 'NONE',  ( 18.94512977948576093, 13.32499999726879913, -13.76444248337722875 ) ) ;
#8244 = ORIENTED_EDGE ( 'NONE', *, *, #12201, .T. ) ;
#8245 = CARTESIAN_POINT ( 'NONE',  ( -14.97647472619946285, 37.64361083425730925, -26.02091320914851025 ) ) ;
#8246 = CARTESIAN_POINT ( 'NONE',  ( -2.092463501923844636E-15, 14.00000000546237899, -34.17252228774368916 ) ) ;
#8247 = CARTESIAN_POINT ( 'NONE',  ( -7.505752307972844761, 55.54166666666667140, 28.01184896238304134 ) ) ;
#8248 = CARTESIAN_POINT ( 'NONE',  ( 7.505752307973351023, 65.56770833333332860, 28.01184896238290278 ) ) ;
#8249 = CARTESIAN_POINT ( 'NONE',  ( 27.16883889988623935, 50.57500000273118701, -19.73931689729374384 ) ) ;
#8250 = CARTESIAN_POINT ( 'NONE',  ( 20.08610463437157279, 59.80000000546235839, -27.64615127144129758 ) ) ;
#8251 = CARTESIAN_POINT ( 'NONE',  ( 8.601468415847520532, 76.07500000273115859, 11.83890561707634781 ) ) ;
#8252 = CARTESIAN_POINT ( 'NONE',  ( -20.75514604977248823, 38.82500000273120122, -28.56700777964554305 ) ) ;
#8253 = CARTESIAN_POINT ( 'NONE',  ( 2.375766604868046361, 72.80125428700920054, 14.99999999999999822 ) ) ;
#8254 = CARTESIAN_POINT ( 'NONE',  ( -33.58253175000000113, 59.37500000273118417, 0.000000000000000000 ) ) ;
#8255 = PRODUCT_DEFINITION ( 'UNKNOWN', '', #14809, #19552 ) ;
#8256 = CARTESIAN_POINT ( 'NONE',  ( 32.50000000000000000, 1.500000005462381880, -3.980102097228898626E-15 ) ) ;
#8257 = CARTESIAN_POINT ( 'NONE',  ( 33.58253175000000113, 52.22500000273118559, -10.91162601494193574 ) ) ;
#8258 = CARTESIAN_POINT ( 'NONE',  ( 28.01184896238304134, 20.30729166666666430, 7.505752307972846538 ) ) ;
#8259 = CARTESIAN_POINT ( 'NONE',  ( 20.08610463437158344, 42.69999999999998863, 27.64615127144129403 ) ) ;
#8260 = CARTESIAN_POINT ( 'NONE',  ( 18.94512977948575738, 4.424999997268807661, 13.76444248337723408 ) ) ;
#8261 = CARTESIAN_POINT ( 'NONE',  ( 6.486482029760649416E-15, 13.87500000273117529, 35.31076352940723240 ) ) ;
#8262 = CARTESIAN_POINT ( 'NONE',  ( -2.165007332552593587E-13, 51.00000000546238255, 32.50000000000000000 ) ) ;
#8263 = CARTESIAN_POINT ( 'NONE',  ( 8.601468415847520532, 74.07500000273120122, 11.83890561707634781 ) ) ;
#8264 = CARTESIAN_POINT ( 'NONE',  ( -27.16883889988624290, 75.17500000273119554, -19.73931689729374028 ) ) ;
#8265 = CARTESIAN_POINT ( 'NONE',  ( -26.29305231718579350, 21.79999999999998650, -19.10302069950537884 ) ) ;
#8266 = CARTESIAN_POINT ( 'NONE',  ( -10.37757302488623701, 65.77500000273118985, 31.93888565452638417 ) ) ;
#8267 = EDGE_LOOP ( 'NONE', ( #4639, #15658, #7103, #21992 ) ) ;
#8268 = CARTESIAN_POINT ( 'NONE',  ( -14.47279130897151589, 17.82499999726881157, -19.92008829642072598 ) ) ;
#8269 = CARTESIAN_POINT ( 'NONE',  ( -13.97622843553632421, 60.26822916666665009, -24.20753774853731599 ) ) ;
#8270 = CARTESIAN_POINT ( 'NONE',  ( -20.75514604977248823, 52.82500000273116569, -28.56700777964554305 ) ) ;
#8271 = CARTESIAN_POINT ( 'NONE',  ( -33.58253175000000113, 9.475000002731185589, 10.91162601494193929 ) ) ;
#8272 = CARTESIAN_POINT ( 'NONE',  ( 10.37757302488624767, 3.975000002731182924, 31.93888565452638417 ) ) ;
#8273 = CARTESIAN_POINT ( 'NONE',  ( 19.09188309203661049, 43.79687500000000000, -19.09188309203694445 ) ) ;
#8274 = CARTESIAN_POINT ( 'NONE',  ( 28.00173670424549499, 32.05767333425730214, 7.543491769121417612 ) ) ;
#8275 = CARTESIAN_POINT ( 'NONE',  ( -25.98046417659831420, 23.59597249907602290, 15.04653450569339945 ) ) ;
#8276 = CARTESIAN_POINT ( 'NONE',  ( 26.29305231718578995, 73.70000000546238539, -19.10302069950538240 ) ) ;
#8277 = CARTESIAN_POINT ( 'NONE',  ( 33.02351622650643037, 51.99999999999999289, -4.441931073548142983 ) ) ;
#8278 = CARTESIAN_POINT ( 'NONE',  ( 33.58253175000000113, 36.22500000273119980, -10.91162601494193574 ) ) ;
#8279 = CARTESIAN_POINT ( 'NONE',  ( 27.95245687107223276, 42.78868083240935505, -0.04044903255042905932 ) ) ;
#8280 = CARTESIAN_POINT ( 'NONE',  ( 18.94512977948575738, 14.42499999726881654, 13.76444248337723408 ) ) ;
#8281 = DIRECTION ( 'NONE',  ( 0.000000000000000000, -1.000000000000000000, 0.000000000000000000 ) ) ;
#8282 = VERTEX_POINT ( 'NONE', #33361 ) ;
#8283 = CARTESIAN_POINT ( 'NONE',  ( -27.16883889988624290, 49.17500000273118843, -19.73931689729374028 ) ) ;
#8284 = CARTESIAN_POINT ( 'NONE',  ( 4.635254915624212657, 76.59999999999999432, 14.26584774442730286 ) ) ;
#8285 = AXIS2_PLACEMENT_3D ( 'NONE', #5611, #26716, #10930 ) ;
#8286 = CONICAL_SURFACE ( 'NONE', #25293, 10.72870458603808075, 0.8042044335707554392 ) ;
#8287 = CARTESIAN_POINT ( 'NONE',  ( -19.06425588902591173, 51.25038166759065206, -19.11951029504763611 ) ) ;
#8288 = CARTESIAN_POINT ( 'NONE',  ( 33.58253175000000113, 72.47500000273119269, -10.91162601494193751 ) ) ;
#8289 = ORIENTED_EDGE ( 'NONE', *, *, #30841, .T. ) ;
#8290 = CARTESIAN_POINT ( 'NONE',  ( -27.16883889988623935, 17.32500000273119767, 19.73931689729374739 ) ) ;
#8291 = CARTESIAN_POINT ( 'NONE',  ( 20.50609665441005092, 27.46875000000000000, 20.50609665440969209 ) ) ;
#8292 = ORIENTED_EDGE ( 'NONE', *, *, #13074, .T. ) ;
#8293 = CARTESIAN_POINT ( 'NONE',  ( -15.14183272437242067, 2.449999994537622960, -20.84094480462497856 ) ) ;
#8294 = CARTESIAN_POINT ( 'NONE',  ( 27.16883889988624290, 51.92500000273120264, 19.73931689729373673 ) ) ;
#8295 = CARTESIAN_POINT ( 'NONE',  ( 2.740863092043355209E-13, 48.52343750000000000, 30.02300923189239512 ) ) ;
#8296 = CARTESIAN_POINT ( 'NONE',  ( -20.08610463437157989, 18.20000000546239605, -27.64615127144129758 ) ) ;
#8297 = CARTESIAN_POINT ( 'NONE',  ( 10.72870458603808608, -72.44024934668307480, 0.000000000000000000 ) ) ;
#8298 = CARTESIAN_POINT ( 'NONE',  ( 23.41746824999999887, 7.124999997268815832, 0.000000000000000000 ) ) ;
#8299 = CARTESIAN_POINT ( 'NONE',  ( -20.75514604977248112, 31.67500000273119909, 28.56700777964554661 ) ) ;
#8300 = CARTESIAN_POINT ( 'NONE',  ( -10.04305231718578462, 64.40000000000000568, 30.90933677959249337 ) ) ;
#8301 = CARTESIAN_POINT ( 'NONE',  ( -14.97647472619899389, 57.68451416574269075, 26.02091320914878025 ) ) ;
#8302 = DIRECTION ( 'NONE',  ( -1.000000000000000000, 0.000000000000000000, 0.000000000000000000 ) ) ;
#8303 = CARTESIAN_POINT ( 'NONE',  ( -20.08610463437157989, 3.699999999999999289, -27.64615127144129758 ) ) ;
#8304 = ADVANCED_FACE ( 'NONE', ( #5221 ), #22909, .T. ) ;
#8305 = CARTESIAN_POINT ( 'NONE',  ( 20.08610463437158344, 10.69999999999999574, 27.64615127144129403 ) ) ;
#8306 = CARTESIAN_POINT ( 'NONE',  ( 24.20753774853756113, 61.70052083333332860, 13.97622843553589789 ) ) ;
#8307 = CARTESIAN_POINT ( 'NONE',  ( -24.50000000000000000, 18.74999999453763522, -3.000384657911015469E-15 ) ) ;
#8308 = CARTESIAN_POINT ( 'NONE',  ( -11.25946833292375793, 72.67500000273119554, -8.180482586598733619 ) ) ;
#8309 = CARTESIAN_POINT ( 'NONE',  ( 2.584737979205441561E-13, 27.89843750000000000, 27.95245687107222921 ) ) ;
#8310 = CARTESIAN_POINT ( 'NONE',  ( 20.75514604977249178, 23.82500000273118701, 28.56700777964553950 ) ) ;
#8311 = CARTESIAN_POINT ( 'NONE',  ( -20.75514604977248823, 72.82500000273118701, -28.56700777964554305 ) ) ;
#8312 = COLOUR_RGB ( '', 0.66274510, 0.83137255, 0.94901961) ;
#8313 = CARTESIAN_POINT ( 'NONE',  ( 33.58253175000000113, 38.47500000273118559, -10.91162601494193751 ) ) ;
#8314 = CARTESIAN_POINT ( 'NONE',  ( 6.486482029760648627E-15, 15.87500000273120015, 35.31076352940722529 ) ) ;
#8315 = CARTESIAN_POINT ( 'NONE',  ( -19.06425588902591173, 58.12538166759063785, -19.11951029504763611 ) ) ;
#8316 = ADVANCED_FACE ( 'NONE', ( #18370 ), #12678, .T. ) ;
#8317 = CARTESIAN_POINT ( 'NONE',  ( 33.58253175000000113, 68.12500000273119838, -4.112674001490185761E-15 ) ) ;
#8318 = EDGE_CURVE ( 'NONE', #29257, #6224, #20927, .T. ) ;
#8319 = CARTESIAN_POINT ( 'NONE',  ( 26.29305231718579350, 3.300000005462377928, 19.10302069950537529 ) ) ;
#8320 = CARTESIAN_POINT ( 'NONE',  ( 32.50000000000000000, 51.00000000000000711, -3.980102097228898626E-15 ) ) ;
#8321 = DIRECTION ( 'NONE',  ( 0.000000000000000000, 1.000000000000000000, 0.000000000000000000 ) ) ;
#8322 = CARTESIAN_POINT ( 'NONE',  ( -33.58253175000000113, 57.12500000273118417, 0.000000000000000000 ) ) ;
#8323 = CARTESIAN_POINT ( 'NONE',  ( -14.47279130897151589, 17.82499999726881157, -19.92008829642072598 ) ) ;
#8324 = EDGE_CURVE ( 'NONE', #21971, #25648, #20608, .T. ) ;
#8325 = ORIENTED_EDGE ( 'NONE', *, *, #6515, .T. ) ;
#8326 = CARTESIAN_POINT ( 'NONE',  ( 20.75514604977249178, 64.07500000273120122, 28.56700777964553950 ) ) ;
#8327 = CARTESIAN_POINT ( 'NONE',  ( -20.75514604977248112, 3.425000002731186655, 28.56700777964554661 ) ) ;
#8328 = CARTESIAN_POINT ( 'NONE',  ( 23.41746824999999887, 8.624999997268817609, 0.000000000000000000 ) ) ;
#8329 = CARTESIAN_POINT ( 'NONE',  ( 26.09010956794232428, 24.89621500092397710, -6.950374756619718042 ) ) ;
#8330 = ORIENTED_EDGE ( 'NONE', *, *, #21754, .F. ) ;
#8331 = CARTESIAN_POINT ( 'NONE',  ( -10.37757302488623701, 37.52500000273118985, 31.93888565452638417 ) ) ;
#8332 = CARTESIAN_POINT ( 'NONE',  ( -20.08610463437157989, 68.20000000546239960, -27.64615127144129758 ) ) ;
#8333 = ORIENTED_EDGE ( 'NONE', *, *, #14071, .T. ) ;
#8334 = CARTESIAN_POINT ( 'NONE',  ( 28.01184896238304134, 54.68229166666665719, 7.505752307972846538 ) ) ;
#8335 = CARTESIAN_POINT ( 'NONE',  ( 26.29305231718579350, 4.799999999999998934, 19.10302069950537529 ) ) ;
#8336 = CARTESIAN_POINT ( 'NONE',  ( -1.778240108872766143E-15, 59.50000000000000711, -32.49999999999999289 ) ) ;
#8337 = LINE ( 'NONE', #26540, #3049 ) ;
#8338 = CARTESIAN_POINT ( 'NONE',  ( -20.50609665440969209, 18.01562499999999645, 20.50609665441005092 ) ) ;
#8339 = CARTESIAN_POINT ( 'NONE',  ( -24.50000000000000355, 2.899999999999995470, -7.960532557706207157 ) ) ;
#8340 = CARTESIAN_POINT ( 'NONE',  ( -33.58253175000000113, 7.475000002731175819, 10.91162601494193929 ) ) ;
#8341 = CARTESIAN_POINT ( 'NONE',  ( -20.08610463437157989, 59.70000000000000284, -27.64615127144129758 ) ) ;
#8342 = CARTESIAN_POINT ( 'NONE',  ( 32.50000000000000000, 57.60000000546236976, -10.55989012756945833 ) ) ;
#8343 = CARTESIAN_POINT ( 'NONE',  ( 3.245314017740486554E-15, 0.000000000000000000, -26.50000000000000355 ) ) ;
#8344 = CARTESIAN_POINT ( 'NONE',  ( -7.468012846824272799, 33.47878499907601935, 28.02196122052058413 ) ) ;
#8345 = CARTESIAN_POINT ( 'NONE',  ( 13.91746825000000065, 74.27500000273117564, 4.522059556121114987 ) ) ;
#8346 = CARTESIAN_POINT ( 'NONE',  ( -7.505752307973343918, 46.66145833333332860, -28.01184896238290989 ) ) ;
#8347 = FACE_OUTER_BOUND ( 'NONE', #14708, .T. ) ;
#8348 = CARTESIAN_POINT ( 'NONE',  ( -32.50000000000000000, 38.40000000546235981, -10.55989012756945300 ) ) ;
#8349 = CARTESIAN_POINT ( 'NONE',  ( 14.01125832528330051, 60.54909749907603356, 24.18731323226221974 ) ) ;
#8350 = CARTESIAN_POINT ( 'NONE',  ( 33.58253175000000823, 46.02500000273118275, 10.91162601494192863 ) ) ;
#8351 = AXIS2_PLACEMENT_3D ( 'NONE', #25074, #4483, #6552 ) ;
#8352 = CARTESIAN_POINT ( 'NONE',  ( 13.91746824999999532, 79.97500000273115006, -4.522059556121118540 ) ) ;
#8353 = CARTESIAN_POINT ( 'NONE',  ( 33.58253175000000113, 54.47500000273117138, -10.91162601494193751 ) ) ;
#8354 = CARTESIAN_POINT ( 'NONE',  ( -20.75514604977248823, 35.07500000273120833, -28.56700777964554305 ) ) ;
#8355 = DIRECTION ( 'NONE',  ( 0.000000000000000000, -1.000000000000000000, 0.000000000000000000 ) ) ;
#8356 = AXIS2_PLACEMENT_3D ( 'NONE', #5535, #10182, #21332 ) ;
#8357 = CARTESIAN_POINT ( 'NONE',  ( -13.97622843553632777, 19.01822916666666430, -24.20753774853731599 ) ) ;
#8358 = CARTESIAN_POINT ( 'NONE',  ( 4.222871413987100692E-15, -57.48236190979495319, 0.000000000000000000 ) ) ;
#8359 = CARTESIAN_POINT ( 'NONE',  ( 32.50000000000000000, 31.10000000000000497, -10.55989012756945833 ) ) ;
#8360 = CARTESIAN_POINT ( 'NONE',  ( 32.50000000000000711, 72.90000000000000568, 10.55989012756945122 ) ) ;
#8361 = CARTESIAN_POINT ( 'NONE',  ( -33.58253175000000113, 7.225000002731182924, 10.91162601494193929 ) ) ;
#8362 = CARTESIAN_POINT ( 'NONE',  ( 14.47279130897151944, 2.924999997268816099, -19.92008829642072598 ) ) ;
#8363 = CARTESIAN_POINT ( 'NONE',  ( -7.570916362186215665, 11.14999999453761248, 23.30088464923126423 ) ) ;
#8364 = CARTESIAN_POINT ( 'NONE',  ( -24.18731323226221974, 30.47097249907602290, 14.01125832528330406 ) ) ;
#8365 = ADVANCED_FACE ( 'NONE', ( #12044 ), #15794, .T. ) ;
#8366 =( BOUNDED_CURVE ( )  B_SPLINE_CURVE ( 2, ( #22177, #19600, #32950, #27485, #3975, #14447, #4309, #9280, #19764, #14785, #17363, #22501, #27827 ),
 .UNSPECIFIED., .F., .T. ) 
 B_SPLINE_CURVE_WITH_KNOTS ( ( 3, 2, 2, 2, 2, 2, 3 ),
 ( 0.3269230769230769273, 0.3282051282051282048, 0.3307692307692307598, 0.3333333333333333148, 0.3358974358974358698, 0.3384615384615384803, 0.3397435897435897578 ),
 .UNSPECIFIED. ) 
 CURVE ( )  GEOMETRIC_REPRESENTATION_ITEM ( )  RATIONAL_B_SPLINE_CURVE ( ( 0.9755282581475768211, 0.9755282581475768211, 1.000000000000000000, 0.9510565162951535312, 1.000000000000000000, 0.9510565162951535312, 1.000000000000000000, 0.9510565162951535312, 1.000000000000000000, 0.9510565162951535312, 1.000000000000000000, 0.9755282581475768211, 0.9755282581475768211 ) ) 
 REPRESENTATION_ITEM ( '' )  );
#8367 = CARTESIAN_POINT ( 'NONE',  ( -10.04305231718578462, 60.40000000000000568, 30.90933677959249337 ) ) ;
#8368 = CARTESIAN_POINT ( 'NONE',  ( -27.16883889988623935, 19.32500000273118701, 19.73931689729374739 ) ) ;
#8369 = CARTESIAN_POINT ( 'NONE',  ( -24.20753774853756823, 53.10677083333331439, -13.97622843553588723 ) ) ;
#8370 = ORIENTED_EDGE ( 'NONE', *, *, #14830, .T. ) ;
#8371 = CARTESIAN_POINT ( 'NONE',  ( 27.16883889988623935, 64.32500000273121543, -19.73931689729374384 ) ) ;
#8372 = ORIENTED_EDGE ( 'NONE', *, *, #11319, .F. ) ;
#8373 = CARTESIAN_POINT ( 'NONE',  ( 2.740863092043355209E-13, 17.58593749999999645, 30.02300923189239512 ) ) ;
#8374 = CARTESIAN_POINT ( 'NONE',  ( 30.02300923189239867, 11.28944416759064140, 0.04044903254992252006 ) ) ;
#8375 = AXIS2_PLACEMENT_3D ( 'NONE', #2754, #9970, #13219 ) ;
#8376 = CARTESIAN_POINT ( 'NONE',  ( -27.16883889988623935, 3.325000002731184789, 19.73931689729374739 ) ) ;
#8377 = VECTOR ( 'NONE', #1999, 1000.000000000000000 ) ;
#8378 = ORIENTED_EDGE ( 'NONE', *, *, #29484, .T. ) ;
#8379 = FACE_OUTER_BOUND ( 'NONE', #24261, .T. ) ;
#8380 = CARTESIAN_POINT ( 'NONE',  ( -33.58253175000000113, 25.27500000273119696, -10.91162601494193218 ) ) ;
#8381 = CARTESIAN_POINT ( 'NONE',  ( 26.29305231718579350, 29.30000000546237260, 19.10302069950537529 ) ) ;
#8382 = CARTESIAN_POINT ( 'NONE',  ( 15.00000000000000000, 73.00000000000001421, -1.836970198721029589E-15 ) ) ;
#8383 = CARTESIAN_POINT ( 'NONE',  ( 10.04305231718579705, 52.60000000000000853, 30.90933677959248982 ) ) ;
#8384 = CARTESIAN_POINT ( 'NONE',  ( -15.14183272437242067, 10.70000000000001172, -20.84094480462497856 ) ) ;
#8385 = CARTESIAN_POINT ( 'NONE',  ( 6.486482029760649416E-15, 41.87500000273119127, 35.31076352940723240 ) ) ;
#8386 = CARTESIAN_POINT ( 'NONE',  ( 26.29305231718578995, 23.19999999999998508, -19.10302069950538240 ) ) ;
#8387 = CARTESIAN_POINT ( 'NONE',  ( 26.29305231718579350, 20.79999999999998650, 19.10302069950537529 ) ) ;
#8388 = CARTESIAN_POINT ( 'NONE',  ( 7.570916362186207671, 5.599999999999994316, 23.30088464923126779 ) ) ;
#8389 = CARTESIAN_POINT ( 'NONE',  ( 10.37757302488624767, 65.72500000273117848, 31.93888565452638417 ) ) ;
#8390 = CARTESIAN_POINT ( 'NONE',  ( -31.08180318173140577, 66.99999999999998579, 11.59917702625715030 ) ) ;
#8391 = CARTESIAN_POINT ( 'NONE',  ( -1.525229598305639200, 73.99999999999998579, -14.55759990445270269 ) ) ;
#8392 = CARTESIAN_POINT ( 'NONE',  ( -27.16883889988624290, 55.17500000273118133, -19.73931689729374028 ) ) ;
#8393 = CARTESIAN_POINT ( 'NONE',  ( 7.236395654485755280, 6.224999997268803931, 22.27133577429736988 ) ) ;
#8394 = CARTESIAN_POINT ( 'NONE',  ( 20.75514604977249178, 7.825000002731194115, 28.56700777964553950 ) ) ;
#8395 = CARTESIAN_POINT ( 'NONE',  ( -19.06425588902591173, 40.93788166759063785, -19.11951029504763611 ) ) ;
#8396 = CARTESIAN_POINT ( 'NONE',  ( 17.62835169016977233, 16.99999999999998579, -15.43382168286624179 ) ) ;
#8397 = CARTESIAN_POINT ( 'NONE',  ( -29.12397828776023800, 52.00000000000000000, 15.02363756889442570 ) ) ;
#8398 = CARTESIAN_POINT ( 'NONE',  ( -10.37757302488623701, 27.52500000273118275, 31.93888565452638417 ) ) ;
#8399 = CARTESIAN_POINT ( 'NONE',  ( 26.29305231718579350, 64.80000000000001137, 19.10302069950537529 ) ) ;
#8400 = DIRECTION ( 'NONE',  ( -0.000000000000000000, -1.000000000000000000, -0.000000000000000000 ) ) ;
#8401 = CIRCLE ( 'NONE', #728, 15.00000000000000000 ) ;
#8402 = CARTESIAN_POINT ( 'NONE',  ( 11.25946833292375793, 76.07500000273120122, -8.180482586598735395 ) ) ;
#8403 = CARTESIAN_POINT ( 'NONE',  ( -20.47846945139866648, 57.82774333240935505, 20.53372385742108008 ) ) ;
#8404 = CARTESIAN_POINT ( 'NONE',  ( -32.50000000000000000, 52.50000000546238255, 0.000000000000000000 ) ) ;
#8405 = CARTESIAN_POINT ( 'NONE',  ( -1.778240108872766143E-15, 49.50000000000000000, -32.49999999999999289 ) ) ;
#8406 = SURFACE_STYLE_USAGE ( .BOTH. , #22136 ) ;
#8407 = CARTESIAN_POINT ( 'NONE',  ( -19.09188309203660694, 14.57812499999999645, 19.09188309203694800 ) ) ;
#8408 = EDGE_CURVE ( 'NONE', #30686, #17243, #26222, .T. ) ;
#8409 = CARTESIAN_POINT ( 'NONE',  ( 20.08610463437157279, 69.80000000546240813, -27.64615127144129758 ) ) ;
#8410 = CARTESIAN_POINT ( 'NONE',  ( -20.50609665440969209, 28.32812499999999645, 20.50609665441005092 ) ) ;
#8411 = CARTESIAN_POINT ( 'NONE',  ( -7.236395654485763274, 12.52499999726880375, 22.27133577429736633 ) ) ;
#8412 = ORIENTED_EDGE ( 'NONE', *, *, #19074, .T. ) ;
#8413 = CARTESIAN_POINT ( 'NONE',  ( -20.53372385742071771, 40.07850666759064495, 20.47846945139902530 ) ) ;
#8414 = CARTESIAN_POINT ( 'NONE',  ( 32.50000000000000711, 17.40000000546238823, 10.55989012756945122 ) ) ;
#8415 = CARTESIAN_POINT ( 'NONE',  ( -26.00068869287340334, 55.97135416666665719, 15.01150461594643382 ) ) ;
#8416 = LINE ( 'NONE', #6015, #31105 ) ;
#8417 = CARTESIAN_POINT ( 'NONE',  ( 10.37757302488624767, 45.97500000273119269, 31.93888565452638417 ) ) ;
#8418 = CARTESIAN_POINT ( 'NONE',  ( 26.29305231718578995, 55.70000000546237828, -19.10302069950538240 ) ) ;
#8419 = LINE ( 'NONE', #13419, #28666 ) ;
#8420 = CARTESIAN_POINT ( 'NONE',  ( 20.75514604977248467, 34.42500000273117422, -28.56700777964554305 ) ) ;
#8421 = CARTESIAN_POINT ( 'NONE',  ( 7.313012447739250820E-14, 11.49999999999999112, 24.50000000000000000 ) ) ;
#8422 = CARTESIAN_POINT ( 'NONE',  ( -27.16883889988624290, 63.17500000273118843, -19.73931689729374028 ) ) ;
#8423 = CARTESIAN_POINT ( 'NONE',  ( -20.08610463437156923, 0.8000000054623617185, 27.64615127144130113 ) ) ;
#8424 = CIRCLE ( 'NONE', #12821, 30.00000000000004974 ) ;
#8425 = CARTESIAN_POINT ( 'NONE',  ( 20.75514604977248467, 54.42500000273117422, -28.56700777964554305 ) ) ;
#8426 = CARTESIAN_POINT ( 'NONE',  ( -20.50609665440969209, 18.01562499999999645, 20.50609665441005092 ) ) ;
#8427 = CARTESIAN_POINT ( 'NONE',  ( -2.092463501923844636E-15, 39.50000000000000000, -34.17252228774368916 ) ) ;
#8428 = CARTESIAN_POINT ( 'NONE',  ( -14.47279130897151589, 3.324999997268803131, -19.92008829642072598 ) ) ;
#8429 = CARTESIAN_POINT ( 'NONE',  ( -10.37757302488624411, 2.975000002731182036, -31.93888565452638417 ) ) ;
#8430 = CARTESIAN_POINT ( 'NONE',  ( 19.82091636218621034, 19.54999999453763238, 14.40073868116559730 ) ) ;
#8431 = CARTESIAN_POINT ( 'NONE',  ( -11.25946833292375793, 75.17500000273119554, -8.180482586598733619 ) ) ;
#8432 = CARTESIAN_POINT ( 'NONE',  ( 20.75514604977248467, 70.67500000273119554, -28.56700777964554305 ) ) ;
#8433 = CYLINDRICAL_SURFACE ( 'NONE', #6711, 32.50000000000000000 ) ;
#8434 = CARTESIAN_POINT ( 'NONE',  ( -33.58253175000000113, 65.37500000273121259, 0.000000000000000000 ) ) ;
#8435 = VERTEX_POINT ( 'NONE', #17379 ) ;
#8436 = CARTESIAN_POINT ( 'NONE',  ( 0.000000000000000000, 80.00000000000001421, 0.000000000000000000 ) ) ;
#8437 = CARTESIAN_POINT ( 'NONE',  ( 26.07999730980477437, 61.27083333333332860, -6.988114217768290004 ) ) ;
#8438 = CARTESIAN_POINT ( 'NONE',  ( -8.891200544363830713E-16, 75.50000000000001421, -15.00000000000000000 ) ) ;
#8439 = CARTESIAN_POINT ( 'NONE',  ( 20.75514604977249178, 55.82500000273119412, 28.56700777964553950 ) ) ;
#8440 = CARTESIAN_POINT ( 'NONE',  ( -33.58253175000000113, 11.37500000273118594, 0.000000000000000000 ) ) ;
#8441 = CARTESIAN_POINT ( 'NONE',  ( 33.58253175000000113, 64.37500000273121259, -4.112674001490185761E-15 ) ) ;
#8442 = CARTESIAN_POINT ( 'NONE',  ( -19.09188309203660694, 52.39062499999999289, 19.09188309203694800 ) ) ;
#8443 = CARTESIAN_POINT ( 'NONE',  ( -26.02091320914849959, 33.34673583425730214, 14.97647472619947528 ) ) ;
#8444 = CARTESIAN_POINT ( 'NONE',  ( -7.468012846824272799, 23.16628499907601579, 28.02196122052058413 ) ) ;
#8445 = CARTESIAN_POINT ( 'NONE',  ( 20.08610463437157279, 75.80000000546237970, -27.64615127144129758 ) ) ;
#8446 = CARTESIAN_POINT ( 'NONE',  ( 11.25946833292375793, 80.07500000273121543, -8.180482586598735395 ) ) ;
#8447 = VECTOR ( 'NONE', #23654, 1000.000000000000114 ) ;
#8448 = CARTESIAN_POINT ( 'NONE',  ( -10.37757302488623701, 39.52500000273118275, 31.93888565452638417 ) ) ;
#8449 = CARTESIAN_POINT ( 'NONE',  ( 14.01125832528330051, 50.23659749907603356, 24.18731323226221974 ) ) ;
#8450 = CARTESIAN_POINT ( 'NONE',  ( 1.507698388325705758E-15, 17.12499999726880517, -24.62258325217400312 ) ) ;
#8451 = EDGE_CURVE ( 'NONE', #14454, #7660, #31021, .T. ) ;
#8452 = CARTESIAN_POINT ( 'NONE',  ( 24.50000000000000000, 13.89999999999999680, 7.960532557706212486 ) ) ;
#8453 = EDGE_CURVE ( 'NONE', #15743, #31472, #11048, .T. ) ;
#8454 = ORIENTED_EDGE ( 'NONE', *, *, #18889, .T. ) ;
#8455 = CARTESIAN_POINT ( 'NONE',  ( 20.75514604977249178, 50.07500000273120122, 28.56700777964553950 ) ) ;
#8456 = CARTESIAN_POINT ( 'NONE',  ( -20.08610463437157989, 50.20000000546237118, -27.64615127144129758 ) ) ;
#8457 = CARTESIAN_POINT ( 'NONE',  ( 7.025853678916403666, 55.26079833425730214, -26.06988505166735237 ) ) ;
#8458 = CARTESIAN_POINT ( 'NONE',  ( -2.162160676586881955E-15, 68.87500000273118417, -35.31076352940723240 ) ) ;
#8459 = ORIENTED_EDGE ( 'NONE', *, *, #12464, .T. ) ;
#8460 = CARTESIAN_POINT ( 'NONE',  ( 33.58253175000000113, 20.12500000273119483, -4.112674001490185761E-15 ) ) ;
#8461 = CARTESIAN_POINT ( 'NONE',  ( -28.01184896238290278, 21.73958333333332860, 7.505752307973363457 ) ) ;
#8462 = ORIENTED_EDGE ( 'NONE', *, *, #10902, .T. ) ;
#8463 = CARTESIAN_POINT ( 'NONE',  ( -3.880418787951138260, 3.198745712990784806, 24.50000000000000000 ) ) ;
#8464 = CARTESIAN_POINT ( 'NONE',  ( -33.58253175000000113, 57.12500000273118417, 0.000000000000000000 ) ) ;
#8465 = CARTESIAN_POINT ( 'NONE',  ( -26.00068869287340334, 49.09635416666665719, 15.01150461594643382 ) ) ;
#8466 =( BOUNDED_CURVE ( )  B_SPLINE_CURVE ( 2, ( #1671, #22619, #17145, #33072, #11980, #9578, #2024, #7342, #22448, #15077, #7001, #1845, #14396 ),
 .UNSPECIFIED., .F., .T. ) 
 B_SPLINE_CURVE_WITH_KNOTS ( ( 3, 2, 2, 2, 2, 2, 3 ),
 ( 0.3782051282051281937, 0.3794871794871794712, 0.3820512820512820262, 0.3846153846153846367, 0.3871794871794871917, 0.3897435897435897467, 0.3910256410256410242 ),
 .UNSPECIFIED. ) 
 CURVE ( )  GEOMETRIC_REPRESENTATION_ITEM ( )  RATIONAL_B_SPLINE_CURVE ( ( 0.9755282581475768211, 0.9755282581475768211, 1.000000000000000000, 0.9510565162951535312, 1.000000000000000000, 0.9510565162951535312, 1.000000000000000000, 0.9510565162951535312, 1.000000000000000000, 0.9510565162951535312, 1.000000000000000000, 0.9755282581475768211, 0.9755282581475768211 ) ) 
 REPRESENTATION_ITEM ( '' )  );
#8467 = CARTESIAN_POINT ( 'NONE',  ( -26.29305231718578995, 20.70000000546237828, 19.10302069950538595 ) ) ;
#8468 = FACE_OUTER_BOUND ( 'NONE', #9635, .T. ) ;
#8469 = CARTESIAN_POINT ( 'NONE',  ( -7.236395654485763274, 8.524999997268800200, 22.27133577429736633 ) ) ;
#8470 = COLOUR_RGB ( '', 0.09019608, 0.27058824, 0.51372549) ;
#8471 = EDGE_CURVE ( 'NONE', #24301, #9005, #3575, .T. ) ;
#8472 =( BOUNDED_CURVE ( )  B_SPLINE_CURVE ( 2, ( #3003, #18293, #21202, #18795, #18460, #5405, #13298, #26510, #20864, #29239, #13126, #8144, #31310 ),
 .UNSPECIFIED., .F., .T. ) 
 B_SPLINE_CURVE_WITH_KNOTS ( ( 3, 2, 2, 2, 2, 2, 3 ),
 ( 0.2500000000000000000, 0.2512820512820512775, 0.2538461538461538325, 0.2564102564102563875, 0.2589743589743589980, 0.2615384615384615530, 0.2628205128205128305 ),
 .UNSPECIFIED. ) 
 CURVE ( )  GEOMETRIC_REPRESENTATION_ITEM ( )  RATIONAL_B_SPLINE_CURVE ( ( 0.9755282581475768211, 0.9755282581475768211, 1.000000000000000000, 0.9510565162951535312, 1.000000000000000000, 0.9510565162951535312, 1.000000000000000000, 0.9510565162951535312, 1.000000000000000000, 0.9510565162951535312, 1.000000000000000000, 0.9755282581475768211, 0.9755282581475768211 ) ) 
 REPRESENTATION_ITEM ( '' )  );
#8473 = CARTESIAN_POINT ( 'NONE',  ( 20.75514604977248467, 24.67500000273118843, -28.56700777964554305 ) ) ;
#8474 = CARTESIAN_POINT ( 'NONE',  ( -19.06425588902558133, 20.01524333240935505, 19.11951029504797006 ) ) ;
#8475 = CARTESIAN_POINT ( 'NONE',  ( 8.601468415847520532, 79.57500000273120122, 11.83890561707634781 ) ) ;
#8476 = CARTESIAN_POINT ( 'NONE',  ( -10.04305231718578462, 28.90000000546238823, 30.90933677959249337 ) ) ;
#8477 = CARTESIAN_POINT ( 'NONE',  ( 32.50000000000000000, 10.99999999999999645, -3.980102097228898626E-15 ) ) ;
#8478 = ORIENTED_EDGE ( 'NONE', *, *, #9780, .T. ) ;
#8479 = CARTESIAN_POINT ( 'NONE',  ( 14.47279130897151767, 1.424999997268804997, -19.92008829642072598 ) ) ;
#8480 = CARTESIAN_POINT ( 'NONE',  ( -4.300734207923755825, 75.27500000273118985, 13.23629886949340673 ) ) ;
#8481 = CARTESIAN_POINT ( 'NONE',  ( -24.20753774853756823, 32.48177083333332860, -13.97622843553588723 ) ) ;
#8482 = CARTESIAN_POINT ( 'NONE',  ( -20.75514604977248112, 27.42500000273118488, 28.56700777964554661 ) ) ;
#8483 = CARTESIAN_POINT ( 'NONE',  ( -10.37757302488623701, 75.52500000273120406, 31.93888565452638417 ) ) ;
#8484 = CARTESIAN_POINT ( 'NONE',  ( -10.37757302488624411, 28.97500000273119269, -31.93888565452638417 ) ) ;
#8485 = CARTESIAN_POINT ( 'NONE',  ( 10.37757302488624767, 15.97500000273119269, 31.93888565452638417 ) ) ;
#8486 = CARTESIAN_POINT ( 'NONE',  ( -24.22776226481240514, 53.97173583425732346, 13.94119854578937812 ) ) ;
#8487 = CARTESIAN_POINT ( 'NONE',  ( -33.58253175000000113, 69.22500000273116427, 10.91162601494193929 ) ) ;
#8488 = CARTESIAN_POINT ( 'NONE',  ( 0.000000000000000000, 74.00000000000001421, 15.00000000000000000 ) ) ;
#8489 = CARTESIAN_POINT ( 'NONE',  ( -4.300734207923759378, 78.97500000273119269, -13.23629886949340495 ) ) ;
#8490 = CARTESIAN_POINT ( 'NONE',  ( -32.50000000000000000, 54.00000000000000711, 0.000000000000000000 ) ) ;
#8491 = CARTESIAN_POINT ( 'NONE',  ( 23.09401076758502569, 96.00000000000002842, -6.857326241137392698E-15 ) ) ;
#8492 = CARTESIAN_POINT ( 'NONE',  ( -33.58253175000000113, 59.12500000273118417, 0.000000000000000000 ) ) ;
#8493 = CARTESIAN_POINT ( 'NONE',  ( 7.236395654485755280, 14.72499999726881192, 22.27133577429736988 ) ) ;
#8494 = ORIENTED_EDGE ( 'NONE', *, *, #10556, .T. ) ;
#8495 = CARTESIAN_POINT ( 'NONE',  ( 20.75514604977248467, 64.67500000273118133, -28.56700777964554305 ) ) ;
#8496 = CARTESIAN_POINT ( 'NONE',  ( -26.29305231718579350, 61.80000000000000426, -19.10302069950537884 ) ) ;
#8497 = CARTESIAN_POINT ( 'NONE',  ( -7.236395654485763274, 4.024999997268824181, 22.27133577429736633 ) ) ;
#8498 = CARTESIAN_POINT ( 'NONE',  ( 14.01125832528286352, 27.90402750092397355, -24.18731323226246843 ) ) ;
#8499 = ORIENTED_EDGE ( 'NONE', *, *, #3387, .T. ) ;
#8500 = CARTESIAN_POINT ( 'NONE',  ( 10.37757302488624767, 39.72500000273119980, 31.93888565452638417 ) ) ;
#8501 = PLANE ( 'NONE',  #21463 ) ;
#8502 = ORIENTED_EDGE ( 'NONE', *, *, #9354, .T. ) ;
#8503 = CARTESIAN_POINT ( 'NONE',  ( -7.505752307973343918, 50.09895833333332860, -28.01184896238290989 ) ) ;
#8504 = CARTESIAN_POINT ( 'NONE',  ( 1.093617666956751375E-13, 60.00000000546238255, -32.50000000000000711 ) ) ;
#8505 = CARTESIAN_POINT ( 'NONE',  ( -4.223320258572819786E-15, 3.500000000000004441, 24.50000000000000000 ) ) ;
#8506 = CARTESIAN_POINT ( 'NONE',  ( 10.37757302488624767, 71.72500000273119269, 31.93888565452638417 ) ) ;
#8507 = CARTESIAN_POINT ( 'NONE',  ( -28.01184896238290278, 25.17708333333332860, 7.505752307973363457 ) ) ;
#8508 = EDGE_CURVE ( 'NONE', #2126, #33755, #9935, .T. ) ;
#8509 = CARTESIAN_POINT ( 'NONE',  ( -15.14183272437241889, 8.699999999999986855, -20.84094480462497856 ) ) ;
#8510 = CARTESIAN_POINT ( 'NONE',  ( 20.75514604977249178, 10.07500000273118168, 28.56700777964553950 ) ) ;
#8511 = CARTESIAN_POINT ( 'NONE',  ( -20.75514604977248112, 15.42500000273118843, 28.56700777964554661 ) ) ;
#8512 = VECTOR ( 'NONE', #33159, 1000.000000000000000 ) ;
#8513 = CARTESIAN_POINT ( 'NONE',  ( 8.601468415847516980, 80.17500000273116711, -11.83890561707634603 ) ) ;
#8514 = LINE ( 'NONE', #11103, #21461 ) ;
#8515 = CARTESIAN_POINT ( 'NONE',  ( -20.53372385742107653, 38.06211833240934084, -20.47846945139867003 ) ) ;
#8516 = CARTESIAN_POINT ( 'NONE',  ( 4.300734207923761154, 75.97500000273119269, 13.23629886949340495 ) ) ;
#8517 = CARTESIAN_POINT ( 'NONE',  ( 28.01184896238290278, 47.52083333333332860, -7.505752307973347470 ) ) ;
#8518 = EDGE_CURVE ( 'NONE', #20335, #31666, #18538, .T. ) ;
#8519 = CARTESIAN_POINT ( 'NONE',  ( -24.50000000000000000, 8.749999994537628112, -3.000384657911015469E-15 ) ) ;
#8520 = VECTOR ( 'NONE', #15225, 1000.000000000000000 ) ;
#8521 = CARTESIAN_POINT ( 'NONE',  ( 26.29305231718578995, 49.70000000546237118, -19.10302069950538240 ) ) ;
#8522 = CARTESIAN_POINT ( 'NONE',  ( 19.06425588902558133, 59.54649333240936215, -19.11951029504797006 ) ) ;
#8523 = CARTESIAN_POINT ( 'NONE',  ( -10.37757302488623701, 45.52500000273118985, 31.93888565452638417 ) ) ;
#8524 = CARTESIAN_POINT ( 'NONE',  ( 12.13525491562421088, 71.05000000546240813, 8.816778784387095058 ) ) ;
#8525 = CARTESIAN_POINT ( 'NONE',  ( -33.58253175000000113, 47.37500000273119127, 0.000000000000000000 ) ) ;
#8526 = CARTESIAN_POINT ( 'NONE',  ( 33.58253175000000823, 36.27500000273119696, 10.91162601494192685 ) ) ;
#8527 = CARTESIAN_POINT ( 'NONE',  ( -5.260389231090357498, 16.99999999999999289, 23.61507992718642868 ) ) ;
#8528 = CARTESIAN_POINT ( 'NONE',  ( 6.988114217768294445, 20.88020833333333215, 26.07999730980477437 ) ) ;
#8529 = CARTESIAN_POINT ( 'NONE',  ( 15.14183272437242422, 12.04999999453761106, -20.84094480462497856 ) ) ;
#8530 = CARTESIAN_POINT ( 'NONE',  ( -20.08610463437157989, 44.20000000546238539, -27.64615127144129758 ) ) ;
#8531 = CARTESIAN_POINT ( 'NONE',  ( -32.50000000000000000, 71.89999999999999147, -10.55989012756945478 ) ) ;
#8532 = VECTOR ( 'NONE', #21161, 1000.000000000000000 ) ;
#8533 = CARTESIAN_POINT ( 'NONE',  ( 33.58253175000000823, 10.02500000273118275, 10.91162601494192863 ) ) ;
#8534 = CARTESIAN_POINT ( 'NONE',  ( 23.41746824999999887, 2.724999997268822138, -7.608796670333727974 ) ) ;
#8535 = VECTOR ( 'NONE', #11078, 1000.000000000000000 ) ;
#8536 = CARTESIAN_POINT ( 'NONE',  ( -5.147494310547423346, 52.94874572391552903, 32.50000000000000000 ) ) ;
#8537 = CARTESIAN_POINT ( 'NONE',  ( -6.950374756619247307, 26.60378499907601579, 26.09010956794245217 ) ) ;
#8538 = CARTESIAN_POINT ( 'NONE',  ( -5.147494310547430452, 59.55125428154684641, -32.49999999999999289 ) ) ;
#8539 = PRODUCT_DEFINITION_SHAPE ( 'NONE', 'NONE',  #12245 ) ;
#8540 = CARTESIAN_POINT ( 'NONE',  ( 33.58253175000000823, 20.02500000273118275, 10.91162601494192685 ) ) ;
#8541 = CARTESIAN_POINT ( 'NONE',  ( -24.20753774853730889, 49.09635416666665719, 13.97622843553633842 ) ) ;
#8542 = VERTEX_POINT ( 'NONE', #5819 ) ;
#8543 = CARTESIAN_POINT ( 'NONE',  ( -2.162160676586881955E-15, 54.62500000273116996, -35.31076352940723240 ) ) ;
#8544 = VERTEX_POINT ( 'NONE', #29638 ) ;
#8545 = CARTESIAN_POINT ( 'NONE',  ( -20.50609665440969209, 28.32812499999999645, 20.50609665441005092 ) ) ;
#8546 = CARTESIAN_POINT ( 'NONE',  ( 28.02196122052045268, 21.45871500092397355, -7.468012846824774620 ) ) ;
#8547 = LINE ( 'NONE', #16454, #23332 ) ;
#8548 =( REPRESENTATION_RELATIONSHIP ('NONE','NONE', #5873, #22108 ) REPRESENTATION_RELATIONSHIP_WITH_TRANSFORMATION ( #31688 )SHAPE_REPRESENTATION_RELATIONSHIP( ) );
#8549 = ORIENTED_EDGE ( 'NONE', *, *, #1168, .T. ) ;
#8550 = CARTESIAN_POINT ( 'NONE',  ( -7.236395654485763274, 2.024999997268822405, 22.27133577429736633 ) ) ;
#8551 = CARTESIAN_POINT ( 'NONE',  ( 33.58253175000000113, 30.37500000273119127, -4.112674001490185761E-15 ) ) ;
#8552 = CARTESIAN_POINT ( 'NONE',  ( -10.04305231718578462, 28.90000000546238823, 30.90933677959249337 ) ) ;
#8553 = AXIS2_PLACEMENT_3D ( 'NONE', #10350, #20828, #4851 ) ;
#8554 = CARTESIAN_POINT ( 'NONE',  ( 26.29305231718579350, 76.80000000000001137, 19.10302069950537529 ) ) ;
#8555 = CARTESIAN_POINT ( 'NONE',  ( -10.04305231718579172, 54.10000000546239107, -30.90933677959248982 ) ) ;
#8556 = CARTESIAN_POINT ( 'NONE',  ( 26.29305231718578995, 37.70000000546236407, -19.10302069950538240 ) ) ;
#8557 = CARTESIAN_POINT ( 'NONE',  ( -27.16883889988623935, 41.57500000273117990, 19.73931689729374739 ) ) ;
#8558 =( LENGTH_UNIT ( ) NAMED_UNIT ( * ) SI_UNIT ( .MILLI., .METRE. ) );
#8559 = CARTESIAN_POINT ( 'NONE',  ( -32.50000000000000000, 26.09999999999999076, 10.55989012756946366 ) ) ;
#8560 = CARTESIAN_POINT ( 'NONE',  ( -26.29305231718578995, 22.19999999999999574, 19.10302069950538595 ) ) ;
#8561 = CARTESIAN_POINT ( 'NONE',  ( 19.82091636218621034, 11.80000000000000426, 14.40073868116559730 ) ) ;
#8562 = CARTESIAN_POINT ( 'NONE',  ( -33.58253175000000113, 65.22500000273117848, 10.91162601494193929 ) ) ;
#8563 = CARTESIAN_POINT ( 'NONE',  ( -33.58253175000000113, 51.37500000273120548, 0.000000000000000000 ) ) ;
#8564 = CARTESIAN_POINT ( 'NONE',  ( -4.523095164977117273E-15, 12.12499999726881583, 24.62258325217400312 ) ) ;
#8565 = DIRECTION ( 'NONE',  ( -0.000000000000000000, -1.000000000000000000, -0.000000000000000000 ) ) ;
#8566 = CARTESIAN_POINT ( 'NONE',  ( -2.162160676586881955E-15, 2.625000002731183724, -35.31076352940723240 ) ) ;
#8567 = CARTESIAN_POINT ( 'NONE',  ( 26.06988505166735592, 42.37017333425730925, 7.025853678916393896 ) ) ;
#8568 =( BOUNDED_CURVE ( )  B_SPLINE_CURVE ( 2, ( #17614, #14527, #20194, #4732, #14699, #27910, #28076, #17274, #4565, #32700, #14866, #24818, #30294 ),
 .UNSPECIFIED., .F., .T. ) 
 B_SPLINE_CURVE_WITH_KNOTS ( ( 3, 2, 2, 2, 2, 2, 3 ),
 ( 0.3500000000000000333, 0.3599999999999999867, 0.3800000000000000044, 0.4000000000000000222, 0.4199999999999999845, 0.4400000000000000022, 0.4500000000000000111 ),
 .UNSPECIFIED. ) 
 CURVE ( )  GEOMETRIC_REPRESENTATION_ITEM ( )  RATIONAL_B_SPLINE_CURVE ( ( 0.9755282581475768211, 0.9755282581475768211, 1.000000000000000000, 0.9510565162951535312, 1.000000000000000000, 0.9510565162951535312, 1.000000000000000000, 0.9510565162951535312, 1.000000000000000000, 0.9510565162951535312, 1.000000000000000000, 0.9755282581475768211, 0.9755282581475768211 ) ) 
 REPRESENTATION_ITEM ( '' )  );
#8569 = CARTESIAN_POINT ( 'NONE',  ( 1.076200423132605543E-16, 52.00000000000000711, -46.18802153517007980 ) ) ;
#8570 = CARTESIAN_POINT ( 'NONE',  ( 0.000000000000000000, 80.00000000000001421, 0.000000000000000000 ) ) ;
#8571 = UNCERTAINTY_MEASURE_WITH_UNIT (LENGTH_MEASURE( 1.000000000000000082E-05 ), #1661, 'distance_accuracy_value', 'NONE');
#8572 = CARTESIAN_POINT ( 'NONE',  ( -20.75514604977248823, 30.82500000273119767, -28.56700777964554305 ) ) ;
#8573 = FACE_OUTER_BOUND ( 'NONE', #18017, .T. ) ;
#8574 = CARTESIAN_POINT ( 'NONE',  ( -10.04305231718578462, 58.90000000546238823, 30.90933677959249337 ) ) ;
#8575 = CARTESIAN_POINT ( 'NONE',  ( 7.468012846824281681, 59.26003499907601935, -28.02196122052058058 ) ) ;
#8576 = CARTESIAN_POINT ( 'NONE',  ( -32.50000000000000000, 48.60000000546236976, 10.55989012756946366 ) ) ;
#8577 = CARTESIAN_POINT ( 'NONE',  ( -8.601468415847515203, 71.67500000273116711, 11.83890561707634959 ) ) ;
#8578 = CARTESIAN_POINT ( 'NONE',  ( 24.50000000000000000, 0.000000000000000000, 0.000000000000000000 ) ) ;
#8579 = CARTESIAN_POINT ( 'NONE',  ( -13.97622843553632421, 22.45572916666666430, -24.20753774853731599 ) ) ;
#8580 = CARTESIAN_POINT ( 'NONE',  ( -33.58253175000000113, 75.22500000273119269, 10.91162601494193929 ) ) ;
#8581 = CARTESIAN_POINT ( 'NONE',  ( -28.01184896238304134, 32.33854166666666430, -7.505752307972844761 ) ) ;
#8582 = CARTESIAN_POINT ( 'NONE',  ( 23.41746824999999887, 15.22499999726880482, -7.608796670333727974 ) ) ;
#8583 = VERTEX_POINT ( 'NONE', #16295 ) ;
#8584 = CARTESIAN_POINT ( 'NONE',  ( -25.98046417659859486, 47.66965250092398065, -15.04653450569291628 ) ) ;
#8585 = CARTESIAN_POINT ( 'NONE',  ( -26.29305231718579350, 20.30000000546237970, -19.10302069950537884 ) ) ;
#8586 = CARTESIAN_POINT ( 'NONE',  ( -20.50609665441004736, 49.81249999999999289, -20.50609665440969565 ) ) ;
#8587 = CARTESIAN_POINT ( 'NONE',  ( -28.01184896238290278, 66.42708333333332860, 7.505752307973363457 ) ) ;
#8588 = CARTESIAN_POINT ( 'NONE',  ( -20.75514604977248112, 49.67500000273118133, 28.56700777964554661 ) ) ;
#8589 = CARTESIAN_POINT ( 'NONE',  ( -10.04305231718578462, 52.90000000546238113, 30.90933677959249337 ) ) ;
#8590 = CARTESIAN_POINT ( 'NONE',  ( -11.25946833292375793, 79.17500000273119554, -8.180482586598733619 ) ) ;
#8591 = CARTESIAN_POINT ( 'NONE',  ( -20.75514604977248823, 34.82500000273118701, -28.56700777964554305 ) ) ;
#8592 = CARTESIAN_POINT ( 'NONE',  ( 7.570916362186207671, 11.59999999999999964, 23.30088464923126779 ) ) ;
#8593 = CARTESIAN_POINT ( 'NONE',  ( -27.16883889988624290, 65.17500000273118133, -19.73931689729374028 ) ) ;
#8594 =( NAMED_UNIT ( * ) PLANE_ANGLE_UNIT ( ) SI_UNIT ( $, .RADIAN. ) );
#8595 = CARTESIAN_POINT ( 'NONE',  ( -26.29305231718578995, 42.20000000000001705, 19.10302069950538595 ) ) ;
#8596 = CARTESIAN_POINT ( 'NONE',  ( -7.236395654485763274, 12.02499999726880375, 22.27133577429736633 ) ) ;
#8597 = ADVANCED_FACE ( 'NONE', ( #26587 ), #8286, .F. ) ;
#8598 = CARTESIAN_POINT ( 'NONE',  ( -27.16883889988623935, 1.575000002731197224, 19.73931689729374739 ) ) ;
#8599 = DIRECTION ( 'NONE',  ( -0.000000000000000000, -1.000000000000000000, -0.000000000000000000 ) ) ;
#8600 = CARTESIAN_POINT ( 'NONE',  ( -8.601468415847518756, 75.07500000273118701, -11.83890561707634781 ) ) ;
#8601 = CARTESIAN_POINT ( 'NONE',  ( 10.37757302488624767, 75.97500000273119269, 31.93888565452638417 ) ) ;
#8602 = FACE_OUTER_BOUND ( 'NONE', #9304, .T. ) ;
#8603 = EDGE_CURVE ( 'NONE', #22348, #33045, #5167, .T. ) ;
#8604 = CARTESIAN_POINT ( 'NONE',  ( 27.16883889988624290, 70.17500000273118133, 19.73931689729373673 ) ) ;
#8605 = VERTEX_POINT ( 'NONE', #31725 ) ;
#8606 = AXIS2_PLACEMENT_3D ( 'NONE', #12627, #10399, #23275 ) ;
#8607 = CYLINDRICAL_SURFACE ( 'NONE', #2542, 24.50000000000000000 ) ;
#8608 = CARTESIAN_POINT ( 'NONE',  ( 19.09188309203661049, 64.42187499999998579, -19.09188309203694445 ) ) ;
#8609 = CARTESIAN_POINT ( 'NONE',  ( 4.635254915624209993, 75.40000000000001990, -14.26584774442730463 ) ) ;
#8610 = CARTESIAN_POINT ( 'NONE',  ( -27.16883889988623935, 45.32500000273119412, 19.73931689729374739 ) ) ;
#8611 = CARTESIAN_POINT ( 'NONE',  ( 20.75514604977249178, 10.07500000273119234, 28.56700777964553950 ) ) ;
#8612 = CARTESIAN_POINT ( 'NONE',  ( -20.75514604977248112, 59.67500000273118133, 28.56700777964554661 ) ) ;
#8613 = CARTESIAN_POINT ( 'NONE',  ( -24.20753774853730889, 45.65885416666666430, 13.97622843553634020 ) ) ;
#8614 = CARTESIAN_POINT ( 'NONE',  ( 20.47846945139902530, 35.78163166759063074, 20.53372385742071771 ) ) ;
#8615 = AXIS2_PLACEMENT_3D ( 'NONE', #31048, #10965, #21439 ) ;
#8616 = CARTESIAN_POINT ( 'NONE',  ( 26.02091320914876960, 32.76263916574268364, 14.97647472619900455 ) ) ;
#8617 = CARTESIAN_POINT ( 'NONE',  ( 32.50000000000000000, 67.60000000546237686, -10.55989012756945833 ) ) ;
#8618 = CARTESIAN_POINT ( 'NONE',  ( 4.300734207923761154, 77.47500000273116427, 13.23629886949340495 ) ) ;
#8619 = CARTESIAN_POINT ( 'NONE',  ( -7.025853678916861966, 55.53607666574269075, -26.06988505166722803 ) ) ;
#8620 = CARTESIAN_POINT ( 'NONE',  ( 14.47279130897151767, 14.92499999726881299, -19.92008829642072598 ) ) ;
#8621 = CARTESIAN_POINT ( 'NONE',  ( 20.08610463437158344, 13.20000000546237651, 27.64615127144129403 ) ) ;
#8622 = ORIENTED_EDGE ( 'NONE', *, *, #132, .F. ) ;
#8623 = CARTESIAN_POINT ( 'NONE',  ( 27.16883889988624290, 50.17500000273118843, 19.73931689729373673 ) ) ;
#8624 = CARTESIAN_POINT ( 'NONE',  ( 20.08610463437157279, 51.29999999999997584, -27.64615127144129758 ) ) ;
#8625 = CARTESIAN_POINT ( 'NONE',  ( -0.04044903254992426173, 53.39881916759064495, 27.95245687107223276 ) ) ;
#8626 = CARTESIAN_POINT ( 'NONE',  ( -33.58253175000000113, 67.27500000273117564, -10.91162601494193218 ) ) ;
#8627 = ORIENTED_EDGE ( 'NONE', *, *, #4965, .T. ) ;
#8628 = CARTESIAN_POINT ( 'NONE',  ( 33.58253175000000113, 16.12500000273119127, -4.112674001490185761E-15 ) ) ;
#8629 = CARTESIAN_POINT ( 'NONE',  ( 20.50609665441005092, 24.03124999999999645, 20.50609665440969209 ) ) ;
#8630 = ORIENTED_EDGE ( 'NONE', *, *, #2230, .F. ) ;
#8631 = DIRECTION ( 'NONE',  ( -1.000000000000000000, 0.000000000000000000, 0.000000000000000000 ) ) ;
#8632 = CARTESIAN_POINT ( 'NONE',  ( 6.486482029760649416E-15, 57.62500000273119127, 35.31076352940723240 ) ) ;
#8633 = CARTESIAN_POINT ( 'NONE',  ( 2.740863092043355209E-13, 58.83593750000000000, 30.02300923189239512 ) ) ;
#8634 = AXIS2_PLACEMENT_3D ( 'NONE', #33719, #26332, #26166 ) ;
#8635 = CARTESIAN_POINT ( 'NONE',  ( 20.08610463437158344, 19.20000000546236052, 27.64615127144129403 ) ) ;
#8636 = CARTESIAN_POINT ( 'NONE',  ( 7.236395654485760609, 11.52499999726880375, -22.27133577429736633 ) ) ;
#8637 = CARTESIAN_POINT ( 'NONE',  ( -33.58253175000000113, 21.37500000273118062, 0.000000000000000000 ) ) ;
#8638 = DIRECTION ( 'NONE',  ( -1.000000000000000000, 0.000000000000000000, 0.000000000000000000 ) ) ;
#8639 = CARTESIAN_POINT ( 'NONE',  ( -27.95245687107223986, 20.44493083240935150, 0.04044903255043252877 ) ) ;
#8640 = FACE_OUTER_BOUND ( 'NONE', #33617, .T. ) ;
#8641 = CARTESIAN_POINT ( 'NONE',  ( -10.04305231718579172, 33.59999999999999432, -30.90933677959248982 ) ) ;
#8642 = CARTESIAN_POINT ( 'NONE',  ( -32.50000000000000000, 11.89999999999998614, -10.55989012756945478 ) ) ;
#8643 = ORIENTED_EDGE ( 'NONE', *, *, #30311, .T. ) ;
#8644 = CARTESIAN_POINT ( 'NONE',  ( 1.507698388325705758E-15, 3.624999997268822938, -24.62258325217400312 ) ) ;
#8645 = CARTESIAN_POINT ( 'NONE',  ( 4.300734207923757602, 74.27500000273118985, -13.23629886949340673 ) ) ;
#8646 = CARTESIAN_POINT ( 'NONE',  ( -26.07999730980477437, 38.92708333333333570, 6.988114217768305103 ) ) ;
#8647 = CARTESIAN_POINT ( 'NONE',  ( -27.16883889988624290, 26.92500000273118133, -19.73931689729374028 ) ) ;
#8648 = CARTESIAN_POINT ( 'NONE',  ( 6.486482029760649416E-15, 65.62500000273116996, 35.31076352940723240 ) ) ;
#8649 = CARTESIAN_POINT ( 'NONE',  ( 33.58253175000000113, 32.47500000273117138, -10.91162601494193751 ) ) ;
#8650 = CARTESIAN_POINT ( 'NONE',  ( 6.486482029760649416E-15, 17.87500000273119838, 35.31076352940723240 ) ) ;
#8651 = CARTESIAN_POINT ( 'NONE',  ( -27.16883889988623935, 11.57500000273120655, 19.73931689729374739 ) ) ;
#8652 = CARTESIAN_POINT ( 'NONE',  ( -13.94119854578936923, 58.26861083425732346, -24.22776226481241224 ) ) ;
#8653 = CARTESIAN_POINT ( 'NONE',  ( 20.75514604977248467, 72.42500000273119554, -28.56700777964554305 ) ) ;
#8654 = CARTESIAN_POINT ( 'NONE',  ( 28.01184896238290278, 50.95833333333332860, -7.505752307973347470 ) ) ;
#8655 = CARTESIAN_POINT ( 'NONE',  ( 0.000000000000000000, 0.000000000000000000, 0.000000000000000000 ) ) ;
#8656 = CARTESIAN_POINT ( 'NONE',  ( -8.960552108402744065E-16, 78.87500000273118417, -14.63369212191046209 ) ) ;
#8657 = CARTESIAN_POINT ( 'NONE',  ( 26.29305231718579350, 52.79999999999999716, 19.10302069950537529 ) ) ;
#8658 = DIRECTION ( 'NONE',  ( -1.000000000000000000, 0.000000000000000000, 0.000000000000000000 ) ) ;
#8659 = CARTESIAN_POINT ( 'NONE',  ( -20.75514604977248823, 58.82500000273117990, -28.56700777964554305 ) ) ;
#8660 = CARTESIAN_POINT ( 'NONE',  ( 14.47279130897151589, 14.82499999726881690, 19.92008829642072953 ) ) ;
#8661 = CONICAL_SURFACE ( 'NONE', #27847, 14.00000000000000178, 0.2617993877991500740 ) ;
#8662 = ORIENTED_EDGE ( 'NONE', *, *, #1689, .F. ) ;
#8663 = CARTESIAN_POINT ( 'NONE',  ( 33.58253175000000823, 68.27500000273120406, 10.91162601494192863 ) ) ;
#8664 = CARTESIAN_POINT ( 'NONE',  ( -32.50000000000000000, 16.10000000000001208, 10.55989012756946366 ) ) ;
#8665 = CARTESIAN_POINT ( 'NONE',  ( -18.94512977948576093, 3.824999997268818674, 13.76444248337722698 ) ) ;
#8666 = CARTESIAN_POINT ( 'NONE',  ( 19.06425588902592239, 25.46913166759064140, 19.11951029504763611 ) ) ;
#8667 =( BOUNDED_CURVE ( )  B_SPLINE_CURVE ( 2, ( #5099, #12826, #7153, #4926, #9906, #30834, #10083, #20562, #23298, #31007, #20216, #20898, #20738 ),
 .UNSPECIFIED., .F., .F. ) 
 B_SPLINE_CURVE_WITH_KNOTS ( ( 3, 2, 2, 2, 2, 2, 3 ),
 ( 0.5277777777777777901, 0.5333333333333333259, 0.5444444444444443976, 0.5555555555555555802, 0.5666666666666666519, 0.5777777777777777235, 0.5833333333333332593 ),
 .UNSPECIFIED. ) 
 CURVE ( )  GEOMETRIC_REPRESENTATION_ITEM ( )  RATIONAL_B_SPLINE_CURVE ( ( 0.9755282581475768211, 0.9755282581475768211, 1.000000000000000000, 0.9510565162951535312, 1.000000000000000000, 0.9510565162951535312, 1.000000000000000000, 0.9510565162951535312, 1.000000000000000000, 0.9510565162951535312, 1.000000000000000000, 0.9755282581475770431, 0.9755282581475768211 ) ) 
 REPRESENTATION_ITEM ( '' )  );
#8668 = ORIENTED_EDGE ( 'NONE', *, *, #30311, .F. ) ;
#8669 = CARTESIAN_POINT ( 'NONE',  ( 6.486482029760649416E-15, 35.62500000273119127, 35.31076352940723240 ) ) ;
#8670 = CARTESIAN_POINT ( 'NONE',  ( -32.50000000000000000, 68.60000000546237686, 10.55989012756946366 ) ) ;
#8671 = ORIENTED_EDGE ( 'NONE', *, *, #23447, .F. ) ;
#8673 = CARTESIAN_POINT ( 'NONE',  ( 20.50609665441005092, 51.53124999999999289, 20.50609665440969209 ) ) ;
#8672 =( BOUNDED_CURVE ( )  B_SPLINE_CURVE ( 2, ( #31634, #3325, #29397, #1056, #29228, #6225, #21521, #24097, #19115, #8133, #5733, #13795, #29553 ),
 .UNSPECIFIED., .F., .T. ) 
 B_SPLINE_CURVE_WITH_KNOTS ( ( 3, 2, 2, 2, 2, 2, 3 ),
 ( 0.3782051282051281937, 0.3794871794871794712, 0.3820512820512820262, 0.3846153846153846367, 0.3871794871794871917, 0.3897435897435897467, 0.3910256410256410242 ),
 .UNSPECIFIED. ) 
 CURVE ( )  GEOMETRIC_REPRESENTATION_ITEM ( )  RATIONAL_B_SPLINE_CURVE ( ( 0.9755282581475768211, 0.9755282581475768211, 1.000000000000000000, 0.9510565162951535312, 1.000000000000000000, 0.9510565162951535312, 1.000000000000000000, 0.9510565162951535312, 1.000000000000000000, 0.9510565162951535312, 1.000000000000000000, 0.9755282581475768211, 0.9755282581475768211 ) ) 
 REPRESENTATION_ITEM ( '' )  );
#8674 = CARTESIAN_POINT ( 'NONE',  ( 27.16883889988624290, 66.17500000273116711, 19.73931689729373673 ) ) ;
#8675 = CARTESIAN_POINT ( 'NONE',  ( -7.570916362186210335, 2.599999999999991207, -23.30088464923126779 ) ) ;
#8676 = CARTESIAN_POINT ( 'NONE',  ( -20.75514604977248112, 71.42500000273119554, 28.56700777964554661 ) ) ;
#8677 = CARTESIAN_POINT ( 'NONE',  ( -15.01150461594595775, 31.62239583333332860, 26.00068869287368756 ) ) ;
#8678 = CARTESIAN_POINT ( 'NONE',  ( 24.50000000000000355, 4.099999999999986322, -7.960532557706203605 ) ) ;
#8679 = CARTESIAN_POINT ( 'NONE',  ( -10.37757302488624411, 6.975000002731185589, -31.93888565452638417 ) ) ;
#8680 = CARTESIAN_POINT ( 'NONE',  ( 27.16883889988623935, 18.32500000273118346, -19.73931689729374384 ) ) ;
#8681 = CARTESIAN_POINT ( 'NONE',  ( 13.91746825000000065, 75.77500000273120406, 4.522059556121115875 ) ) ;
#8682 = DIRECTION ( 'NONE',  ( -1.000000000000000000, -1.063101997391471025E-16, 0.000000000000000000 ) ) ;
#8683 = CARTESIAN_POINT ( 'NONE',  ( -20.53372385742107653, 41.49961833240934794, -20.47846945139867003 ) ) ;
#8684 = CARTESIAN_POINT ( 'NONE',  ( 4.635254915624212657, 80.60000000000000853, 14.26584774442730286 ) ) ;
#8685 = CARTESIAN_POINT ( 'NONE',  ( -2.584737979205442066E-13, 50.24218750000000711, -30.02300923189239867 ) ) ;
#8686 = CARTESIAN_POINT ( 'NONE',  ( 0.000000000000000000, 96.00000000000002842, 0.000000000000000000 ) ) ;
#8687 = CARTESIAN_POINT ( 'NONE',  ( -26.29305231718578995, 38.70000000546236407, 19.10302069950538595 ) ) ;
#8688 = CARTESIAN_POINT ( 'NONE',  ( -7.025853678916861966, 65.84857666574268364, -26.06988505166722803 ) ) ;
#8689 = CARTESIAN_POINT ( 'NONE',  ( 6.486482029760649416E-15, 41.62500000273116996, 35.31076352940723240 ) ) ;
#8690 = CARTESIAN_POINT ( 'NONE',  ( 9.270509831248423538, 73.55000000546235128, -12.75976212528059861 ) ) ;
#8691 = CARTESIAN_POINT ( 'NONE',  ( 33.58253175000000113, 50.47500000273117848, -10.91162601494193751 ) ) ;
#8692 = CARTESIAN_POINT ( 'NONE',  ( 6.486482029760648627E-15, 33.87500000273118417, 35.31076352940722529 ) ) ;
#8693 = CARTESIAN_POINT ( 'NONE',  ( -6.220434760165790777, 16.99999999999999645, 23.40342332511181667 ) ) ;
#8694 = CARTESIAN_POINT ( 'NONE',  ( 2.584737979205442066E-13, 24.46093749999999645, 27.95245687107223276 ) ) ;
#8695 = CARTESIAN_POINT ( 'NONE',  ( 0.000000000000000000, 82.00000000000001421, -15.00000000000000000 ) ) ;
#8696 = CARTESIAN_POINT ( 'NONE',  ( -26.29305231718578995, 44.70000000546237118, 19.10302069950538595 ) ) ;
#8697 = CARTESIAN_POINT ( 'NONE',  ( 10.04305231718578817, 71.40000000000000568, -30.90933677959249337 ) ) ;
#8698 = CARTESIAN_POINT ( 'NONE',  ( -10.37757302488623701, 9.525000002731195181, 31.93888565452638417 ) ) ;
#8699 = CARTESIAN_POINT ( 'NONE',  ( -18.94512977948575738, 5.424999997268809437, -13.76444248337723231 ) ) ;
#8700 = CARTESIAN_POINT ( 'NONE',  ( -10.04305231718579172, 52.10000000546239107, -30.90933677959248982 ) ) ;
#8701 = CARTESIAN_POINT ( 'NONE',  ( -26.09010956794245217, 24.02565999907602290, -6.950374756619243755 ) ) ;
#8702 = CARTESIAN_POINT ( 'NONE',  ( 0.000000000000000000, 80.00000000000001421, 0.000000000000000000 ) ) ;
#8703 = CARTESIAN_POINT ( 'NONE',  ( 27.16883889988624290, 21.92500000273117777, 19.73931689729373673 ) ) ;
#8704 = CARTESIAN_POINT ( 'NONE',  ( 23.41746825000000243, 9.024999997268826846, 7.608796670333735079 ) ) ;
#8705 = CARTESIAN_POINT ( 'NONE',  ( 13.97622843553633665, 51.67447916666665719, 24.20753774853730889 ) ) ;
#8706 = ORIENTED_EDGE ( 'NONE', *, *, #20063, .F. ) ;
#8707 = CARTESIAN_POINT ( 'NONE',  ( -33.58253175000000113, 55.02500000273118985, -10.91162601494193218 ) ) ;
#8708 = ORIENTED_EDGE ( 'NONE', *, *, #25136, .T. ) ;
#8709 = CARTESIAN_POINT ( 'NONE',  ( 7.505752307973351023, 20.88020833333333215, 28.01184896238290278 ) ) ;
#8710 = CARTESIAN_POINT ( 'NONE',  ( 14.97647472619947351, 25.61236083425731636, 26.02091320914850314 ) ) ;
#8711 = CARTESIAN_POINT ( 'NONE',  ( 32.50000000000000000, 39.10000000000001563, -10.55989012756945833 ) ) ;
#8712 = CARTESIAN_POINT ( 'NONE',  ( -7.236395654485763274, 8.024999997268800200, 22.27133577429736633 ) ) ;
#8713 = CARTESIAN_POINT ( 'NONE',  ( -27.16883889988623935, 27.57500000273119412, 19.73931689729374739 ) ) ;
#8714 = CARTESIAN_POINT ( 'NONE',  ( -26.29305231718579350, 28.30000000546237260, -19.10302069950537884 ) ) ;
#8715 = CARTESIAN_POINT ( 'NONE',  ( -32.50000000000000000, 70.00000000000000000, 0.000000000000000000 ) ) ;
#8716 = DIRECTION ( 'NONE',  ( 0.000000000000000000, 0.000000000000000000, 1.000000000000000000 ) ) ;
#8717 = CARTESIAN_POINT ( 'NONE',  ( 7.313012447739250820E-14, 11.49999999999999112, 24.50000000000000000 ) ) ;
#8718 = CARTESIAN_POINT ( 'NONE',  ( 28.00173670424549499, 59.55767333425731636, 7.543491769121417612 ) ) ;
#8719 = CARTESIAN_POINT ( 'NONE',  ( 20.75514604977249178, 44.07500000273117990, 28.56700777964553950 ) ) ;
#8720 =( NAMED_UNIT ( * ) SI_UNIT ( $, .STERADIAN. ) SOLID_ANGLE_UNIT ( ) );
#8721 = CARTESIAN_POINT ( 'NONE',  ( 18.94512977948575738, 10.92499999726881299, 13.76444248337723408 ) ) ;
#8722 = CARTESIAN_POINT ( 'NONE',  ( -10.04305231718578462, 18.39999999999999858, 30.90933677959249337 ) ) ;
#8723 = CARTESIAN_POINT ( 'NONE',  ( -7.570916362186215665, 9.399999999999991473, 23.30088464923126423 ) ) ;
#8724 = EDGE_CURVE ( 'NONE', #19688, #30562, #19039, .T. ) ;
#8725 = CARTESIAN_POINT ( 'NONE',  ( 6.950374756619257965, 38.63503499907601224, -26.09010956794244507 ) ) ;
#8726 = CARTESIAN_POINT ( 'NONE',  ( -33.58253175000000113, 63.12500000273119127, 0.000000000000000000 ) ) ;
#8727 = CARTESIAN_POINT ( 'NONE',  ( 20.75514604977249178, 56.07500000273117990, 28.56700777964553950 ) ) ;
#8728 = CARTESIAN_POINT ( 'NONE',  ( -23.41746824999999887, 7.524999997268816188, -7.608796670333730638 ) ) ;
#8729 = ADVANCED_FACE ( 'NONE', ( #16626 ), #2265, .T. ) ;
#8730 = CARTESIAN_POINT ( 'NONE',  ( 15.14183272437242422, 4.300000000000009592, -20.84094480462497856 ) ) ;
#8731 = CARTESIAN_POINT ( 'NONE',  ( 10.37757302488624767, 3.725000002731182480, 31.93888565452638417 ) ) ;
#8732 = CARTESIAN_POINT ( 'NONE',  ( 19.11951029504763611, 38.35975666759064495, -19.06425588902591173 ) ) ;
#8733 = CARTESIAN_POINT ( 'NONE',  ( 5.147494310547434893, 25.05125428700921830, 32.49999999999999289 ) ) ;
#8734 = CARTESIAN_POINT ( 'NONE',  ( -32.50000000000000000, 19.99999999999998934, 0.000000000000000000 ) ) ;
#8735 = CARTESIAN_POINT ( 'NONE',  ( -33.58253175000000113, 29.02500000273119340, -10.91162601494193218 ) ) ;
#8736 = CARTESIAN_POINT ( 'NONE',  ( 5.779280353836490358E-15, 57.00000000546238965, 32.49999999999999289 ) ) ;
#8737 = CARTESIAN_POINT ( 'NONE',  ( -10.17814985357208535, -45.51763809020504681, 0.000000000000000000 ) ) ;
#8738 = CARTESIAN_POINT ( 'NONE',  ( 32.50000000000000711, 1.400000005462371799, 10.55989012756945122 ) ) ;
#8739 = EDGE_CURVE ( 'NONE', #15393, #1219, #1434, .T. ) ;
#8740 = CARTESIAN_POINT ( 'NONE',  ( 26.02091320914876960, 56.82513916574268364, 14.97647472619900455 ) ) ;
#8741 = CARTESIAN_POINT ( 'NONE',  ( 20.08610463437158344, 47.20000000546238539, 27.64615127144129403 ) ) ;
#8742 = CARTESIAN_POINT ( 'NONE',  ( 0.000000000000000000, 74.00000000000001421, 0.000000000000000000 ) ) ;
#8743 = LINE ( 'NONE', #21965, #12889 ) ;
#8744 = CARTESIAN_POINT ( 'NONE',  ( 27.95245687107222921, 30.47656250000000355, -2.463307335887066074E-13 ) ) ;
#8745 = CARTESIAN_POINT ( 'NONE',  ( 6.486482029760649416E-15, 75.62500000273121259, 35.31076352940723240 ) ) ;
#8746 = CARTESIAN_POINT ( 'NONE',  ( 28.01184896238304134, 34.05729166666666430, 7.505752307972846538 ) ) ;
#8747 = FACE_OUTER_BOUND ( 'NONE', #29426, .T. ) ;
#8748 = ORIENTED_EDGE ( 'NONE', *, *, #24249, .T. ) ;
#8749 = CARTESIAN_POINT ( 'NONE',  ( 25.98046417659858420, 45.95090250092398065, 15.04653450569292872 ) ) ;
#8750 = CARTESIAN_POINT ( 'NONE',  ( 10.04305231718579705, 9.100000005462391073, 30.90933677959248982 ) ) ;
#8751 = CARTESIAN_POINT ( 'NONE',  ( -28.01184896238304134, 59.83854166666666430, -7.505752307972844761 ) ) ;
#8752 = CARTESIAN_POINT ( 'NONE',  ( 0.000000000000000000, 80.00000000000001421, 0.000000000000000000 ) ) ;
#8753 = CARTESIAN_POINT ( 'NONE',  ( 10.37757302488624056, 50.77500000273118985, -31.93888565452638417 ) ) ;
#8754 = CARTESIAN_POINT ( 'NONE',  ( -32.50000000000000000, 52.50000000546236834, 0.000000000000000000 ) ) ;
#8755 = CARTESIAN_POINT ( 'NONE',  ( 11.25946833292375793, 80.57500000273121543, -8.180482586598735395 ) ) ;
#8756 = CARTESIAN_POINT ( 'NONE',  ( -27.16883889988624290, 38.92500000273118843, -19.73931689729374028 ) ) ;
#8757 = CARTESIAN_POINT ( 'NONE',  ( 5.779280353836490358E-15, 27.00000000546237544, 32.49999999999999289 ) ) ;
#8758 = CARTESIAN_POINT ( 'NONE',  ( -2.162160676586881955E-15, 64.87500000273119838, -35.31076352940723240 ) ) ;
#8759 =( NAMED_UNIT ( * ) SI_UNIT ( $, .STERADIAN. ) SOLID_ANGLE_UNIT ( ) );
#8760 = CARTESIAN_POINT ( 'NONE',  ( 32.50000000000000711, 38.89999999999999147, 10.55989012756945122 ) ) ;
#8761 = CARTESIAN_POINT ( 'NONE',  ( 18.94512977948576093, 10.82499999726882578, -13.76444248337722875 ) ) ;
#8762 =( BOUNDED_CURVE ( )  B_SPLINE_CURVE ( 2, ( #20663, #26129, #15504, #2103, #12576, #18252, #33505, #28867, #20481, #25787, #8104, #28699, #15844, #2452, #23730, #26301, #30932, #2276, #21164, #7425, #31606, #31103, #31272, #12750, #23223, #33682, #7599, #5196, #12918, #25958, #23563, #6193, #13431, #5867, #8601, #5704, #18591, #3458, #18756, #24231, #19248, #23899, #8264, #29199, #14099, #21331, #8765, #29367, #29687, #13929, #11348, #16182, #24393, #21989, #31939, #21658, #21825, #11022, #32272, #26469, #19084, #26637, #29031, #867, #3131, #702, #16674, #18921, #16345, #11188, #27130, #26958, #29524, #11509, #3295, #3625, #370, #24555, #1028, #13604, #32437, #24069, #535, #26801, #32103, #6027, #21492, #8432, #16505, #13761, #5534, #16015, #10856, #2962, #31772, #22326, #22657, #22161, #4294, #8936, #29865, #6868, #14941, #27639, #19919, #27980, #14602, #4127, #25059, #25406, #1884, #33111, #25234, #22485, #27300, #1540, #12016, #32936, #19584, #6698, #9434, #14769, #9613, #1709, #30367, #17347, #24887, #27810, #20095, #12187, #30540, #30032, #7036, #17519, #6537, #14263, #4467, #17010, #27469, #12362, #3958, #6366, #32771, #22830, #19416, #16844, #3792, #24721, #32604, #1197, #11678, #9103, #14432, #9265, #1371, #11847, #19749, #30197, #17181, #4807, #4982, #13211, #23354, #26088, #7556, #18379, #23521, #28151, #18041, #31062, #18212, #20266, #15461, #28654, #33290, #2228, #2410, #4637, #9788, #17867, #30713, #12705, #12877, #2585, #25746, #13049, #7208, #33816, #2747, #15286, #15116, #17691, #23176, #5323, #7892, #25580, #23005, #33980, #33638, #2060, #10137, #28485, #10474, #12536, #20952, #7724, #9962, #15803, #20619, #5151, #20437, #33462, #30887, #10309, #25916, #20787, #31232, #7383, #15637, #28319, #31401, #28825, #26259, #3417, #2920, #19047, #23688, #10643, #153, #21453, #26921, #13891, #24189, #8727, #24358, #3254, #5492, #18877, #21293, #29326, #5989, #8062, #8392, #26762, #13724, #326, #31896, #661, #10979, #21120, #21787, #21620, #26427, #5828, #6150, #828, #29154, #18547, #19211, #13389, #11149, #31733, #28993, #11309, #10813, #8224, #32063, #18718, #5660, #16143, #29648, #29486, #16466, #32235, #15971, #16635, #31564, #16307, #27091, #26596, #8563, #23861, #3093, #3585, #13564, #24027, #496, #11638, #27942, #4086, #6824, #22287, #9225, #19709, #20052, #6998, #27769, #30328, #27595, #32399, #32732, #17480, #14057, #24519, #32565, #25190, #9391, #4254, #19875, #1500, #14561, #29993, #30155, #1668, #6659, #17142, #24682, #17307, #22616, #22122, #19378, #25020, #24848, #8894, #29824, #11977, #11474, #3919, #22445, #14729, #32892, #9575, #12143, #3752, #33069, #30497, #989, #21948, #14392, #14226, #6328, #16805, #27261, #1156, #9064, #19545, #6497, #16970, #27428, #1328, #11811, #28612, #33245, #4597, #33944, #7167, #5112, #15245, #15596, #23313, #31194, #22964, #14900, #10097, #12662, #31361, #4767, #26050, #9743, #25707, #28447, #25542, #4425, #33778, #15074, #20576, #2544, #2188, #23131, #31020, #20751, #25364, #7339, #30848, #28110, #1842, #13010, #10435, #7684, #22792, #23482, #33422, #2020, #33597, #7517, #18002, #9920, #12495, #4938, #15420, #12839, #20229, #20397, #20910, #25874, #7853, #12322, #18341, #17649, #30669, #17824, #2366, #18170, #28281, #10269, #13855, #32029, #18682, #10943, #5624, #21418, #26391, #26727, #2884, #13350, #23823, #24321, #24154, #11114, #19010, #13175, #8526, #26221, #461, #794, #21254, #3222, #29121, #5284, #23652, #18843, #31861, #289, #8354, #10777, #16436, #8191, #13690, #15767, #3055, #26559, #625, #2713, #29289, #21583, #8692, #31698, #5789, #114, #28786, #16108, #32198, #13526, #16270, #29454, #23989, #5956, #10606, #26888, #21084, #3385, #31533, #8026, #11277, #21753, #18512, #28958, #5454, #15935, #1115, #6115, #12104, #3879, #19834, #24481, #9352, #27557, #29782, #1626, #9025, #14519, #6287, #19338, #16763, #22248, #6458, #16932, #27390, #29613, #14352, #3546, #17099, #11766, #32525, #19507, #9187, #17266, #21912, #16598, #27053, #24809, #22408, #30287, #19671, #4217, #32856, #32692, #955, #1287, #27222, #30116, #6620, #14018, #4045, #24978, #1461, #3715, #11939, #6788, #27729, #11435, #14691, #25150, #32362, #22575, #33026, #19176, #24641, #8856, #14185, #11600, #22081, #29954, #33555, #4384, #15381, #20012, #7126, #23443, #10055, #2325, #17782, #28575, #33735, #14859, #9705, #5071, #12278, #10232, #20357, #20712, #25325, #9531, #28069, #30459, #15206, #28240, #2501, #9877, #31154, #1800, #30804, #20536, #30629, #6956, #28410, #20185, #25670, #7645, #7297, #4725, #25837, #17961, #30980, #12969, #2149, #18131, #22751, #15555, #4900, #17607, #26008, #33381, #12799, #4556, #15035, #25500, #12624, #23092, #7480, #23272, #17440, #27902, #33202, #1980, #12455, #22925, #13307, #23950, #31989, #2677, #20874, #10395, #31656, #3183, #24117, #419, #18972, #13652, #13485, #15727, #26849, #584, #16233, #10906, #18302, #18642, #3013, #21378, #10564, #8153, #31823, #21211, #31322, #8485, #8314, #13135, #29079, #16396, #11075, #5414, #26519, #21043, #21540, #29417, #31493, #5245, #5919, #7983, #18471, #18804, #28913, #15893, #26349, #3346, #29248, #26687, #13816, #28747, #33904, #7813, #26182, #23609, #5752, #249, #77, #2839, #5584, #23782, #10734, #16064, #19468, #29917, #30244, #17229, #4007, #6583, #3839, #8651, #8987, #27354, #27689, #752, #8815, #1422, #19632, #14481, #30077, #11726, #14314, #6247, #6419, #11900, #16891, #24769, #918, #27520, #32819, #21874, #29573, #24937, #1079, #19136, #6074, #1247, #21712, #14149, #32655, #22372, #22208, #19796, #9150, #13978, #17058, #9311, #6749, #4179, #24605, #24441, #24283, #11236, #16558, #32158, #27011, #32324, #3508, #11397, #19298, #32485, #29742, #16727, #27182, #3675, #11559, #22041, #5328, #25463, #26264, #33986, #7899, #4346, #25113, #20318, #22886, #8067, #14993, #2752, #9490, #1938, #5157, #1758, #14653, #10479, #14821, #30767, #15809, #12416, #33343, #7729, #31406, #23526, #17572, #7088, #25286, #12065, #23693, #10649, #18384, #32986, #159, #33164, #12238, #9840, #18218, #28662, #9667, #22714, #15642, #26093, #20957, #28830 ),
 .UNSPECIFIED., .F., .F. ) 
 B_SPLINE_CURVE_WITH_KNOTS ( ( 3, 2, 2, 2, 2, 2, 2, 2, 2, 2, 2, 2, 2, 2, 2, 2, 2, 2, 2, 2, 2, 2, 2, 2, 2, 2, 2, 2, 2, 2, 2, 2, 2, 2, 2, 2, 2, 2, 2, 2, 2, 2, 2, 2, 2, 2, 2, 2, 2, 2, 2, 2, 2, 2, 2, 2, 2, 2, 2, 2, 2, 2, 2, 2, 2, 2, 2, 2, 2, 2, 2, 2, 2, 2, 2, 2, 2, 2, 2, 2, 2, 2, 2, 2, 2, 2, 2, 2, 2, 2, 2, 2, 2, 2, 2, 2, 2, 2, 2, 2, 2, 2, 2, 2, 2, 2, 2, 2, 2, 2, 2, 2, 2, 2, 2, 2, 2, 2, 2, 2, 2, 2, 2, 2, 2, 2, 2, 2, 2, 2, 2, 2, 2, 2, 2, 2, 2, 2, 2, 2, 2, 2, 2, 2, 2, 2, 2, 2, 2, 2, 2, 2, 2, 2, 2, 2, 2, 2, 2, 2, 2, 2, 2, 2, 2, 2, 2, 2, 2, 2, 2, 2, 2, 2, 2, 2, 2, 2, 2, 2, 2, 2, 2, 2, 2, 2, 2, 2, 2, 2, 2, 2, 2, 2, 2, 2, 2, 2, 2, 2, 2, 2, 2, 2, 2, 2, 2, 2, 2, 2, 2, 2, 2, 2, 2, 2, 2, 2, 2, 2, 2, 2, 2, 2, 2, 2, 2, 2, 2, 2, 2, 2, 2, 2, 2, 2, 2, 2, 2, 2, 2, 2, 2, 2, 2, 2, 2, 2, 2, 2, 2, 2, 2, 2, 2, 2, 2, 2, 2, 2, 2, 2, 2, 2, 2, 2, 2, 2, 2, 2, 2, 2, 2, 2, 2, 2, 2, 2, 2, 2, 2, 2, 2, 2, 2, 2, 2, 2, 2, 2, 2, 2, 2, 2, 2, 2, 2, 2, 2, 2, 2, 2, 2, 2, 2, 2, 2, 2, 2, 2, 2, 2, 2, 2, 2, 2, 2, 2, 2, 2, 2, 2, 2, 2, 2, 2, 2, 2, 2, 2, 2, 2, 2, 2, 2, 2, 2, 2, 2, 2, 2, 2, 2, 2, 2, 2, 2, 2, 2, 2, 2, 2, 2, 2, 2, 2, 2, 2, 2, 2, 2, 2, 2, 2, 2, 2, 2, 2, 2, 2, 2, 2, 2, 2, 2, 2, 2, 2, 2, 2, 2, 2, 2, 2, 2, 2, 2, 2, 2, 2, 3 ),
 ( 0.000000000000000000, 0.002564102564102564100, 0.005128205128205128201, 0.007692307692307692735, 0.01025641025641025640, 0.01282051282051282007, 0.01538461538461538547, 0.01794871794871794740, 0.02051282051282051280, 0.02307692307692307820, 0.02564102564102564014, 0.02820512820512820554, 0.03076923076923077094, 0.03333333333333333287, 0.03589743589743589480, 0.03846153846153846367, 0.04102564102564102561, 0.04358974358974358754, 0.04615384615384615641, 0.04871794871794871834, 0.05128205128205128027, 0.05384615384615384914, 0.05641025641025641107, 0.05897435897435897301, 0.06153846153846154188, 0.06410256410256409687, 0.06666666666666666574, 0.06923076923076923461, 0.07179487179487178961, 0.07435897435897435848, 0.07692307692307692735, 0.07948717948717948234, 0.08205128205128205121, 0.08461538461538462008, 0.08717948717948717507, 0.08974358974358974395, 0.09230769230769231282, 0.09487179487179486781, 0.09743589743589743668, 0.1000000000000000056, 0.1025641025641025605, 0.1051282051282051294, 0.1076923076923076983, 0.1102564102564102533, 0.1128205128205128221, 0.1153846153846153910, 0.1179487179487179460, 0.1205128205128205149, 0.1230769230769230838, 0.1256410256410256387, 0.1282051282051281937, 0.1307692307692307765, 0.1333333333333333315, 0.1358974358974358865, 0.1384615384615384692, 0.1410256410256410242, 0.1435897435897435792, 0.1461538461538461620, 0.1487179487179487170, 0.1512820512820512719, 0.1538461538461538547, 0.1564102564102564097, 0.1589743589743589647, 0.1615384615384615474, 0.1641025641025641024, 0.1666666666666666574, 0.1692307692307692402, 0.1717948717948717952, 0.1743589743589743501, 0.1769230769230769329, 0.1794871794871794879, 0.1820512820512820429, 0.1846153846153846256, 0.1871794871794871806, 0.1897435897435897356, 0.1923076923076923184, 0.1948717948717948734, 0.1974358974358974284, 0.2000000000000000111, 0.2025641025641025661, 0.2051282051282051211, 0.2076923076923077038, 0.2102564102564102588, 0.2128205128205128138, 0.2153846153846153966, 0.2179487179487179516, 0.2205128205128205066, 0.2230769230769230893, 0.2256410256410256443, 0.2282051282051281993, 0.2307692307692307820, 0.2333333333333333370, 0.2358974358974358920, 0.2384615384615384748, 0.2410256410256410298, 0.2435897435897435848, 0.2461538461538461675, 0.2487179487179487225, 0.2512820512820512775, 0.2538461538461538325, 0.2564102564102563875, 0.2589743589743589980, 0.2615384615384615530, 0.2641025641025641080, 0.2666666666666666630, 0.2692307692307692180, 0.2717948717948717730, 0.2743589743589743835, 0.2769230769230769384, 0.2794871794871794934, 0.2820512820512820484, 0.2846153846153846034, 0.2871794871794871584, 0.2897435897435897689, 0.2923076923076923239, 0.2948717948717948789, 0.2974358974358974339, 0.2999999999999999889, 0.3025641025641025439, 0.3051282051282051544, 0.3076923076923077094, 0.3102564102564102644, 0.3128205128205128194, 0.3153846153846153744, 0.3179487179487179294, 0.3205128205128205399, 0.3230769230769230949, 0.3256410256410256499, 0.3282051282051282048, 0.3307692307692307598, 0.3333333333333333148, 0.3358974358974358698, 0.3384615384615384803, 0.3410256410256410353, 0.3435897435897435903, 0.3461538461538461453, 0.3487179487179487003, 0.3512820512820512553, 0.3538461538461538658, 0.3564102564102564208, 0.3589743589743589758, 0.3615384615384615308, 0.3641025641025640858, 0.3666666666666666408, 0.3692307692307692513, 0.3717948717948718063, 0.3743589743589743613, 0.3769230769230769162, 0.3794871794871794712, 0.3820512820512820262, 0.3846153846153846367, 0.3871794871794871917, 0.3897435897435897467, 0.3923076923076923017, 0.3948717948717948567, 0.3974358974358974117, 0.4000000000000000222, 0.4025641025641025772, 0.4051282051282051322, 0.4076923076923076872, 0.4102564102564102422, 0.4128205128205127972, 0.4153846153846154077, 0.4179487179487179627, 0.4205128205128205177, 0.4230769230769230727, 0.4256410256410256276, 0.4282051282051281826, 0.4307692307692307931, 0.4333333333333333481, 0.4358974358974359031, 0.4384615384615384581, 0.4410256410256410131, 0.4435897435897435681, 0.4461538461538461786, 0.4487179487179487336, 0.4512820512820512886, 0.4538461538461538436, 0.4564102564102563986, 0.4589743589743589536, 0.4615384615384615641, 0.4641025641025641191, 0.4666666666666666741, 0.4692307692307692291, 0.4717948717948717841, 0.4743589743589743390, 0.4769230769230769496, 0.4794871794871795045, 0.4820512820512820595, 0.4846153846153846145, 0.4871794871794871695, 0.4897435897435897245, 0.4923076923076923350, 0.4948717948717948900, 0.4974358974358974450, 0.5000000000000000000, 0.5025641025641025550, 0.5051282051282051100, 0.5076923076923076650, 0.5102564102564102200, 0.5128205128205127750, 0.5153846153846153300, 0.5179487179487179960, 0.5205128205128205510, 0.5230769230769231060, 0.5256410256410256610, 0.5282051282051282159, 0.5307692307692307709, 0.5333333333333333259, 0.5358974358974358809, 0.5384615384615384359, 0.5410256410256409909, 0.5435897435897435459, 0.5461538461538461009, 0.5487179487179487669, 0.5512820512820513219, 0.5538461538461538769, 0.5564102564102564319, 0.5589743589743589869, 0.5615384615384615419, 0.5641025641025640969, 0.5666666666666666519, 0.5692307692307692069, 0.5717948717948717618, 0.5743589743589743168, 0.5769230769230768718, 0.5794871794871795379, 0.5820512820512820928, 0.5846153846153846478, 0.5871794871794872028, 0.5897435897435897578, 0.5923076923076923128, 0.5948717948717948678, 0.5974358974358974228, 0.5999999999999999778, 0.6025641025641025328, 0.6051282051282050878, 0.6076923076923076428, 0.6102564102564103088, 0.6128205128205128638, 0.6153846153846154188, 0.6179487179487179738, 0.6205128205128205288, 0.6230769230769230838, 0.6256410256410256387, 0.6282051282051281937, 0.6307692307692307487, 0.6333333333333333037, 0.6358974358974358587, 0.6384615384615384137, 0.6410256410256410797, 0.6435897435897436347, 0.6461538461538461897, 0.6487179487179487447, 0.6512820512820512997, 0.6538461538461538547, 0.6564102564102564097, 0.6589743589743589647, 0.6615384615384615197, 0.6641025641025640747, 0.6666666666666666297, 0.6692307692307691847, 0.6717948717948717396, 0.6743589743589744057, 0.6769230769230769607, 0.6794871794871795156, 0.6820512820512820706, 0.6846153846153846256, 0.6871794871794871806, 0.6897435897435897356, 0.6923076923076922906, 0.6948717948717948456, 0.6974358974358974006, 0.6999999999999999556, 0.7025641025641025106, 0.7051282051282051766, 0.7076923076923077316, 0.7102564102564102866, 0.7128205128205128416, 0.7153846153846153966, 0.7179487179487179516, 0.7205128205128205066, 0.7230769230769230616, 0.7256410256410256165, 0.7282051282051281715, 0.7307692307692307265, 0.7333333333333332815, 0.7358974358974359475, 0.7384615384615385025, 0.7410256410256410575, 0.7435897435897436125, 0.7461538461538461675, 0.7487179487179487225, 0.7512820512820512775, 0.7538461538461538325, 0.7564102564102563875, 0.7589743589743589425, 0.7615384615384614975, 0.7641025641025640525, 0.7666666666666667185, 0.7692307692307692735, 0.7717948717948718285, 0.7743589743589743835, 0.7769230769230769384, 0.7794871794871794934, 0.7820512820512820484, 0.7846153846153846034, 0.7871794871794871584, 0.7897435897435897134, 0.7923076923076922684, 0.7948717948717948234, 0.7974358974358974894, 0.8000000000000000444, 0.8025641025641025994, 0.8051282051282051544, 0.8076923076923077094, 0.8102564102564102644, 0.8128205128205128194, 0.8153846153846153744, 0.8179487179487179294, 0.8205128205128204844, 0.8230769230769230393, 0.8256410256410255943, 0.8282051282051282604, 0.8307692307692308153, 0.8333333333333333703, 0.8358974358974359253, 0.8384615384615384803, 0.8410256410256410353, 0.8435897435897435903, 0.8461538461538461453, 0.8487179487179487003, 0.8512820512820512553, 0.8538461538461538103, 0.8564102564102563653, 0.8589743589743589203, 0.8615384615384615863, 0.8641025641025641413, 0.8666666666666666963, 0.8692307692307692513, 0.8717948717948718063, 0.8743589743589743613, 0.8769230769230769162, 0.8794871794871794712, 0.8820512820512820262, 0.8846153846153845812, 0.8871794871794871362, 0.8897435897435896912, 0.8923076923076923572, 0.8948717948717949122, 0.8974358974358974672, 0.9000000000000000222, 0.9025641025641025772, 0.9051282051282051322, 0.9076923076923076872, 0.9102564102564102422, 0.9128205128205127972, 0.9153846153846153522, 0.9179487179487179072, 0.9205128205128204621, 0.9230769230769231282, 0.9256410256410256832, 0.9282051282051282382, 0.9307692307692307931, 0.9333333333333333481, 0.9358974358974359031, 0.9384615384615384581, 0.9410256410256410131, 0.9435897435897435681, 0.9461538461538461231, 0.9487179487179486781, 0.9512820512820512331, 0.9538461538461538991, 0.9564102564102564541, 0.9589743589743590091, 0.9615384615384615641, 0.9641025641025641191, 0.9666666666666666741, 0.9692307692307692291, 0.9717948717948717841, 0.9743589743589743390, 0.9769230769230768940, 0.9794871794871794490, 0.9820512820512820040, 0.9846153846153846700, 0.9871794871794872250, 0.9897435897435897800, 0.9923076923076923350, 0.9948717948717948900, 0.9974358974358974450, 1.000000000000000000 ),
 .UNSPECIFIED. ) 
 CURVE ( )  GEOMETRIC_REPRESENTATION_ITEM ( )  RATIONAL_B_SPLINE_CURVE ( ( 1.000000000000000000, 0.9510565162951535312, 1.000000000000000000, 0.9510565162951535312, 1.000000000000000000, 0.9510565162951535312, 1.000000000000000000, 0.9510565162951535312, 1.000000000000000000, 0.9510565162951535312, 1.000000000000000000, 0.9510565162951535312, 1.000000000000000000, 0.9510565162951535312, 1.000000000000000000, 0.9510565162951535312, 1.000000000000000000, 0.9510565162951535312, 1.000000000000000000, 0.9510565162951535312, 1.000000000000000000, 0.9510565162951535312, 1.000000000000000000, 0.9510565162951535312, 1.000000000000000000, 0.9510565162951535312, 1.000000000000000000, 0.9510565162951535312, 1.000000000000000000, 0.9510565162951535312, 1.000000000000000000, 0.9510565162951535312, 1.000000000000000000, 0.9510565162951535312, 1.000000000000000000, 0.9510565162951535312, 1.000000000000000000, 0.9510565162951535312, 1.000000000000000000, 0.9510565162951535312, 1.000000000000000000, 0.9510565162951535312, 1.000000000000000000, 0.9510565162951535312, 1.000000000000000000, 0.9510565162951535312, 1.000000000000000000, 0.9510565162951535312, 1.000000000000000000, 0.9510565162951535312, 1.000000000000000000, 0.9510565162951535312, 1.000000000000000000, 0.9510565162951535312, 1.000000000000000000, 0.9510565162951535312, 1.000000000000000000, 0.9510565162951535312, 1.000000000000000000, 0.9510565162951535312, 1.000000000000000000, 0.9510565162951535312, 1.000000000000000000, 0.9510565162951535312, 1.000000000000000000, 0.9510565162951535312, 1.000000000000000000, 0.9510565162951535312, 1.000000000000000000, 0.9510565162951535312, 1.000000000000000000, 0.9510565162951535312, 1.000000000000000000, 0.9510565162951535312, 1.000000000000000000, 0.9510565162951535312, 1.000000000000000000, 0.9510565162951535312, 1.000000000000000000, 0.9510565162951535312, 1.000000000000000000, 0.9510565162951535312, 1.000000000000000000, 0.9510565162951535312, 1.000000000000000000, 0.9510565162951535312, 1.000000000000000000, 0.9510565162951535312, 1.000000000000000000, 0.9510565162951535312, 1.000000000000000000, 0.9510565162951535312, 1.000000000000000000, 0.9510565162951535312, 1.000000000000000000, 0.9510565162951535312, 1.000000000000000000, 0.9510565162951535312, 1.000000000000000000, 0.9510565162951535312, 1.000000000000000000, 0.9510565162951535312, 1.000000000000000000, 0.9510565162951535312, 1.000000000000000000, 0.9510565162951535312, 1.000000000000000000, 0.9510565162951535312, 1.000000000000000000, 0.9510565162951535312, 1.000000000000000000, 0.9510565162951535312, 1.000000000000000000, 0.9510565162951535312, 1.000000000000000000, 0.9510565162951535312, 1.000000000000000000, 0.9510565162951535312, 1.000000000000000000, 0.9510565162951535312, 1.000000000000000000, 0.9510565162951535312, 1.000000000000000000, 0.9510565162951535312, 1.000000000000000000, 0.9510565162951535312, 1.000000000000000000, 0.9510565162951535312, 1.000000000000000000, 0.9510565162951535312, 1.000000000000000000, 0.9510565162951535312, 1.000000000000000000, 0.9510565162951535312, 1.000000000000000000, 0.9510565162951535312, 1.000000000000000000, 0.9510565162951535312, 1.000000000000000000, 0.9510565162951535312, 1.000000000000000000, 0.9510565162951535312, 1.000000000000000000, 0.9510565162951535312, 1.000000000000000000, 0.9510565162951535312, 1.000000000000000000, 0.9510565162951535312, 1.000000000000000000, 0.9510565162951535312, 1.000000000000000000, 0.9510565162951535312, 1.000000000000000000, 0.9510565162951535312, 1.000000000000000000, 0.9510565162951535312, 1.000000000000000000, 0.9510565162951535312, 1.000000000000000000, 0.9510565162951535312, 1.000000000000000000, 0.9510565162951535312, 1.000000000000000000, 0.9510565162951535312, 1.000000000000000000, 0.9510565162951535312, 1.000000000000000000, 0.9510565162951535312, 1.000000000000000000, 0.9510565162951535312, 1.000000000000000000, 0.9510565162951535312, 1.000000000000000000, 0.9510565162951535312, 1.000000000000000000, 0.9510565162951535312, 1.000000000000000000, 0.9510565162951535312, 1.000000000000000000, 0.9510565162951535312, 1.000000000000000000, 0.9510565162951535312, 1.000000000000000000, 0.9510565162951535312, 1.000000000000000000, 0.9510565162951535312, 1.000000000000000000, 0.9510565162951535312, 1.000000000000000000, 0.9510565162951535312, 1.000000000000000000, 0.9510565162951535312, 1.000000000000000000, 0.9510565162951535312, 1.000000000000000000, 0.9510565162951535312, 1.000000000000000000, 0.9510565162951535312, 1.000000000000000000, 0.9510565162951535312, 1.000000000000000000, 0.9510565162951535312, 1.000000000000000000, 0.9510565162951535312, 1.000000000000000000, 0.9510565162951535312, 1.000000000000000000, 0.9510565162951535312, 1.000000000000000000, 0.9510565162951535312, 1.000000000000000000, 0.9510565162951535312, 1.000000000000000000, 0.9510565162951535312, 1.000000000000000000, 0.9510565162951535312, 1.000000000000000000, 0.9510565162951535312, 1.000000000000000000, 0.9510565162951535312, 1.000000000000000000, 0.9510565162951535312, 1.000000000000000000, 0.9510565162951535312, 1.000000000000000000, 0.9510565162951535312, 1.000000000000000000, 0.9510565162951535312, 1.000000000000000000, 0.9510565162951535312, 1.000000000000000000, 0.9510565162951535312, 1.000000000000000000, 0.9510565162951535312, 1.000000000000000000, 0.9510565162951535312, 1.000000000000000000, 0.9510565162951535312, 1.000000000000000000, 0.9510565162951535312, 1.000000000000000000, 0.9510565162951535312, 1.000000000000000000, 0.9510565162951535312, 1.000000000000000000, 0.9510565162951535312, 1.000000000000000000, 0.9510565162951535312, 1.000000000000000000, 0.9510565162951535312, 1.000000000000000000, 0.9510565162951535312, 1.000000000000000000, 0.9510565162951535312, 1.000000000000000000, 0.9510565162951535312, 1.000000000000000000, 0.9510565162951535312, 1.000000000000000000, 0.9510565162951535312, 1.000000000000000000, 0.9510565162951535312, 1.000000000000000000, 0.9510565162951535312, 1.000000000000000000, 0.9510565162951535312, 1.000000000000000000, 0.9510565162951535312, 1.000000000000000000, 0.9510565162951535312, 1.000000000000000000, 0.9510565162951535312, 1.000000000000000000, 0.9510565162951535312, 1.000000000000000000, 0.9510565162951535312, 1.000000000000000000, 0.9510565162951535312, 1.000000000000000000, 0.9510565162951535312, 1.000000000000000000, 0.9510565162951535312, 1.000000000000000000, 0.9510565162951535312, 1.000000000000000000, 0.9510565162951535312, 1.000000000000000000, 0.9510565162951535312, 1.000000000000000000, 0.9510565162951535312, 1.000000000000000000, 0.9510565162951535312, 1.000000000000000000, 0.9510565162951535312, 1.000000000000000000, 0.9510565162951535312, 1.000000000000000000, 0.9510565162951535312, 1.000000000000000000, 0.9510565162951535312, 1.000000000000000000, 0.9510565162951535312, 1.000000000000000000, 0.9510565162951535312, 1.000000000000000000, 0.9510565162951535312, 1.000000000000000000, 0.9510565162951535312, 1.000000000000000000, 0.9510565162951535312, 1.000000000000000000, 0.9510565162951535312, 1.000000000000000000, 0.9510565162951535312, 1.000000000000000000, 0.9510565162951535312, 1.000000000000000000, 0.9510565162951535312, 1.000000000000000000, 0.9510565162951535312, 1.000000000000000000, 0.9510565162951535312, 1.000000000000000000, 0.9510565162951535312, 1.000000000000000000, 0.9510565162951535312, 1.000000000000000000, 0.9510565162951535312, 1.000000000000000000, 0.9510565162951535312, 1.000000000000000000, 0.9510565162951535312, 1.000000000000000000, 0.9510565162951535312, 1.000000000000000000, 0.9510565162951535312, 1.000000000000000000, 0.9510565162951535312, 1.000000000000000000, 0.9510565162951535312, 1.000000000000000000, 0.9510565162951535312, 1.000000000000000000, 0.9510565162951535312, 1.000000000000000000, 0.9510565162951535312, 1.000000000000000000, 0.9510565162951535312, 1.000000000000000000, 0.9510565162951535312, 1.000000000000000000, 0.9510565162951535312, 1.000000000000000000, 0.9510565162951535312, 1.000000000000000000, 0.9510565162951535312, 1.000000000000000000, 0.9510565162951535312, 1.000000000000000000, 0.9510565162951535312, 1.000000000000000000, 0.9510565162951535312, 1.000000000000000000, 0.9510565162951535312, 1.000000000000000000, 0.9510565162951535312, 1.000000000000000000, 0.9510565162951535312, 1.000000000000000000, 0.9510565162951535312, 1.000000000000000000, 0.9510565162951535312, 1.000000000000000000, 0.9510565162951535312, 1.000000000000000000, 0.9510565162951535312, 1.000000000000000000, 0.9510565162951535312, 1.000000000000000000, 0.9510565162951535312, 1.000000000000000000, 0.9510565162951535312, 1.000000000000000000, 0.9510565162951535312, 1.000000000000000000, 0.9510565162951535312, 1.000000000000000000, 0.9510565162951535312, 1.000000000000000000, 0.9510565162951535312, 1.000000000000000000, 0.9510565162951535312, 1.000000000000000000, 0.9510565162951535312, 1.000000000000000000, 0.9510565162951535312, 1.000000000000000000, 0.9510565162951535312, 1.000000000000000000, 0.9510565162951535312, 1.000000000000000000, 0.9510565162951535312, 1.000000000000000000, 0.9510565162951535312, 1.000000000000000000, 0.9510565162951535312, 1.000000000000000000, 0.9510565162951535312, 1.000000000000000000, 0.9510565162951535312, 1.000000000000000000, 0.9510565162951535312, 1.000000000000000000, 0.9510565162951535312, 1.000000000000000000, 0.9510565162951535312, 1.000000000000000000, 0.9510565162951535312, 1.000000000000000000, 0.9510565162951535312, 1.000000000000000000, 0.9510565162951535312, 1.000000000000000000, 0.9510565162951535312, 1.000000000000000000, 0.9510565162951535312, 1.000000000000000000, 0.9510565162951535312, 1.000000000000000000, 0.9510565162951535312, 1.000000000000000000, 0.9510565162951535312, 1.000000000000000000, 0.9510565162951535312, 1.000000000000000000, 0.9510565162951535312, 1.000000000000000000, 0.9510565162951535312, 1.000000000000000000, 0.9510565162951535312, 1.000000000000000000, 0.9510565162951535312, 1.000000000000000000, 0.9510565162951535312, 1.000000000000000000, 0.9510565162951535312, 1.000000000000000000, 0.9510565162951535312, 1.000000000000000000, 0.9510565162951535312, 1.000000000000000000, 0.9510565162951535312, 1.000000000000000000, 0.9510565162951535312, 1.000000000000000000, 0.9510565162951535312, 1.000000000000000000, 0.9510565162951535312, 1.000000000000000000, 0.9510565162951535312, 1.000000000000000000, 0.9510565162951535312, 1.000000000000000000, 0.9510565162951535312, 1.000000000000000000, 0.9510565162951535312, 1.000000000000000000, 0.9510565162951535312, 1.000000000000000000, 0.9510565162951535312, 1.000000000000000000, 0.9510565162951535312, 1.000000000000000000, 0.9510565162951535312, 1.000000000000000000, 0.9510565162951535312, 1.000000000000000000, 0.9510565162951535312, 1.000000000000000000, 0.9510565162951535312, 1.000000000000000000, 0.9510565162951535312, 1.000000000000000000, 0.9510565162951535312, 1.000000000000000000, 0.9510565162951535312, 1.000000000000000000, 0.9510565162951535312, 1.000000000000000000, 0.9510565162951535312, 1.000000000000000000, 0.9510565162951535312, 1.000000000000000000, 0.9510565162951535312, 1.000000000000000000, 0.9510565162951535312, 1.000000000000000000, 0.9510565162951535312, 1.000000000000000000, 0.9510565162951535312, 1.000000000000000000, 0.9510565162951535312, 1.000000000000000000, 0.9510565162951535312, 1.000000000000000000, 0.9510565162951535312, 1.000000000000000000, 0.9510565162951535312, 1.000000000000000000, 0.9510565162951535312, 1.000000000000000000, 0.9510565162951535312, 1.000000000000000000, 0.9510565162951535312, 1.000000000000000000, 0.9510565162951535312, 1.000000000000000000, 0.9510565162951535312, 1.000000000000000000, 0.9510565162951535312, 1.000000000000000000, 0.9510565162951535312, 1.000000000000000000, 0.9510565162951535312, 1.000000000000000000, 0.9510565162951535312, 1.000000000000000000, 0.9510565162951535312, 1.000000000000000000, 0.9510565162951535312, 1.000000000000000000, 0.9510565162951535312, 1.000000000000000000, 0.9510565162951535312, 1.000000000000000000, 0.9510565162951535312, 1.000000000000000000, 0.9510565162951535312, 1.000000000000000000, 0.9510565162951535312, 1.000000000000000000, 0.9510565162951535312, 1.000000000000000000, 0.9510565162951535312, 1.000000000000000000, 0.9510565162951535312, 1.000000000000000000, 0.9510565162951535312, 1.000000000000000000, 0.9510565162951535312, 1.000000000000000000, 0.9510565162951535312, 1.000000000000000000, 0.9510565162951535312, 1.000000000000000000, 0.9510565162951535312, 1.000000000000000000, 0.9510565162951535312, 1.000000000000000000, 0.9510565162951535312, 1.000000000000000000, 0.9510565162951535312, 1.000000000000000000, 0.9510565162951535312, 1.000000000000000000, 0.9510565162951535312, 1.000000000000000000, 0.9510565162951535312, 1.000000000000000000, 0.9510565162951535312, 1.000000000000000000, 0.9510565162951535312, 1.000000000000000000, 0.9510565162951535312, 1.000000000000000000, 0.9510565162951535312, 1.000000000000000000, 0.9510565162951535312, 1.000000000000000000, 0.9510565162951535312, 1.000000000000000000, 0.9510565162951535312, 1.000000000000000000, 0.9510565162951535312, 1.000000000000000000, 0.9510565162951535312, 1.000000000000000000, 0.9510565162951535312, 1.000000000000000000, 0.9510565162951535312, 1.000000000000000000, 0.9510565162951535312, 1.000000000000000000, 0.9510565162951535312, 1.000000000000000000, 0.9510565162951535312, 1.000000000000000000, 0.9510565162951535312, 1.000000000000000000, 0.9510565162951535312, 1.000000000000000000, 0.9510565162951535312, 1.000000000000000000, 0.9510565162951535312, 1.000000000000000000, 0.9510565162951535312, 1.000000000000000000, 0.9510565162951535312, 1.000000000000000000, 0.9510565162951535312, 1.000000000000000000, 0.9510565162951535312, 1.000000000000000000, 0.9510565162951535312, 1.000000000000000000, 0.9510565162951535312, 1.000000000000000000, 0.9510565162951535312, 1.000000000000000000, 0.9510565162951535312, 1.000000000000000000, 0.9510565162951535312, 1.000000000000000000, 0.9510565162951535312, 1.000000000000000000, 0.9510565162951535312, 1.000000000000000000, 0.9510565162951535312, 1.000000000000000000, 0.9510565162951535312, 1.000000000000000000, 0.9510565162951535312, 1.000000000000000000, 0.9510565162951535312, 1.000000000000000000, 0.9510565162951535312, 1.000000000000000000, 0.9510565162951535312, 1.000000000000000000, 0.9510565162951535312, 1.000000000000000000, 0.9510565162951535312, 1.000000000000000000, 0.9510565162951535312, 1.000000000000000000, 0.9510565162951535312, 1.000000000000000000, 0.9510565162951535312, 1.000000000000000000, 0.9510565162951535312, 1.000000000000000000, 0.9510565162951535312, 1.000000000000000000, 0.9510565162951535312, 1.000000000000000000, 0.9510565162951535312, 1.000000000000000000, 0.9510565162951535312, 1.000000000000000000, 0.9510565162951535312, 1.000000000000000000, 0.9510565162951535312, 1.000000000000000000, 0.9510565162951535312, 1.000000000000000000, 0.9510565162951535312, 1.000000000000000000, 0.9510565162951535312, 1.000000000000000000, 0.9510565162951535312, 1.000000000000000000, 0.9510565162951535312, 1.000000000000000000, 0.9510565162951535312, 1.000000000000000000, 0.9510565162951535312, 1.000000000000000000, 0.9510565162951535312, 1.000000000000000000, 0.9510565162951535312, 1.000000000000000000, 0.9510565162951535312, 1.000000000000000000, 0.9510565162951535312, 1.000000000000000000, 0.9510565162951535312, 1.000000000000000000, 0.9510565162951535312, 1.000000000000000000, 0.9510565162951535312, 1.000000000000000000, 0.9510565162951535312, 1.000000000000000000, 0.9510565162951535312, 1.000000000000000000, 0.9510565162951535312, 1.000000000000000000, 0.9510565162951535312, 1.000000000000000000, 0.9510565162951535312, 1.000000000000000000, 0.9510565162951535312, 1.000000000000000000, 0.9510565162951535312, 1.000000000000000000, 0.9510565162951535312, 1.000000000000000000, 0.9510565162951535312, 1.000000000000000000, 0.9510565162951535312, 1.000000000000000000, 0.9510565162951535312, 1.000000000000000000, 0.9510565162951535312, 1.000000000000000000, 0.9510565162951535312, 1.000000000000000000, 0.9510565162951535312, 1.000000000000000000, 0.9510565162951535312, 1.000000000000000000, 0.9510565162951535312, 1.000000000000000000, 0.9510565162951535312, 1.000000000000000000, 0.9510565162951535312, 1.000000000000000000, 0.9510565162951535312, 1.000000000000000000, 0.9510565162951535312, 1.000000000000000000, 0.9510565162951535312, 1.000000000000000000, 0.9510565162951535312, 1.000000000000000000, 0.9510565162951535312, 1.000000000000000000, 0.9510565162951535312, 1.000000000000000000, 0.9510565162951535312, 1.000000000000000000, 0.9510565162951535312, 1.000000000000000000, 0.9510565162951535312, 1.000000000000000000, 0.9510565162951535312, 1.000000000000000000, 0.9510565162951535312, 1.000000000000000000, 0.9510565162951535312, 1.000000000000000000, 0.9510565162951535312, 1.000000000000000000, 0.9510565162951535312, 1.000000000000000000, 0.9510565162951535312, 1.000000000000000000, 0.9510565162951535312, 1.000000000000000000, 0.9510565162951535312, 1.000000000000000000, 0.9510565162951535312, 1.000000000000000000, 0.9510565162951535312, 1.000000000000000000, 0.9510565162951535312, 1.000000000000000000, 0.9510565162951535312, 1.000000000000000000, 0.9510565162951535312, 1.000000000000000000, 0.9510565162951535312, 1.000000000000000000, 0.9510565162951535312, 1.000000000000000000, 0.9510565162951535312, 1.000000000000000000, 0.9510565162951535312, 1.000000000000000000, 0.9510565162951535312, 1.000000000000000000 ) ) 
 REPRESENTATION_ITEM ( '' )  );
#8763 = CARTESIAN_POINT ( 'NONE',  ( -20.75514604977248823, 3.075000002731198112, -28.56700777964554305 ) ) ;
#8764 = CARTESIAN_POINT ( 'NONE',  ( -8.960552108402744065E-16, 76.87500000273118417, -14.63369212191046209 ) ) ;
#8765 = CARTESIAN_POINT ( 'NONE',  ( 10.37757302488624056, 74.77500000273118985, -31.93888565452638417 ) ) ;
#8766 = CARTESIAN_POINT ( 'NONE',  ( -7.570916362186215665, 19.14999999453761959, 23.30088464923126423 ) ) ;
#8767 = CARTESIAN_POINT ( 'NONE',  ( 10.37757302488624767, 69.97500000273119269, 31.93888565452638417 ) ) ;
#8768 = ORIENTED_EDGE ( 'NONE', *, *, #3988, .T. ) ;
#8769 = CARTESIAN_POINT ( 'NONE',  ( -24.50000000000001066, 6.849999994537628645, 7.960532557706201828 ) ) ;
#8770 = CARTESIAN_POINT ( 'NONE',  ( -19.11951029504763611, 12.57850666759064140, 19.06425588902592239 ) ) ;
#8771 = CARTESIAN_POINT ( 'NONE',  ( 15.00000000000000000, 75.09999999999996589, -4.873795443493596835 ) ) ;
#8772 = CARTESIAN_POINT ( 'NONE',  ( -33.58253175000000113, 49.12500000273119127, 0.000000000000000000 ) ) ;
#8773 = CARTESIAN_POINT ( 'NONE',  ( 6.486482029760649416E-15, 9.875000002731187720, 35.31076352940723240 ) ) ;
#8774 = CARTESIAN_POINT ( 'NONE',  ( -10.37757302488623701, 61.77500000273118985, 31.93888565452638417 ) ) ;
#8775 = CARTESIAN_POINT ( 'NONE',  ( 24.20753774853731244, 54.25260416666666430, -13.97622843553633132 ) ) ;
#8776 = CARTESIAN_POINT ( 'NONE',  ( 30.02300923189239867, 35.35194416759064495, 0.04044903254992252006 ) ) ;
#8777 = CARTESIAN_POINT ( 'NONE',  ( -30.02300923189239867, 23.88243083240935505, 0.04044903255044988294 ) ) ;
#8778 = CARTESIAN_POINT ( 'NONE',  ( -20.08610463437156923, 68.80000000546236549, 27.64615127144130113 ) ) ;
#8779 = CARTESIAN_POINT ( 'NONE',  ( 13.91746825000000065, 77.77500000273114722, 4.522059556121114987 ) ) ;
#8780 = CARTESIAN_POINT ( 'NONE',  ( -19.11951029504797006, 58.68711833240935505, -19.06425588902558133 ) ) ;
#8781 = CARTESIAN_POINT ( 'NONE',  ( -23.41746824999999887, 15.62499999726882294, -2.867812753649727150E-15 ) ) ;
#8782 = CARTESIAN_POINT ( 'NONE',  ( 7.890940483122900408E-14, 16.49999999999999645, -24.50000000000000000 ) ) ;
#8783 = ORIENTED_EDGE ( 'NONE', *, *, #25934, .F. ) ;
#8784 = EDGE_CURVE ( 'NONE', #33960, #14496, #6316, .T. ) ;
#8785 = CARTESIAN_POINT ( 'NONE',  ( 6.486482029760649416E-15, 45.87500000273117706, 35.31076352940723240 ) ) ;
#8786 = DIRECTION ( 'NONE',  ( 0.000000000000000000, 0.000000000000000000, -1.000000000000000000 ) ) ;
#8787 = CARTESIAN_POINT ( 'NONE',  ( -26.06988505166735237, 50.96392333425730925, -7.025853678916388567 ) ) ;
#8788 = CARTESIAN_POINT ( 'NONE',  ( 33.58253175000000113, 66.47500000273119269, -10.91162601494193751 ) ) ;
#8789 = ORIENTED_EDGE ( 'NONE', *, *, #29131, .T. ) ;
#8790 = CARTESIAN_POINT ( 'NONE',  ( -10.37757302488623701, 17.52500000273120406, 31.93888565452638417 ) ) ;
#8791 = CARTESIAN_POINT ( 'NONE',  ( 20.50609665441005092, 20.59374999999999645, 20.50609665440969209 ) ) ;
#8792 = VERTEX_POINT ( 'NONE', #1489 ) ;
#8793 = ORIENTED_EDGE ( 'NONE', *, *, #2129, .T. ) ;
#8794 = CARTESIAN_POINT ( 'NONE',  ( -33.04126587500000056, 1.687500001365582758, 0.000000000000000000 ) ) ;
#8795 = CARTESIAN_POINT ( 'NONE',  ( -10.37757302488624411, 54.72500000273117138, -31.93888565452638417 ) ) ;
#8796 = CARTESIAN_POINT ( 'NONE',  ( -7.505752307973343918, 60.41145833333332149, -28.01184896238290989 ) ) ;
#8797 = CARTESIAN_POINT ( 'NONE',  ( 20.08610463437157279, 11.80000000546236194, -27.64615127144129758 ) ) ;
#8798 = CYLINDRICAL_SURFACE ( 'NONE', #21802, 15.00000000000000000 ) ;
#8799 = CARTESIAN_POINT ( 'NONE',  ( 7.236395654485760609, 15.52499999726880731, -22.27133577429736633 ) ) ;
#8800 =( BOUNDED_CURVE ( )  B_SPLINE_CURVE ( 2, ( #18404, #16490, #19071, #3445, #16166, #32091, #8088, #5516, #29183, #23547, #354, #26283, #10498 ),
 .UNSPECIFIED., .F., .T. ) 
 B_SPLINE_CURVE_WITH_KNOTS ( ( 3, 2, 2, 2, 2, 2, 3 ),
 ( 0.5576923076923077094, 0.5589743589743589869, 0.5615384615384615419, 0.5641025641025640969, 0.5666666666666666519, 0.5692307692307692069, 0.5705128205128204844 ),
 .UNSPECIFIED. ) 
 CURVE ( )  GEOMETRIC_REPRESENTATION_ITEM ( )  RATIONAL_B_SPLINE_CURVE ( ( 0.9755282581475768211, 0.9755282581475768211, 1.000000000000000000, 0.9510565162951535312, 1.000000000000000000, 0.9510565162951535312, 1.000000000000000000, 0.9510565162951535312, 1.000000000000000000, 0.9510565162951535312, 1.000000000000000000, 0.9755282581475768211, 0.9755282581475768211 ) ) 
 REPRESENTATION_ITEM ( '' )  );
#8801 = CARTESIAN_POINT ( 'NONE',  ( -10.37757302488624411, 24.97500000273117493, -31.93888565452638417 ) ) ;
#8802 = CARTESIAN_POINT ( 'NONE',  ( 4.635254915624212657, 76.59999999999999432, 14.26584774442730286 ) ) ;
#8803 = CARTESIAN_POINT ( 'NONE',  ( 6.950374756619257965, 18.01003499907601935, -26.09010956794244507 ) ) ;
#8804 = CARTESIAN_POINT ( 'NONE',  ( -5.147494310547640062, 32.44874571845313227, 32.49999999999992895 ) ) ;
#8805 = CARTESIAN_POINT ( 'NONE',  ( -10.04305231718578462, 34.39999999999998437, 30.90933677959249337 ) ) ;
#8806 = CARTESIAN_POINT ( 'NONE',  ( 26.29305231718579350, 12.79999999999999183, 19.10302069950537529 ) ) ;
#8807 = EDGE_LOOP ( 'NONE', ( #24411, #7448, #8959, #30301 ) ) ;
#8808 = CARTESIAN_POINT ( 'NONE',  ( 7.236395654485760609, 7.524999997268827734, -22.27133577429736633 ) ) ;
#8809 = CARTESIAN_POINT ( 'NONE',  ( -4.300734207923755825, 73.27500000273118985, 13.23629886949340673 ) ) ;
#8810 = CARTESIAN_POINT ( 'NONE',  ( 6.988114217767829928, 40.07291666666666430, -26.07999730980489872 ) ) ;
#8811 = CARTESIAN_POINT ( 'NONE',  ( 33.58253175000000113, 16.12500000273120548, -4.112674001490185761E-15 ) ) ;
#8812 = CARTESIAN_POINT ( 'NONE',  ( 33.58253175000000113, 66.22500000273120691, -10.91162601494193751 ) ) ;
#8813 = CARTESIAN_POINT ( 'NONE',  ( 10.37757302488624056, 32.77500000273118985, -31.93888565452638417 ) ) ;
#8814 = CARTESIAN_POINT ( 'NONE',  ( -27.16883889988624290, 17.17500000273118488, -19.73931689729374028 ) ) ;
#8815 = CARTESIAN_POINT ( 'NONE',  ( -20.75514604977248823, 11.07500000273117990, -28.56700777964554305 ) ) ;
#8816 = CARTESIAN_POINT ( 'NONE',  ( -7.468012846824771955, 13.72434000092397532, -28.02196122052045624 ) ) ;
#8817 = CARTESIAN_POINT ( 'NONE',  ( 20.50609665440969565, 57.54687500000000000, -20.50609665441004736 ) ) ;
#8818 = CARTESIAN_POINT ( 'NONE',  ( -15.00000000000000000, 71.12500000273119838, 0.000000000000000000 ) ) ;
#8819 = CARTESIAN_POINT ( 'NONE',  ( -11.25946833292375793, 75.17500000273119554, -8.180482586598733619 ) ) ;
#8820 = CARTESIAN_POINT ( 'NONE',  ( -10.04305231718579172, 49.60000000000001563, -30.90933677959248982 ) ) ;
#8821 = VECTOR ( 'NONE', #28600, 1000.000000000000000 ) ;
#8822 = FACE_BOUND ( 'NONE', #11917, .T. ) ;
#8823 = CARTESIAN_POINT ( 'NONE',  ( 33.58253175000000113, 52.12500000273118417, -4.112674001490185761E-15 ) ) ;
#8824 = CARTESIAN_POINT ( 'NONE',  ( 23.41746825000000243, 13.02499999726881619, 7.608796670333735079 ) ) ;
#8825 = ADVANCED_FACE ( 'NONE', ( #22434 ), #9561, .T. ) ;
#8826 = ORIENTED_EDGE ( 'NONE', *, *, #1694, .T. ) ;
#8827 = CARTESIAN_POINT ( 'NONE',  ( -10.37757302488624411, 66.97500000273119269, -31.93888565452638417 ) ) ;
#8828 = CARTESIAN_POINT ( 'NONE',  ( -10.37757302488623701, 1.525000002731202731, 31.93888565452638417 ) ) ;
#8829 = CARTESIAN_POINT ( 'NONE',  ( 14.47279130897151767, 6.924999997268805885, -19.92008829642072598 ) ) ;
#8830 = CARTESIAN_POINT ( 'NONE',  ( -19.11951029504763611, 26.32850666759063785, 19.06425588902592239 ) ) ;
#8831 = ADVANCED_FACE ( 'NONE', ( #29982 ), #26404, .T. ) ;
#8832 = ORIENTED_EDGE ( 'NONE', *, *, #20979, .T. ) ;
#8833 = CARTESIAN_POINT ( 'NONE',  ( 33.58253175000000113, 34.12500000273117706, -4.112674001490185761E-15 ) ) ;
#8834 = CARTESIAN_POINT ( 'NONE',  ( -26.29305231718578995, 68.70000000546238539, 19.10302069950538595 ) ) ;
#8835 = ORIENTED_EDGE ( 'NONE', *, *, #16099, .F. ) ;
#8836 = CARTESIAN_POINT ( 'NONE',  ( 26.00068869287367335, 54.82552083333331439, 15.01150461594596308 ) ) ;
#8837 = CARTESIAN_POINT ( 'NONE',  ( -20.75514604977248823, 63.07500000273119412, -28.56700777964554305 ) ) ;
#8838 = CARTESIAN_POINT ( 'NONE',  ( 2.445080149700053643E-15, 74.75000000546239676, 15.00000000000000000 ) ) ;
#8839 = CARTESIAN_POINT ( 'NONE',  ( -27.16883889988624290, 72.92500000273119554, -19.73931689729374028 ) ) ;
#8840 = CARTESIAN_POINT ( 'NONE',  ( -15.01150461594642138, 25.89322916666666430, -26.00068869287340334 ) ) ;
#8841 = CARTESIAN_POINT ( 'NONE',  ( 19.82091636218621034, 3.799999999999998046, 14.40073868116559730 ) ) ;
#8842 = CARTESIAN_POINT ( 'NONE',  ( 0.000000000000000000, 80.00000000000001421, 0.000000000000000000 ) ) ;
#8843 = CARTESIAN_POINT ( 'NONE',  ( 27.16883889988624290, 13.92500000273116889, 19.73931689729373673 ) ) ;
#8844 = CARTESIAN_POINT ( 'NONE',  ( -11.25946833292375793, 73.07500000273120122, 8.180482586598737171 ) ) ;
#8845 = CIRCLE ( 'NONE', #25292, 10.11607355459420177 ) ;
#8846 = CARTESIAN_POINT ( 'NONE',  ( -26.02091320914878025, 41.35638916574269075, -14.97647472619899389 ) ) ;
#8847 = CIRCLE ( 'NONE', #5010, 10.64101615137753676 ) ;
#8848 = CARTESIAN_POINT ( 'NONE',  ( -9.270509831248421762, 78.29999999999999716, 12.75976212528060039 ) ) ;
#8849 = CARTESIAN_POINT ( 'NONE',  ( 7.505752307973351023, 48.38020833333332860, 28.01184896238290278 ) ) ;
#8850 = CARTESIAN_POINT ( 'NONE',  ( -24.50000000000000711, 11.09999999999999787, 7.960532557706201828 ) ) ;
#8851 = CARTESIAN_POINT ( 'NONE',  ( 32.50000000000000000, 49.50000000546239676, -3.980102097228898626E-15 ) ) ;
#8852 = CARTESIAN_POINT ( 'NONE',  ( 6.988114217767829928, 12.57291666666666252, -26.07999730980489872 ) ) ;
#8853 = CARTESIAN_POINT ( 'NONE',  ( 20.75514604977249178, 43.82500000273119412, 28.56700777964553950 ) ) ;
#8854 = CARTESIAN_POINT ( 'NONE',  ( 4.300734207923761154, 73.47500000273116427, 13.23629886949340495 ) ) ;
#8855 = CARTESIAN_POINT ( 'NONE',  ( 33.58253175000000113, 48.37500000273119127, -4.112674001490185761E-15 ) ) ;
#8856 = CARTESIAN_POINT ( 'NONE',  ( -27.16883889988623935, 25.57500000273119056, 19.73931689729374739 ) ) ;
#8857 = CARTESIAN_POINT ( 'NONE',  ( -14.45873412499999944, 80.56250000409679046, 0.000000000000000000 ) ) ;
#8858 = CARTESIAN_POINT ( 'NONE',  ( 27.95245687107223276, 20.16406249999999645, -2.463307335887066074E-13 ) ) ;
#8859 = CARTESIAN_POINT ( 'NONE',  ( 8.891200544363830713E-16, 79.75000000546238255, -15.00000000000000000 ) ) ;
#8860 = CARTESIAN_POINT ( 'NONE',  ( -4.635254915624208216, 80.39999999999997726, 14.26584774442730463 ) ) ;
#8861 = CARTESIAN_POINT ( 'NONE',  ( -26.29305231718578995, 66.19999999999998863, 19.10302069950538595 ) ) ;
#8862 = CARTESIAN_POINT ( 'NONE',  ( 20.75514604977249178, 7.825000002731194115, 28.56700777964553950 ) ) ;
#8863 = CARTESIAN_POINT ( 'NONE',  ( -23.41746825000000243, 3.724999997268820362, 7.608796670333725309 ) ) ;
#8864 = CARTESIAN_POINT ( 'NONE',  ( 28.00173670424535644, 28.89545166574268009, -7.543491769121920321 ) ) ;
#8865 =( BOUNDED_CURVE ( )  B_SPLINE_CURVE ( 2, ( #32471, #1065, #32309, #6061, #4166, #25098, #6735, #24428, #12052, #3660, #8802, #6403, #9137 ),
 .UNSPECIFIED., .F., .T. ) 
 B_SPLINE_CURVE_WITH_KNOTS ( ( 3, 2, 2, 2, 2, 2, 3 ),
 ( 0.4500000000000000111, 0.4600000000000000200, 0.4799999999999999822, 0.5000000000000000000, 0.5200000000000000178, 0.5400000000000000355, 0.5500000000000000444 ),
 .UNSPECIFIED. ) 
 CURVE ( )  GEOMETRIC_REPRESENTATION_ITEM ( )  RATIONAL_B_SPLINE_CURVE ( ( 0.9755282581475768211, 0.9755282581475768211, 1.000000000000000000, 0.9510565162951535312, 1.000000000000000000, 0.9510565162951535312, 1.000000000000000000, 0.9510565162951535312, 1.000000000000000000, 0.9510565162951535312, 1.000000000000000000, 0.9755282581475768211, 0.9755282581475768211 ) ) 
 REPRESENTATION_ITEM ( '' )  );
#8866 = CARTESIAN_POINT ( 'NONE',  ( 1.555960095263670572E-15, 12.50000000000000355, -24.50000000000000000 ) ) ;
#8867 = CARTESIAN_POINT ( 'NONE',  ( 26.09010956794244507, 25.74440999907601935, 6.950374756619249084 ) ) ;
#8868 = CARTESIAN_POINT ( 'NONE',  ( -1.778240108872766143E-15, 54.00000000546237544, -32.49999999999999289 ) ) ;
#8869 = CARTESIAN_POINT ( 'NONE',  ( 33.58253175000000113, 22.12500000273118062, -4.112674001490185761E-15 ) ) ;
#8870 = CARTESIAN_POINT ( 'NONE',  ( 14.47279130897151589, 4.824999997268814234, 19.92008829642072953 ) ) ;
#8871 = CARTESIAN_POINT ( 'NONE',  ( 13.97622843553589966, 50.52864583333333570, -24.20753774853756113 ) ) ;
#8872 = ORIENTED_EDGE ( 'NONE', *, *, #18822, .F. ) ;
#8873 = CARTESIAN_POINT ( 'NONE',  ( 33.58253175000000113, 54.12500000273119838, -4.112674001490185761E-15 ) ) ;
#8874 = CARTESIAN_POINT ( 'NONE',  ( 27.16883889988624290, 28.17500000273119554, 19.73931689729373673 ) ) ;
#8875 = ORIENTED_EDGE ( 'NONE', *, *, #15988, .T. ) ;
#8876 = CARTESIAN_POINT ( 'NONE',  ( -26.00068869287368756, 22.16927083333332504, -15.01150461594595775 ) ) ;
#8877 = CARTESIAN_POINT ( 'NONE',  ( -30.02300923189239867, 19.88319416759064495, -0.04044903254991731589 ) ) ;
#8878 = CARTESIAN_POINT ( 'NONE',  ( -13.91746824999999887, 81.37500000273118417, 0.000000000000000000 ) ) ;
#8879 = CARTESIAN_POINT ( 'NONE',  ( 19.82091636218621034, 17.54999999453762882, 14.40073868116559730 ) ) ;
#8880 = CARTESIAN_POINT ( 'NONE',  ( 23.41746825000000243, 8.724999997268806595, -7.608796670333727974 ) ) ;
#8881 = CARTESIAN_POINT ( 'NONE',  ( 33.58253175000000113, 30.47500000273117493, -10.91162601494193751 ) ) ;
#8882 = CARTESIAN_POINT ( 'NONE',  ( 32.50000000000000000, 31.60000000546237686, -10.55989012756945833 ) ) ;
#8883 = CARTESIAN_POINT ( 'NONE',  ( -32.50000000000000000, 72.00000000000001421, 0.000000000000000000 ) ) ;
#8884 = DIRECTION ( 'NONE',  ( -0.000000000000000000, -1.000000000000000000, -0.000000000000000000 ) ) ;
#8885 = CARTESIAN_POINT ( 'NONE',  ( 12.13525491562421088, 72.79999999999999716, 8.816778784387095058 ) ) ;
#8886 = CARTESIAN_POINT ( 'NONE',  ( -0.04044903254990864921, 60.27381916759065206, 30.02300923189239867 ) ) ;
#8887 = CARTESIAN_POINT ( 'NONE',  ( 33.58253175000000113, 40.37500000273119838, -4.112674001490185761E-15 ) ) ;
#8888 = CARTESIAN_POINT ( 'NONE',  ( -18.94512977948576093, 10.32499999726882400, 13.76444248337722698 ) ) ;
#8889 = CARTESIAN_POINT ( 'NONE',  ( 20.08610463437158344, 14.70000000000000107, 27.64615127144129403 ) ) ;
#8890 = CARTESIAN_POINT ( 'NONE',  ( 24.50000000000000355, 10.10000000000000142, -7.960532557706203605 ) ) ;
#8891 = ADVANCED_FACE ( 'NONE', ( #11797 ), #27418, .T. ) ;
#8892 = CARTESIAN_POINT ( 'NONE',  ( -7.025853678916861966, 41.78607666574268364, -26.06988505166722803 ) ) ;
#8893 = CARTESIAN_POINT ( 'NONE',  ( 6.486482029760649416E-15, 61.62500000273118417, 35.31076352940723240 ) ) ;
#8894 = CARTESIAN_POINT ( 'NONE',  ( -20.75514604977248823, 47.07500000273117280, -28.56700777964554305 ) ) ;
#8895 = CARTESIAN_POINT ( 'NONE',  ( -4.523095164977117273E-15, 8.124999997268826490, 24.62258325217400312 ) ) ;
#8896 = CARTESIAN_POINT ( 'NONE',  ( 3.880418787951139592, 3.301254276084478523, 24.50000000000000000 ) ) ;
#8897 = CARTESIAN_POINT ( 'NONE',  ( 33.58253175000000113, 6.125000002731195714, -4.112674001490185761E-15 ) ) ;
#8898 = CARTESIAN_POINT ( 'NONE',  ( -0.04044903254992426173, 36.21131916759064495, 27.95245687107223276 ) ) ;
#8899 = DIRECTION ( 'NONE',  ( 0.000000000000000000, 0.000000000000000000, 1.000000000000000000 ) ) ;
#8900 = CARTESIAN_POINT ( 'NONE',  ( 19.82091636218621389, 1.949999994537626735, -14.40073868116559197 ) ) ;
#8901 = CARTESIAN_POINT ( 'NONE',  ( -20.75514604977248112, 31.42500000273120619, 28.56700777964554661 ) ) ;
#8902 = CARTESIAN_POINT ( 'NONE',  ( -20.08610463437157989, 56.20000000546238539, -27.64615127144129758 ) ) ;
#8903 = LINE ( 'NONE', #1167, #25408 ) ;
#8904 = CARTESIAN_POINT ( 'NONE',  ( 5.779280353836490358E-15, 60.49999999999998579, 32.49999999999999289 ) ) ;
#8905 = CARTESIAN_POINT ( 'NONE',  ( 28.02196122052058413, 53.24440999907603356, 7.468012846824272799 ) ) ;
#8906 = CARTESIAN_POINT ( 'NONE',  ( -20.08610463437156923, 46.80000000546235839, 27.64615127144130113 ) ) ;
#8907 = CARTESIAN_POINT ( 'NONE',  ( 13.91746824999999887, 72.37500000273116996, -1.704398294459741270E-15 ) ) ;
#8908 = CONICAL_SURFACE ( 'NONE', #33581, 30.00000000000000711, 0.7665918932241471140 ) ;
#8909 = CARTESIAN_POINT ( 'NONE',  ( -24.20753774853730889, 28.47135416666666075, 13.97622843553633842 ) ) ;
#8910 = EDGE_LOOP ( 'NONE', ( #20164, #133, #31042, #47 ) ) ;
#8911 = CIRCLE ( 'NONE', #13317, 1.999999999999993117 ) ;
#8912 = CARTESIAN_POINT ( 'NONE',  ( 20.75514604977248467, 72.42500000273119554, -28.56700777964554305 ) ) ;
#8913 = CARTESIAN_POINT ( 'NONE',  ( -28.01184896238304134, 28.90104166666666785, -7.505752307972844761 ) ) ;
#8914 = CARTESIAN_POINT ( 'NONE',  ( -1.053607264507113999E-13, 64.50000000000000000, 32.50000000000000711 ) ) ;
#8915 = EDGE_LOOP ( 'NONE', ( #19482, #9686, #23244, #18097 ) ) ;
#8916 = CARTESIAN_POINT ( 'NONE',  ( 28.00173670424549499, 45.80767333425730925, 7.543491769121417612 ) ) ;
#8917 = CARTESIAN_POINT ( 'NONE',  ( 26.29305231718579350, 13.30000000546237260, 19.10302069950537529 ) ) ;
#8918 = EDGE_CURVE ( 'NONE', #33879, #17974, #11963, .T. ) ;
#8919 = CARTESIAN_POINT ( 'NONE',  ( 28.01184896238290278, 57.83333333333333570, -7.505752307973347470 ) ) ;
#8920 = CARTESIAN_POINT ( 'NONE',  ( -20.08610463437157989, 64.20000000546238539, -27.64615127144129758 ) ) ;
#8921 = CARTESIAN_POINT ( 'NONE',  ( 10.37757302488624056, 44.77500000273118275, -31.93888565452638417 ) ) ;
#8922 = CARTESIAN_POINT ( 'NONE',  ( -10.04305231718578462, 50.90000000546238113, 30.90933677959249337 ) ) ;
#8923 = CARTESIAN_POINT ( 'NONE',  ( -13.91746824999999887, 73.37500000273116996, 0.000000000000000000 ) ) ;
#8924 = CARTESIAN_POINT ( 'NONE',  ( -2.162160676586881955E-15, 38.62500000273118417, -35.31076352940723240 ) ) ;
#8925 = CARTESIAN_POINT ( 'NONE',  ( -32.50000000000000000, 62.50000000546239676, 0.000000000000000000 ) ) ;
#8926 = CARTESIAN_POINT ( 'NONE',  ( -27.16883889988623935, 63.57500000273119412, 19.73931689729374739 ) ) ;
#8927 = DIRECTION ( 'NONE',  ( 0.000000000000000000, 0.000000000000000000, 1.000000000000000000 ) ) ;
#8928 = EDGE_CURVE ( 'NONE', #9120, #10039, #19011, .T. ) ;
#8929 = CARTESIAN_POINT ( 'NONE',  ( 26.29305231718579350, 36.79999999999998295, 19.10302069950537529 ) ) ;
#8930 = CARTESIAN_POINT ( 'NONE',  ( -26.29305231718579350, 35.79999999999999716, -19.10302069950537884 ) ) ;
#8931 = CARTESIAN_POINT ( 'NONE',  ( -23.41746824999999887, 13.62499999726882116, -2.867812753649727150E-15 ) ) ;
#8932 = CARTESIAN_POINT ( 'NONE',  ( -20.75514604977248112, 5.675000002731203530, 28.56700777964554661 ) ) ;
#8933 = VECTOR ( 'NONE', #12590, 1000.000000000000000 ) ;
#8934 = CARTESIAN_POINT ( 'NONE',  ( 1.836970198721029589E-15, 82.00000000000001421, 15.00000000000000000 ) ) ;
#8935 = CARTESIAN_POINT ( 'NONE',  ( 8.601468415847520532, 80.07500000273121543, 11.83890561707634603 ) ) ;
#8936 = CARTESIAN_POINT ( 'NONE',  ( -33.58253175000000113, 69.47500000273117848, 10.91162601494193929 ) ) ;
#8937 = CARTESIAN_POINT ( 'NONE',  ( -7.570916362186215665, 5.399999999999987921, 23.30088464923126423 ) ) ;
#8938 = CONICAL_SURFACE ( 'NONE', #17725, 32.63512777199724724, 0.7853981633974471688 ) ;
#8939 = EDGE_CURVE ( 'NONE', #12256, #2384, #9769, .T. ) ;
#8940 = CARTESIAN_POINT ( 'NONE',  ( 33.58253175000000113, 70.47500000273117848, -10.91162601494193751 ) ) ;
#8941 = ORIENTED_EDGE ( 'NONE', *, *, #33353, .F. ) ;
#8942 = CARTESIAN_POINT ( 'NONE',  ( -24.50000000000000355, 6.649999994537636461, -7.960532557706207157 ) ) ;
#8943 = CARTESIAN_POINT ( 'NONE',  ( -24.20753774853730889, 66.28385416666662877, 13.97622843553633842 ) ) ;
#8944 = CARTESIAN_POINT ( 'NONE',  ( -11.54700538379251817, 96.00000000000002842, 19.99999999999999645 ) ) ;
#8945 = CARTESIAN_POINT ( 'NONE',  ( -20.75514604977248823, 46.82500000273117990, -28.56700777964554305 ) ) ;
#8946 = CARTESIAN_POINT ( 'NONE',  ( -33.58253175000000113, 9.275000002731177418, -10.91162601494193218 ) ) ;
#8947 = CARTESIAN_POINT ( 'NONE',  ( 6.486482029760648627E-15, 59.87500000273118417, 35.31076352940722529 ) ) ;
#8948 = CARTESIAN_POINT ( 'NONE',  ( 24.20753774853731244, 47.37760416666666430, -13.97622843553633132 ) ) ;
#8949 = CARTESIAN_POINT ( 'NONE',  ( 7.468012846824777284, 36.06809000092397355, 28.02196122052045268 ) ) ;
#8950 = CARTESIAN_POINT ( 'NONE',  ( -15.04653450569338524, 24.45534749907602290, -25.98046417659831775 ) ) ;
#8951 = CARTESIAN_POINT ( 'NONE',  ( 10.04305231718579705, 69.10000000546239107, 30.90933677959248982 ) ) ;
#8952 = CARTESIAN_POINT ( 'NONE',  ( -4.300734207923759378, 80.47500000273116427, -13.23629886949340495 ) ) ;
#8953 = CARTESIAN_POINT ( 'NONE',  ( 7.025853678916867295, 57.25482666574269075, 26.06988505166722803 ) ) ;
#8954 = CYLINDRICAL_SURFACE ( 'NONE', #8351, 30.00000000000004974 ) ;
#8955 = CARTESIAN_POINT ( 'NONE',  ( -15.14183272437242778, 5.049999994537627934, 20.84094480462497856 ) ) ;
#8956 = VERTEX_POINT ( 'NONE', #24670 ) ;
#8957 = CARTESIAN_POINT ( 'NONE',  ( 27.16883889988624290, 40.17500000273120975, 19.73931689729373673 ) ) ;
#8958 = CARTESIAN_POINT ( 'NONE',  ( 26.29305231718579350, 27.30000000546238681, 19.10302069950537529 ) ) ;
#8959 = ORIENTED_EDGE ( 'NONE', *, *, #20203, .T. ) ;
#8960 = CARTESIAN_POINT ( 'NONE',  ( 10.37757302488624767, 15.72500000273117848, 31.93888565452638417 ) ) ;
#8961 = CARTESIAN_POINT ( 'NONE',  ( 30.02300923189239512, 33.91406249999997158, -2.619432448724977703E-13 ) ) ;
#8962 = ORIENTED_EDGE ( 'NONE', *, *, #5665, .T. ) ;
#8963 =( BOUNDED_CURVE ( )  B_SPLINE_CURVE ( 2, ( #17878, #22211, #2071, #9973, #32488, #3842, #31070, #30724, #28331, #27991, #7566, #17703, #28162 ),
 .UNSPECIFIED., .F., .T. ) 
 B_SPLINE_CURVE_WITH_KNOTS ( ( 3, 2, 2, 2, 2, 2, 3 ),
 ( 0.3055555555555555802, 0.3111111111111111160, 0.3222222222222222432, 0.3333333333333333148, 0.3444444444444444420, 0.3555555555555555691, 0.3611111111111111049 ),
 .UNSPECIFIED. ) 
 CURVE ( )  GEOMETRIC_REPRESENTATION_ITEM ( )  RATIONAL_B_SPLINE_CURVE ( ( 0.9755282581475767101, 0.9755282581475768211, 1.000000000000000000, 0.9510565162951535312, 1.000000000000000000, 0.9510565162951535312, 1.000000000000000000, 0.9510565162951535312, 1.000000000000000000, 0.9510565162951535312, 1.000000000000000000, 0.9755282581475768211, 0.9755282581475768211 ) ) 
 REPRESENTATION_ITEM ( '' )  );
#8964 = CARTESIAN_POINT ( 'NONE',  ( -5.147494310547423346, 74.94874572391552192, 32.50000000000000000 ) ) ;
#8965 = CARTESIAN_POINT ( 'NONE',  ( -20.75514604977248823, 54.82500000273118701, -28.56700777964554305 ) ) ;
#8966 = CARTESIAN_POINT ( 'NONE',  ( 20.50609665441005092, 58.40625000000000711, 20.50609665440969209 ) ) ;
#8967 = CARTESIAN_POINT ( 'NONE',  ( 10.04305231718579705, 11.10000000546237864, 30.90933677959248982 ) ) ;
#8968 = LINE ( 'NONE', #26671, #3719 ) ;
#8969 = CARTESIAN_POINT ( 'NONE',  ( -23.41746824999999887, 18.12499999726882649, -2.867812753649727150E-15 ) ) ;
#8970 = CARTESIAN_POINT ( 'NONE',  ( 20.08610463437158344, 56.69999999999998153, 27.64615127144129403 ) ) ;
#8971 = CARTESIAN_POINT ( 'NONE',  ( 20.75514604977249178, 22.07500000273117990, 28.56700777964553950 ) ) ;
#8972 = CARTESIAN_POINT ( 'NONE',  ( 26.29305231718579350, 5.300000005462379704, 19.10302069950537529 ) ) ;
#8973 = CARTESIAN_POINT ( 'NONE',  ( -20.53372385742107653, 68.99961833240934084, -20.47846945139867003 ) ) ;
#8974 = CARTESIAN_POINT ( 'NONE',  ( 13.91746824999999532, 73.97500000273119269, -4.522059556121118540 ) ) ;
#8975 = CARTESIAN_POINT ( 'NONE',  ( 7.570916362186207671, 15.60000000000000320, 23.30088464923126779 ) ) ;
#8976 = CARTESIAN_POINT ( 'NONE',  ( -5.147494310547430452, 33.55125428154685352, -32.49999999999999289 ) ) ;
#8977 = CARTESIAN_POINT ( 'NONE',  ( -20.08610463437156923, 12.29999999999999183, 27.64615127144130113 ) ) ;
#8978 = ORIENTED_EDGE ( 'NONE', *, *, #24561, .F. ) ;
#8979 = CARTESIAN_POINT ( 'NONE',  ( -7.236395654485757944, 7.724999997268805707, -22.27133577429736988 ) ) ;
#8980 = CARTESIAN_POINT ( 'NONE',  ( 2.688165632520823219E-15, 77.37500000273118417, 14.63369212191046387 ) ) ;
#8981 = CARTESIAN_POINT ( 'NONE',  ( -24.20753774853756823, 39.35677083333331439, -13.97622843553588723 ) ) ;
#8982 = CARTESIAN_POINT ( 'NONE',  ( 20.75514604977249178, 19.82500000273119412, 28.56700777964553950 ) ) ;
#8983 = CARTESIAN_POINT ( 'NONE',  ( 10.37757302488624056, 64.52500000273118985, -31.93888565452638417 ) ) ;
#8984 = CARTESIAN_POINT ( 'NONE',  ( 33.58253175000000823, 28.27500000273118985, 10.91162601494192863 ) ) ;
#8985 = VECTOR ( 'NONE', #12938, 1000.000000000000000 ) ;
#8986 = CARTESIAN_POINT ( 'NONE',  ( 33.58253175000000823, 14.27500000273119340, 10.91162601494192863 ) ) ;
#8987 = CARTESIAN_POINT ( 'NONE',  ( -33.58253175000000113, 11.47500000273119447, 10.91162601494193929 ) ) ;
#8988 = CARTESIAN_POINT ( 'NONE',  ( 15.04653450569292872, 14.15402750092397532, -25.98046417659857710 ) ) ;
#8989 = CARTESIAN_POINT ( 'NONE',  ( -30.02300923189239512, 56.25781249999997868, 2.654126918244515359E-13 ) ) ;
#8990 = CARTESIAN_POINT ( 'NONE',  ( 32.63512777199724724, -24.47487373415290790, 3.996650476574133167E-15 ) ) ;
#8991 = CARTESIAN_POINT ( 'NONE',  ( -11.25946833292375793, 79.17500000273119554, -8.180482586598733619 ) ) ;
#8992 = CARTESIAN_POINT ( 'NONE',  ( -20.08610463437156923, 50.30000000000001137, 27.64615127144130113 ) ) ;
#8993 = CARTESIAN_POINT ( 'NONE',  ( 32.50000000000000711, 57.40000000546237402, 10.55989012756945122 ) ) ;
#8994 = CARTESIAN_POINT ( 'NONE',  ( -20.75514604977248823, 50.82500000273117280, -28.56700777964554305 ) ) ;
#8995 = CARTESIAN_POINT ( 'NONE',  ( 14.47279130897151767, 17.42499999726882365, -19.92008829642072598 ) ) ;
#8996 = ORIENTED_EDGE ( 'NONE', *, *, #1791, .T. ) ;
#8997 = CARTESIAN_POINT ( 'NONE',  ( 33.58253175000000113, 62.47500000273118559, -10.91162601494193751 ) ) ;
#8998 = DIRECTION ( 'NONE',  ( 0.000000000000000000, 0.000000000000000000, -1.000000000000000000 ) ) ;
#8999 = CARTESIAN_POINT ( 'NONE',  ( -23.41746824999999887, 3.624999997268813168, -2.867812753649727150E-15 ) ) ;
#9000 = CARTESIAN_POINT ( 'NONE',  ( -14.01125832528285109, 22.74777750092397355, 24.18731323226248264 ) ) ;
#9001 = VERTEX_POINT ( 'NONE', #4412 ) ;
#9002 = CARTESIAN_POINT ( 'NONE',  ( -27.16883889988624290, 36.92500000273117422, -19.73931689729374028 ) ) ;
#9003 = CARTESIAN_POINT ( 'NONE',  ( 24.50000000000000000, 6.000000000000005329, 0.000000000000000000 ) ) ;
#9004 = STYLED_ITEM ( 'NONE', ( #20945 ), #18554 ) ;
#9005 = VERTEX_POINT ( 'NONE', #3908 ) ;
#9006 = CARTESIAN_POINT ( 'NONE',  ( 28.01184896238304134, 47.80729166666666430, 7.505752307972846538 ) ) ;
#9007 = CARTESIAN_POINT ( 'NONE',  ( -33.58253175000000113, 61.37500000273119127, 0.000000000000000000 ) ) ;
#9008 = CARTESIAN_POINT ( 'NONE',  ( 6.277390505771533514E-15, 1.000000005462384323, 34.17252228774368916 ) ) ;
#9009 = CARTESIAN_POINT ( 'NONE',  ( 10.37757302488624767, 73.72500000273119269, 31.93888565452638417 ) ) ;
#9010 = CARTESIAN_POINT ( 'NONE',  ( -2.584737979205441561E-13, 29.61718749999999645, -30.02300923189239512 ) ) ;
#9011 = CARTESIAN_POINT ( 'NONE',  ( 24.50000000000000355, 5.899999999999987921, 7.960532557706212486 ) ) ;
#9012 = CARTESIAN_POINT ( 'NONE',  ( -20.75514604977248112, 5.675000002731203530, 28.56700777964554661 ) ) ;
#9013 = CARTESIAN_POINT ( 'NONE',  ( -2.162160676586881955E-15, 14.62500000273118239, -35.31076352940723240 ) ) ;
#9014 = CARTESIAN_POINT ( 'NONE',  ( 30.02300923189239867, 39.35118083240935505, -0.04044903255044467877 ) ) ;
#9015 = CARTESIAN_POINT ( 'NONE',  ( -12.13525491562420910, 80.19999999999998863, 8.816778784387098611 ) ) ;
#9016 = CARTESIAN_POINT ( 'NONE',  ( 15.01150461594643382, 58.54947916666666430, 26.00068869287340334 ) ) ;
#9017 = CARTESIAN_POINT ( 'NONE',  ( -24.50000000000000000, 8.649999994537632020, -7.960532557706207157 ) ) ;
#9018 = CARTESIAN_POINT ( 'NONE',  ( -19.82091636218621034, 8.549999994537621717, -14.40073868116559552 ) ) ;
#9019 = DIRECTION ( 'NONE',  ( 0.000000000000000000, 1.000000000000000000, 0.000000000000000000 ) ) ;
#9020 = CARTESIAN_POINT ( 'NONE',  ( -27.95245687107222921, 18.44531249999999645, 2.498001805406602216E-13 ) ) ;
#9021 = EDGE_CURVE ( 'NONE', #12035, #969, #1144, .T. ) ;
#9022 = CARTESIAN_POINT ( 'NONE',  ( 33.58253175000000113, 40.12500000273119838, -4.112674001490185761E-15 ) ) ;
#9023 = CARTESIAN_POINT ( 'NONE',  ( -8.601468415847518756, 76.57500000273120122, -11.83890561707634781 ) ) ;
#9024 = CARTESIAN_POINT ( 'NONE',  ( -2.162160676586881955E-15, 48.87500000273117706, -35.31076352940723240 ) ) ;
#9025 = CARTESIAN_POINT ( 'NONE',  ( 33.58253175000000113, 30.47500000273117493, -10.91162601494193574 ) ) ;
#9026 = CARTESIAN_POINT ( 'NONE',  ( 15.14183272437242067, 17.69999999999999218, 20.84094480462498211 ) ) ;
#9027 = EDGE_CURVE ( 'NONE', #16413, #30438, #30773, .T. ) ;
#9028 = CARTESIAN_POINT ( 'NONE',  ( 13.97622843553633842, 31.04947916666666430, 24.20753774853730889 ) ) ;
#9029 = CARTESIAN_POINT ( 'NONE',  ( -5.147494310547430452, 17.55125428154684641, -32.49999999999999289 ) ) ;
#9030 = CARTESIAN_POINT ( 'NONE',  ( 9.270509831248425314, 80.69999999999997442, 12.75976212528059683 ) ) ;
#9031 = CARTESIAN_POINT ( 'NONE',  ( 20.08610463437157279, 67.30000000000001137, -27.64615127144129758 ) ) ;
#9032 = CARTESIAN_POINT ( 'NONE',  ( 20.75514604977249178, 9.825000002731188786, 28.56700777964553950 ) ) ;
#9033 = CARTESIAN_POINT ( 'NONE',  ( -14.47279130897151767, 13.32499999726880624, -19.92008829642072598 ) ) ;
#9034 = CARTESIAN_POINT ( 'NONE',  ( 30.02300923189239867, 25.60118083240935860, -0.04044903255044467877 ) ) ;
#9035 = CARTESIAN_POINT ( 'NONE',  ( 0.000000000000000000, 80.00000000000001421, 0.000000000000000000 ) ) ;
#9036 = CARTESIAN_POINT ( 'NONE',  ( -26.09010956794245217, 30.90065999907601579, -6.950374756619243755 ) ) ;
#9037 = CARTESIAN_POINT ( 'NONE',  ( 5.779280353836490358E-15, 60.49999999999998579, 32.49999999999999289 ) ) ;
#9038 = CARTESIAN_POINT ( 'NONE',  ( -20.75514604977248823, 14.82500000273117813, -28.56700777964554305 ) ) ;
#9039 = CARTESIAN_POINT ( 'NONE',  ( 7.236395654485760609, 7.524999997268800200, -22.27133577429736633 ) ) ;
#9040 = CARTESIAN_POINT ( 'NONE',  ( 26.07999730980477437, 54.39583333333332860, -6.988114217768290004 ) ) ;
#9041 = ORIENTED_EDGE ( 'NONE', *, *, #30437, .T. ) ;
#9042 = CARTESIAN_POINT ( 'NONE',  ( -27.16883889988623935, 53.32500000273120122, 19.73931689729374739 ) ) ;
#9043 = CARTESIAN_POINT ( 'NONE',  ( 20.75514604977248467, 26.67500000273118133, -28.56700777964554305 ) ) ;
#9044 = EDGE_LOOP ( 'NONE', ( #481, #22635, #6478, #9241 ) ) ;
#9045 = CARTESIAN_POINT ( 'NONE',  ( 26.00068869287367335, 23.88802083333331794, 15.01150461594596308 ) ) ;
#9046 = CARTESIAN_POINT ( 'NONE',  ( 0.04044903254992426173, 27.61756916759064140, -30.02300923189239867 ) ) ;
#9047 = LINE ( 'NONE', #11296, #17290 ) ;
#9048 = CARTESIAN_POINT ( 'NONE',  ( 19.82091636218621034, 15.54999999453762705, 14.40073868116559730 ) ) ;
#9049 = CARTESIAN_POINT ( 'NONE',  ( -23.41746825000000243, 5.524999997268821517, -7.608796670333730638 ) ) ;
#9050 = CARTESIAN_POINT ( 'NONE',  ( -27.16883889988624290, 23.17500000273120619, -19.73931689729374028 ) ) ;
#9051 = CARTESIAN_POINT ( 'NONE',  ( 32.50000000000000000, 31.50000000546238255, -3.980102097228898626E-15 ) ) ;
#9052 = CARTESIAN_POINT ( 'NONE',  ( -20.08610463437157989, 69.69999999999997442, -27.64615127144129758 ) ) ;
#9053 = CARTESIAN_POINT ( 'NONE',  ( -5.147494310547430452, 6.051254287009219190, -32.49999999999999289 ) ) ;
#9054 = CARTESIAN_POINT ( 'NONE',  ( -19.82091636218621034, 10.80000000000000426, -14.40073868116559552 ) ) ;
#9055 = CARTESIAN_POINT ( 'NONE',  ( -20.47846945139902175, 58.12538166759063785, -20.53372385742072481 ) ) ;
#9056 = CARTESIAN_POINT ( 'NONE',  ( 27.16883889988623935, 38.57500000273117280, -19.73931689729374384 ) ) ;
#9057 = CARTESIAN_POINT ( 'NONE',  ( -2.162160676586882350E-15, 56.62500000273116996, -35.31076352940722529 ) ) ;
#9058 = CARTESIAN_POINT ( 'NONE',  ( 26.00068869287367690, 34.20052083333332149, 15.01150461594596486 ) ) ;
#9059 = CARTESIAN_POINT ( 'NONE',  ( 7.236395654485760609, 13.52499999726880553, -22.27133577429736633 ) ) ;
#9060 = CARTESIAN_POINT ( 'NONE',  ( -26.29305231718579350, 11.80000000000000426, -19.10302069950537884 ) ) ;
#9061 = CARTESIAN_POINT ( 'NONE',  ( -24.50000000000000355, 12.90000000000000036, -7.960532557706207157 ) ) ;
#9062 = CARTESIAN_POINT ( 'NONE',  ( 27.95245687107223276, 46.22618083240936215, -0.04044903255042905932 ) ) ;
#9063 = CARTESIAN_POINT ( 'NONE',  ( -20.75514604977248112, 57.42500000273118843, 28.56700777964554661 ) ) ;
#9064 = CARTESIAN_POINT ( 'NONE',  ( -10.37757302488624411, 44.97500000273119269, -31.93888565452638417 ) ) ;
#9065 = CARTESIAN_POINT ( 'NONE',  ( -18.94512977948576093, 9.824999997268824004, 13.76444248337722698 ) ) ;
#9066 = CARTESIAN_POINT ( 'NONE',  ( -4.405589869732278832E-13, 32.49999999999997868, 32.50000000000000000 ) ) ;
#9067 = CARTESIAN_POINT ( 'NONE',  ( -2.162160676586881955E-15, 4.625000002731208149, -35.31076352940723240 ) ) ;
#9068 = EDGE_CURVE ( 'NONE', #12231, #28463, #11073, .T. ) ;
#9069 = CARTESIAN_POINT ( 'NONE',  ( 13.94119854578937812, 35.92486083425730214, 24.22776226481240514 ) ) ;
#9070 = CARTESIAN_POINT ( 'NONE',  ( 12.40046052489741157, 16.99999999999998579, -19.87944187943455177 ) ) ;
#9071 = DIRECTION ( 'NONE',  ( -1.224646799147353454E-16, 1.000000000000000000, -0.000000000000000000 ) ) ;
#9072 = CARTESIAN_POINT ( 'NONE',  ( -27.16883889988623935, 25.32500000273117635, 19.73931689729374739 ) ) ;
#9073 = CARTESIAN_POINT ( 'NONE',  ( 1.093617666956751375E-13, 67.50000000000001421, -32.50000000000000711 ) ) ;
#9074 = DIRECTION ( 'NONE',  ( -0.000000000000000000, -1.000000000000000000, -0.000000000000000000 ) ) ;
#9075 = CARTESIAN_POINT ( 'NONE',  ( -20.08610463437157989, 30.20000000546236407, -27.64615127144129758 ) ) ;
#9076 = CARTESIAN_POINT ( 'NONE',  ( -7.543491769121917656, 52.09857666574269075, -28.00173670424536354 ) ) ;
#9077 = CARTESIAN_POINT ( 'NONE',  ( -26.29305231718578995, 46.70000000546238539, 19.10302069950538595 ) ) ;
#9078 = CARTESIAN_POINT ( 'NONE',  ( 20.75514604977248467, 38.42500000273118133, -28.56700777964554305 ) ) ;
#9079 = CARTESIAN_POINT ( 'NONE',  ( -24.20753774853730889, 21.59635416666666785, 13.97622843553633842 ) ) ;
#9080 = EDGE_CURVE ( 'NONE', #23590, #27495, #5582, .T. ) ;
#9081 = CARTESIAN_POINT ( 'NONE',  ( 20.75514604977249178, 75.82500000273118701, 28.56700777964553950 ) ) ;
#9082 = CARTESIAN_POINT ( 'NONE',  ( 2.740863092043355209E-13, 31.33593749999999289, 30.02300923189239512 ) ) ;
#9083 = DIRECTION ( 'NONE',  ( 0.000000000000000000, 0.000000000000000000, -1.000000000000000000 ) ) ;
#9084 = VERTEX_POINT ( 'NONE', #33409 ) ;
#9085 = CARTESIAN_POINT ( 'NONE',  ( -20.53372385742071771, 53.82850666759064495, 20.47846945139902530 ) ) ;
#9086 = CIRCLE ( 'NONE', #28279, 2.000000000000013767 ) ;
#9087 = CARTESIAN_POINT ( 'NONE',  ( 32.50000000000000000, 13.60000000546239285, -10.55989012756945833 ) ) ;
#9088 = CARTESIAN_POINT ( 'NONE',  ( -26.00068869287340334, 62.84635416666667851, 15.01150461594643382 ) ) ;
#9089 = CARTESIAN_POINT ( 'NONE',  ( 5.147494310547535257, 57.44874571845315359, -32.49999999999996447 ) ) ;
#9090 = CARTESIAN_POINT ( 'NONE',  ( -2.162160676586881955E-15, 42.87500000273119127, -35.31076352940723240 ) ) ;
#9091 = CARTESIAN_POINT ( 'NONE',  ( 10.04305231718578817, 49.90000000546238113, -30.90933677959249337 ) ) ;
#9092 = CARTESIAN_POINT ( 'NONE',  ( 13.91746824999999887, 72.37500000273116996, -1.704398294459741270E-15 ) ) ;
#9093 = CARTESIAN_POINT ( 'NONE',  ( -20.75514604977248823, 30.82500000273119767, -28.56700777964554305 ) ) ;
#9094 = CARTESIAN_POINT ( 'NONE',  ( 19.82091636218621034, 11.80000000000000426, 14.40073868116559730 ) ) ;
#9095 = CARTESIAN_POINT ( 'NONE',  ( 33.58253175000000113, 56.47500000273116427, -10.91162601494193751 ) ) ;
#9096 = SURFACE_STYLE_USAGE ( .BOTH. , #32763 ) ;
#9097 = CARTESIAN_POINT ( 'NONE',  ( -32.50000000000000000, 35.99999999999999289, 0.000000000000000000 ) ) ;
#9098 = CARTESIAN_POINT ( 'NONE',  ( 26.29305231718578995, 33.20000000000000995, -19.10302069950538240 ) ) ;
#9099 = CARTESIAN_POINT ( 'NONE',  ( 23.41746825000000243, 8.524999997268812635, 7.608796670333735079 ) ) ;
#9100 = CARTESIAN_POINT ( 'NONE',  ( 33.58253175000000113, 2.475000002731187809, -10.91162601494193751 ) ) ;
#9101 = CARTESIAN_POINT ( 'NONE',  ( -26.29305231718578995, 70.70000000546239960, 19.10302069950538595 ) ) ;
#9102 = CARTESIAN_POINT ( 'NONE',  ( -13.91746824999999532, 79.47500000273116427, 4.522059556121122093 ) ) ;
#9103 = CARTESIAN_POINT ( 'NONE',  ( 33.58253175000000823, 64.27500000273118985, 10.91162601494192685 ) ) ;
#9104 = CARTESIAN_POINT ( 'NONE',  ( 19.82091636218621389, 3.949999994537628289, -14.40073868116559197 ) ) ;
#9105 = EDGE_LOOP ( 'NONE', ( #28929, #15140, #32299, #9590 ) ) ;
#9106 = CARTESIAN_POINT ( 'NONE',  ( -4.732186688966233175E-15, 3.249999994537627224, 25.76082449383753925 ) ) ;
#9107 = CARTESIAN_POINT ( 'NONE',  ( -26.09010956794232428, 12.86496500092397710, 6.950374756619732253 ) ) ;
#9108 = CARTESIAN_POINT ( 'NONE',  ( 12.13525491562420910, 75.19999999999998863, -8.816778784387098611 ) ) ;
#9109 = CARTESIAN_POINT ( 'NONE',  ( 33.58253175000000823, 46.02500000273118275, 10.91162601494192863 ) ) ;
#9110 = CARTESIAN_POINT ( 'NONE',  ( 33.58253175000000113, 2.475000002731187809, -10.91162601494193751 ) ) ;
#9111 = CARTESIAN_POINT ( 'NONE',  ( 6.486482029760648627E-15, 63.87500000273119127, 35.31076352940722529 ) ) ;
#9112 = CARTESIAN_POINT ( 'NONE',  ( -26.07999730980490583, 49.52604166666666430, -6.988114217767815717 ) ) ;
#9113 = CARTESIAN_POINT ( 'NONE',  ( -28.00173670424549499, 37.21392333425730214, -7.543491769121417612 ) ) ;
#9114 = CARTESIAN_POINT ( 'NONE',  ( -15.04653450569338524, 31.33034749907602290, -25.98046417659831775 ) ) ;
#9115 = CARTESIAN_POINT ( 'NONE',  ( 10.04305231718579705, 65.10000000546239107, 30.90933677959248982 ) ) ;
#9116 = CARTESIAN_POINT ( 'NONE',  ( -13.91746824999999532, 76.77500000273118985, -4.522059556121115875 ) ) ;
#9117 = CARTESIAN_POINT ( 'NONE',  ( -24.18731323226221974, 54.53347249907601935, 14.01125832528330406 ) ) ;
#9118 = CARTESIAN_POINT ( 'NONE',  ( 1.076200423132605543E-16, 52.00000000000000711, -46.18802153517007980 ) ) ;
#9119 = CARTESIAN_POINT ( 'NONE',  ( 5.147494310547643614, 13.94874572391553080, -32.49999999999992895 ) ) ;
#9120 = VERTEX_POINT ( 'NONE', #12648 ) ;
#9121 = CARTESIAN_POINT ( 'NONE',  ( 33.58253175000000823, 44.27500000273120406, 10.91162601494192863 ) ) ;
#9122 = CARTESIAN_POINT ( 'NONE',  ( -32.50000000000000000, 76.10000000000000853, 10.55989012756946366 ) ) ;
#9123 = CARTESIAN_POINT ( 'NONE',  ( 32.50000000000000000, 31.60000000546237686, -10.55989012756945833 ) ) ;
#9124 = ORIENTED_EDGE ( 'NONE', *, *, #27744, .F. ) ;
#9125 = CARTESIAN_POINT ( 'NONE',  ( -7.505752307972844761, 38.35416666666666430, 28.01184896238304134 ) ) ;
#9126 = ORIENTED_EDGE ( 'NONE', *, *, #24474, .F. ) ;
#9127 = EDGE_LOOP ( 'NONE', ( #8502, #3832 ) ) ;
#9128 = CARTESIAN_POINT ( 'NONE',  ( 4.445600272181915325E-13, 27.50000000000000355, -32.50000000000000000 ) ) ;
#9129 = CARTESIAN_POINT ( 'NONE',  ( 33.58253175000000113, 48.12500000273117706, -4.112674001490185761E-15 ) ) ;
#9130 = CARTESIAN_POINT ( 'NONE',  ( 26.00068869287367335, 58.26302083333332149, 15.01150461594596308 ) ) ;
#9131 = CARTESIAN_POINT ( 'NONE',  ( -20.08610463437156923, 8.800000005462372599, 27.64615127144130113 ) ) ;
#9132 = LINE ( 'NONE', #29232, #2628 ) ;
#9133 = AXIS2_PLACEMENT_3D ( 'NONE', #22331, #18929, #16352 ) ;
#9134 = CARTESIAN_POINT ( 'NONE',  ( -18.94512977948575738, 13.92499999726881654, -13.76444248337723231 ) ) ;
#9135 = CARTESIAN_POINT ( 'NONE',  ( 32.50000000000000000, 55.09999999999998010, -10.55989012756945833 ) ) ;
#9136 = CARTESIAN_POINT ( 'NONE',  ( -33.58253175000000113, 23.47500000273119269, 10.91162601494193929 ) ) ;
#9137 = CARTESIAN_POINT ( 'NONE',  ( 2.445080149700053643E-15, 76.49999999999998579, 15.00000000000000000 ) ) ;
#9138 = CARTESIAN_POINT ( 'NONE',  ( 19.06425588902558133, 18.29649333240935150, -19.11951029504797006 ) ) ;
#9139 = CARTESIAN_POINT ( 'NONE',  ( -4.300734207923759378, 72.47500000273119269, -13.23629886949340495 ) ) ;
#9140 = CARTESIAN_POINT ( 'NONE',  ( -20.08610463437156923, 34.29999999999999005, 27.64615127144130113 ) ) ;
#9141 = CARTESIAN_POINT ( 'NONE',  ( -2.092463501923844636E-15, 3.500000000000005329, -34.17252228774368916 ) ) ;
#9142 = ORIENTED_EDGE ( 'NONE', *, *, #18822, .T. ) ;
#9143 = CARTESIAN_POINT ( 'NONE',  ( -23.41746825000000243, 10.02499999726882507, -7.608796670333730638 ) ) ;
#9144 = FACE_OUTER_BOUND ( 'NONE', #17034, .T. ) ;
#9145 = CARTESIAN_POINT ( 'NONE',  ( 6.988114217768294445, 38.06770833333332860, 26.07999730980477437 ) ) ;
#9146 = ADVANCED_FACE ( 'NONE', ( #20383, #9730 ), #17636, .F. ) ;
#9147 = CARTESIAN_POINT ( 'NONE',  ( 33.58253175000000113, 64.12500000273118417, -4.112674001490185761E-15 ) ) ;
#9148 = CARTESIAN_POINT ( 'NONE',  ( -27.16883889988623935, 27.57500000273117990, 19.73931689729374739 ) ) ;
#9149 = CARTESIAN_POINT ( 'NONE',  ( 20.75514604977249178, 16.07500000273119412, 28.56700777964553950 ) ) ;
#9150 = CARTESIAN_POINT ( 'NONE',  ( 33.58253175000000823, 8.275000002731179194, 10.91162601494192685 ) ) ;
#9151 = CARTESIAN_POINT ( 'NONE',  ( 26.09010956794232428, 62.70871500092398065, -6.950374756619718042 ) ) ;
#9152 = CARTESIAN_POINT ( 'NONE',  ( 15.01150461594643204, 51.67447916666665719, 26.00068869287340334 ) ) ;
#9153 = CARTESIAN_POINT ( 'NONE',  ( -11.25946833292375793, 80.67500000273119554, -8.180482586598733619 ) ) ;
#9154 = CARTESIAN_POINT ( 'NONE',  ( -13.91746824999999532, 79.27500000273120406, -4.522059556121115875 ) ) ;
#9155 = CARTESIAN_POINT ( 'NONE',  ( -32.50000000000000000, 48.09999999999999432, 10.55989012756946366 ) ) ;
#9156 = SURFACE_SIDE_STYLE ('',( #22214 ) ) ;
#9157 = CARTESIAN_POINT ( 'NONE',  ( 10.37757302488624056, 54.52500000273119696, -31.93888565452638417 ) ) ;
#9158 = CARTESIAN_POINT ( 'NONE',  ( -7.236395654485757944, 5.224999997268803043, -22.27133577429736988 ) ) ;
#9159 = ORIENTED_EDGE ( 'NONE', *, *, #27274, .F. ) ;
#9160 = CARTESIAN_POINT ( 'NONE',  ( -27.16883889988624290, 63.17500000273117422, -19.73931689729374028 ) ) ;
#9161 = FACE_OUTER_BOUND ( 'NONE', #27698, .T. ) ;
#9162 = CARTESIAN_POINT ( 'NONE',  ( -23.41746825000000598, 13.72499999726882258, 7.608796670333726198 ) ) ;
#9163 = CARTESIAN_POINT ( 'NONE',  ( -27.95245687107223986, 30.19569416759064140, -0.04044903254993292840 ) ) ;
#9164 = ORIENTED_EDGE ( 'NONE', *, *, #11001, .T. ) ;
#9165 = CARTESIAN_POINT ( 'NONE',  ( -2.162160676586881955E-15, 32.62500000273119838, -35.31076352940723240 ) ) ;
#9166 = CARTESIAN_POINT ( 'NONE',  ( -23.09401076758502924, 86.00000000000001421, 5.354274672883389237E-15 ) ) ;
#9167 = ORIENTED_EDGE ( 'NONE', *, *, #30966, .F. ) ;
#9168 = CARTESIAN_POINT ( 'NONE',  ( -2.584737979205441561E-13, 60.55468749999999289, -30.02300923189239512 ) ) ;
#9169 = CARTESIAN_POINT ( 'NONE',  ( 27.16883889988624290, 58.17500000273118133, 19.73931689729373673 ) ) ;
#9170 = CARTESIAN_POINT ( 'NONE',  ( 32.50000000000000000, 69.50000000546238255, -3.980102097228898626E-15 ) ) ;
#9171 = CARTESIAN_POINT ( 'NONE',  ( -2.162160676586881955E-15, 76.62500000273118417, -35.31076352940723240 ) ) ;
#9172 = CARTESIAN_POINT ( 'NONE',  ( 26.00068869287367335, 34.20052083333332860, 15.01150461594596308 ) ) ;
#9173 = CARTESIAN_POINT ( 'NONE',  ( 7.570916362186213000, 4.399999999999987033, -23.30088464923126423 ) ) ;
#9174 = CARTESIAN_POINT ( 'NONE',  ( -20.75514604977248823, 5.075000002731193227, -28.56700777964554305 ) ) ;
#9175 = CARTESIAN_POINT ( 'NONE',  ( 27.16883889988624290, 17.92500000273117422, 19.73931689729373673 ) ) ;
#9176 = CARTESIAN_POINT ( 'NONE',  ( 2.688165632520823219E-15, 75.37500000273118417, 14.63369212191046209 ) ) ;
#9177 = CARTESIAN_POINT ( 'NONE',  ( 7.468012846824281681, 45.51003499907601935, -28.02196122052058058 ) ) ;
#9178 = CARTESIAN_POINT ( 'NONE',  ( -9.657523855033125146E-16, 79.49999999999998579, -15.77193336357400710 ) ) ;
#9179 = CARTESIAN_POINT ( 'NONE',  ( 15.01150461594596486, 53.96614583333333570, -26.00068869287367690 ) ) ;
#9180 = CARTESIAN_POINT ( 'NONE',  ( -3.880418787951124493, 9.198745712990794132, 24.50000000000000355 ) ) ;
#9181 = CARTESIAN_POINT ( 'NONE',  ( 7.570916362186207671, 7.349999994537615322, 23.30088464923126779 ) ) ;
#9182 = CARTESIAN_POINT ( 'NONE',  ( 15.00000000000000355, 79.15000000546238823, 4.873795443493592394 ) ) ;
#9183 = CARTESIAN_POINT ( 'NONE',  ( -6.950374756619247307, 67.85378499907602645, 26.09010956794245217 ) ) ;
#9184 = CARTESIAN_POINT ( 'NONE',  ( 33.58253175000000823, 36.02500000273117564, 10.91162601494192863 ) ) ;
#9185 = CARTESIAN_POINT ( 'NONE',  ( -4.300734207923759378, 72.47500000273116427, -13.23629886949340495 ) ) ;
#9186 = CARTESIAN_POINT ( 'NONE',  ( -20.75514604977248112, 47.67500000273118843, 28.56700777964554661 ) ) ;
#9187 = CARTESIAN_POINT ( 'NONE',  ( -2.162160676586882350E-15, 28.87500000273119838, -35.31076352940722529 ) ) ;
#9188 = DIRECTION ( 'NONE',  ( 0.000000000000000000, -1.000000000000000000, 0.000000000000000000 ) ) ;
#9189 = CARTESIAN_POINT ( 'NONE',  ( 24.20753774853756113, 34.20052083333332149, 13.97622843553589789 ) ) ;
#9190 = AXIS2_PLACEMENT_3D ( 'NONE', #30500, #25023, #27431 ) ;
#9191 = CARTESIAN_POINT ( 'NONE',  ( 10.04305231718578817, 69.40000000000000568, -30.90933677959249337 ) ) ;
#9192 = CARTESIAN_POINT ( 'NONE',  ( 18.94512977948576093, 12.82499999726882578, -13.76444248337722875 ) ) ;
#9193 = CARTESIAN_POINT ( 'NONE',  ( -14.97647472619899389, 26.74701416574268720, 26.02091320914878025 ) ) ;
#9194 = CARTESIAN_POINT ( 'NONE',  ( 18.94512977948576093, 1.324999997268816454, -13.76444248337722875 ) ) ;
#9195 = CARTESIAN_POINT ( 'NONE',  ( -24.18731323226221974, 37.34597249907603356, 14.01125832528330406 ) ) ;
#9196 = FACE_OUTER_BOUND ( 'NONE', #15740, .T. ) ;
#9197 = CARTESIAN_POINT ( 'NONE',  ( -2.162160676586882350E-15, 14.62500000273118239, -35.31076352940722529 ) ) ;
#9198 = CARTESIAN_POINT ( 'NONE',  ( -14.47279130897152122, 6.424999997268821872, 19.92008829642072243 ) ) ;
#9199 = CARTESIAN_POINT ( 'NONE',  ( 13.97622843553633665, 61.98697916666665009, 24.20753774853730889 ) ) ;
#9200 = EDGE_LOOP ( 'NONE', ( #6213, #12162 ) ) ;
#9201 = CARTESIAN_POINT ( 'NONE',  ( -2.162160676586881955E-15, 52.62500000273117706, -35.31076352940723240 ) ) ;
#9202 = CARTESIAN_POINT ( 'NONE',  ( 20.75514604977248467, 20.67500000273119909, -28.56700777964554305 ) ) ;
#9203 = EDGE_CURVE ( 'NONE', #3689, #3815, #8667, .T. ) ;
#9204 = ORIENTED_EDGE ( 'NONE', *, *, #1168, .F. ) ;
#9205 = CARTESIAN_POINT ( 'NONE',  ( 28.01184896238290278, 23.45833333333333215, -7.505752307973347470 ) ) ;
#9206 = CARTESIAN_POINT ( 'NONE',  ( 7.543491769121427382, 27.76079833425730925, -28.00173670424548433 ) ) ;
#9207 = CARTESIAN_POINT ( 'NONE',  ( -10.04305231718578462, 72.90000000546237402, 30.90933677959249337 ) ) ;
#9208 = CARTESIAN_POINT ( 'NONE',  ( -19.82091636218621389, 16.94999999453761319, 14.40073868116558842 ) ) ;
#9209 = EDGE_CURVE ( 'NONE', #3518, #14369, #4052, .T. ) ;
#9210 = CARTESIAN_POINT ( 'NONE',  ( -7.236395654485757944, 5.224999997268803043, -22.27133577429736988 ) ) ;
#9211 = CARTESIAN_POINT ( 'NONE',  ( 33.58253175000000823, 22.27500000273116854, 10.91162601494192863 ) ) ;
#9212 = CARTESIAN_POINT ( 'NONE',  ( 6.277390505771533514E-15, 27.00000000546237899, 34.17252228774368916 ) ) ;
#9213 = CARTESIAN_POINT ( 'NONE',  ( 10.04305231718578817, 75.39999999999999147, -30.90933677959249337 ) ) ;
#9214 = CARTESIAN_POINT ( 'NONE',  ( 5.779280353836490358E-15, 7.000000005462371000, 32.49999999999999289 ) ) ;
#9215 = CARTESIAN_POINT ( 'NONE',  ( -15.00000000000000000, 74.00000000000001421, 0.000000000000000000 ) ) ;
#9216 = CARTESIAN_POINT ( 'NONE',  ( 14.97647472619947351, 56.54986083425731636, 26.02091320914850314 ) ) ;
#9217 = CARTESIAN_POINT ( 'NONE',  ( 27.16883889988623935, 36.57500000273117280, -19.73931689729374384 ) ) ;
#9218 = CARTESIAN_POINT ( 'NONE',  ( 27.16883889988623935, 56.32500000273120122, -19.73931689729374384 ) ) ;
#9219 = CARTESIAN_POINT ( 'NONE',  ( -26.00068869287340334, 28.47135416666666430, 15.01150461594643559 ) ) ;
#9220 = CARTESIAN_POINT ( 'NONE',  ( -7.236395654485757944, 11.72499999726880837, -22.27133577429736988 ) ) ;
#9221 = CARTESIAN_POINT ( 'NONE',  ( 32.50000000000000000, 15.00000000000001421, -3.980102097228898626E-15 ) ) ;
#9222 = CARTESIAN_POINT ( 'NONE',  ( -32.50000000000000000, 51.89999999999998437, -10.55989012756945300 ) ) ;
#9223 = CARTESIAN_POINT ( 'NONE',  ( 26.09010956794244507, 39.49440999907601224, 6.950374756619249084 ) ) ;
#9224 = CARTESIAN_POINT ( 'NONE',  ( -27.16883889988624290, 56.92500000273120975, -19.73931689729374028 ) ) ;
#9225 = CARTESIAN_POINT ( 'NONE',  ( 27.16883889988624290, 50.17500000273117422, 19.73931689729373673 ) ) ;
#9226 = CARTESIAN_POINT ( 'NONE',  ( -23.41746824999999887, 11.62499999726881938, -2.867812753649727150E-15 ) ) ;
#9227 = CARTESIAN_POINT ( 'NONE',  ( -1.778240108872766143E-15, 37.50000000000000000, -32.49999999999999289 ) ) ;
#9228 = CARTESIAN_POINT ( 'NONE',  ( -26.29305231718579350, 5.799999999999999822, -19.10302069950537884 ) ) ;
#9229 = CARTESIAN_POINT ( 'NONE',  ( -24.18731323226248264, 47.66965250092398065, -14.01125832528284931 ) ) ;
#9230 = CARTESIAN_POINT ( 'NONE',  ( 26.29305231718578995, 63.70000000546237118, -19.10302069950538240 ) ) ;
#9231 = CARTESIAN_POINT ( 'NONE',  ( 15.14183272437242422, 4.300000000000009592, -20.84094480462497856 ) ) ;
#9232 = CARTESIAN_POINT ( 'NONE',  ( -27.16883889988624290, 18.92500000273118843, -19.73931689729374028 ) ) ;
#9233 = FACE_OUTER_BOUND ( 'NONE', #7098, .T. ) ;
#9234 = CARTESIAN_POINT ( 'NONE',  ( 0.000000000000000000, -10.99999999999999645, 0.000000000000000000 ) ) ;
#9235 = CARTESIAN_POINT ( 'NONE',  ( 26.29305231718578995, 61.20000000000001705, -19.10302069950538240 ) ) ;
#9236 = CARTESIAN_POINT ( 'NONE',  ( -0.04044903255044120238, 65.99180583240935505, -30.02300923189239867 ) ) ;
#9237 = CARTESIAN_POINT ( 'NONE',  ( -26.29305231718579350, 48.30000000546237970, -19.10302069950537884 ) ) ;
#9238 = CARTESIAN_POINT ( 'NONE',  ( -24.50000000000000000, 16.99999999999998579, -3.000384657911015469E-15 ) ) ;
#9239 = CARTESIAN_POINT ( 'NONE',  ( 6.486482029760648627E-15, 29.62500000273120193, 35.31076352940722529 ) ) ;
#9240 = CARTESIAN_POINT ( 'NONE',  ( -19.09188309203660694, 24.89062500000000000, 19.09188309203694800 ) ) ;
#9241 = ORIENTED_EDGE ( 'NONE', *, *, #26475, .F. ) ;
#9242 = CARTESIAN_POINT ( 'NONE',  ( 33.58253175000000823, 74.02500000273120406, 10.91162601494192863 ) ) ;
#9243 = CARTESIAN_POINT ( 'NONE',  ( -26.00068869287340334, 42.22135416666666430, 15.01150461594643382 ) ) ;
#9244 = EDGE_CURVE ( 'NONE', #29890, #22018, #22779, .T. ) ;
#9245 = PLANE ( 'NONE',  #15191 ) ;
#9246 = ORIENTED_EDGE ( 'NONE', *, *, #28799, .F. ) ;
#9247 = CARTESIAN_POINT ( 'NONE',  ( 30.02300923189239867, 49.10194416759064495, 0.04044903254992252006 ) ) ;
#9248 = CARTESIAN_POINT ( 'NONE',  ( 20.08610463437158344, 11.20000000546238184, 27.64615127144129403 ) ) ;
#9249 = EDGE_CURVE ( 'NONE', #12166, #11992, #14383, .T. ) ;
#9250 = CARTESIAN_POINT ( 'NONE',  ( 30.02300923189239512, 57.97656249999997868, -2.619432448724977703E-13 ) ) ;
#9251 = CARTESIAN_POINT ( 'NONE',  ( 2.205017735002230837E-13, 57.49999999999999289, -32.50000000000000000 ) ) ;
#9252 = CARTESIAN_POINT ( 'NONE',  ( 20.75514604977249178, 40.07500000273118701, 28.56700777964553950 ) ) ;
#9253 = CARTESIAN_POINT ( 'NONE',  ( 32.50000000000000711, 47.40000000546237402, 10.55989012756945122 ) ) ;
#9254 = CARTESIAN_POINT ( 'NONE',  ( -15.00000000000000000, 80.10000000000003695, 4.873795443493597723 ) ) ;
#9255 = CARTESIAN_POINT ( 'NONE',  ( 27.16883889988624290, 27.92500000273118133, 19.73931689729373673 ) ) ;
#9256 = CARTESIAN_POINT ( 'NONE',  ( 10.04305231718578817, 31.90000000546239178, -30.90933677959249337 ) ) ;
#9257 = CARTESIAN_POINT ( 'NONE',  ( 10.37757302488624056, 56.77500000273119696, -31.93888565452638417 ) ) ;
#9258 =( LENGTH_UNIT ( ) NAMED_UNIT ( * ) SI_UNIT ( .MILLI., .METRE. ) );
#9259 = CARTESIAN_POINT ( 'NONE',  ( 10.04305231718579705, 34.60000000000000853, 30.90933677959248982 ) ) ;
#9260 = CARTESIAN_POINT ( 'NONE',  ( -2.092463501923844636E-15, 35.49999999999998579, -34.17252228774368916 ) ) ;
#9261 = CARTESIAN_POINT ( 'NONE',  ( 14.47279130897151589, 10.32499999726881335, 19.92008829642072953 ) ) ;
#9262 = CARTESIAN_POINT ( 'NONE',  ( -27.16883889988624290, 72.92500000273119554, -19.73931689729374028 ) ) ;
#9263 = CARTESIAN_POINT ( 'NONE',  ( -10.04305231718578462, 70.90000000546237402, 30.90933677959249337 ) ) ;
#9264 = CARTESIAN_POINT ( 'NONE',  ( 0.000000000000000000, 0.000000000000000000, 0.000000000000000000 ) ) ;
#9265 = CARTESIAN_POINT ( 'NONE',  ( 20.75514604977249178, 64.07500000273120122, 28.56700777964553950 ) ) ;
#9266 = CARTESIAN_POINT ( 'NONE',  ( -12.13525491562421088, 80.05000000546236549, -8.816778784387096835 ) ) ;
#9267 = ORIENTED_EDGE ( 'NONE', *, *, #32213, .F. ) ;
#9268 = CARTESIAN_POINT ( 'NONE',  ( -19.82091636218621389, 4.949999994537629178, 14.40073868116558842 ) ) ;
#9269 = CARTESIAN_POINT ( 'NONE',  ( -14.01125832528285109, 12.43527750092397532, 24.18731323226248264 ) ) ;
#9270 = CARTESIAN_POINT ( 'NONE',  ( 5.779280353836490358E-15, 26.50000000000000711, 32.49999999999999289 ) ) ;
#9271 = CARTESIAN_POINT ( 'NONE',  ( -33.58253175000000113, 49.02500000273116854, -10.91162601494193218 ) ) ;
#9272 = CARTESIAN_POINT ( 'NONE',  ( -10.37757302488623701, 5.775000002731192517, 31.93888565452638417 ) ) ;
#9273 = CARTESIAN_POINT ( 'NONE',  ( -10.37757302488623701, 53.77500000273120406, 31.93888565452638417 ) ) ;
#9274 = CARTESIAN_POINT ( 'NONE',  ( 19.09188309203694800, 54.96875000000000000, 19.09188309203660694 ) ) ;
#9275 = CARTESIAN_POINT ( 'NONE',  ( 26.02091320914851025, 41.94048583425730925, -14.97647472619946463 ) ) ;
#9276 = CARTESIAN_POINT ( 'NONE',  ( -28.00173670424535644, 27.17670166574268009, 7.543491769121936308 ) ) ;
#9277 = CARTESIAN_POINT ( 'NONE',  ( -32.50000000000000000, 64.50000000546239676, 0.000000000000000000 ) ) ;
#9278 = CARTESIAN_POINT ( 'NONE',  ( 2.688165632520823219E-15, 71.37500000273119838, 14.63369212191046387 ) ) ;
#9279 = CARTESIAN_POINT ( 'NONE',  ( 26.06988505166722803, 52.95795166574269075, -7.025853678916862854 ) ) ;
#9280 = CARTESIAN_POINT ( 'NONE',  ( -32.50000000000000000, 53.90000000000001279, -10.55989012756945300 ) ) ;
#9281 = CARTESIAN_POINT ( 'NONE',  ( -24.50000000000000000, 4.749999994537623671, -3.000384657911015469E-15 ) ) ;
#9282 = EDGE_LOOP ( 'NONE', ( #6475, #1071, #6971, #11527 ) ) ;
#9283 = CARTESIAN_POINT ( 'NONE',  ( 33.58253175000000823, 42.27500000273118275, 10.91162601494192863 ) ) ;
#9284 = CARTESIAN_POINT ( 'NONE',  ( 1.507698388325705758E-15, 3.624999997268822938, -24.62258325217400312 ) ) ;
#9285 = CARTESIAN_POINT ( 'NONE',  ( 32.50000000000000000, 29.50000000546236478, -3.980102097228898626E-15 ) ) ;
#9286 = ORIENTED_EDGE ( 'NONE', *, *, #8451, .T. ) ;
#9287 = CARTESIAN_POINT ( 'NONE',  ( -7.505752307973343918, 32.91145833333332860, -28.01184896238290989 ) ) ;
#9288 = ORIENTED_EDGE ( 'NONE', *, *, #16371, .T. ) ;
#9289 = CARTESIAN_POINT ( 'NONE',  ( 32.50000000000000000, 26.99999999999999645, -3.980102097228898626E-15 ) ) ;
#9290 = CARTESIAN_POINT ( 'NONE',  ( 33.58253175000000823, 48.02500000273119696, 10.91162601494192863 ) ) ;
#9291 = CARTESIAN_POINT ( 'NONE',  ( 28.01184896238304134, 54.68229166666665719, 7.505752307972846538 ) ) ;
#9292 = CARTESIAN_POINT ( 'NONE',  ( -32.50000000000000000, 14.60000000546239107, 10.55989012756946366 ) ) ;
#9293 = CARTESIAN_POINT ( 'NONE',  ( -12.13525491562420910, 78.19999999999998863, 8.816778784387098611 ) ) ;
#9294 = CARTESIAN_POINT ( 'NONE',  ( 7.236395654485755280, 16.72499999726881370, 22.27133577429736988 ) ) ;
#9295 = CARTESIAN_POINT ( 'NONE',  ( -26.29305231718579350, 53.80000000000001137, -19.10302069950537884 ) ) ;
#9296 = CARTESIAN_POINT ( 'NONE',  ( 3.980102097228898626E-15, 80.00000000000001421, 32.50000000000000000 ) ) ;
#9297 = CARTESIAN_POINT ( 'NONE',  ( 27.16883889988624290, 16.17500000273119909, 19.73931689729373673 ) ) ;
#9298 = CARTESIAN_POINT ( 'NONE',  ( 32.50000000000000711, 5.400000005462390895, 10.55989012756945122 ) ) ;
#9299 = CARTESIAN_POINT ( 'NONE',  ( 26.09010956794244507, 29.18190999907601579, 6.950374756619249084 ) ) ;
#9300 = CARTESIAN_POINT ( 'NONE',  ( 8.601468415847520532, 73.57500000273117280, 11.83890561707634781 ) ) ;
#9301 = CARTESIAN_POINT ( 'NONE',  ( 0.000000000000000000, 0.000000000000000000, 0.000000000000000000 ) ) ;
#9302 = CARTESIAN_POINT ( 'NONE',  ( 22.23068731925703645, 52.00000000000002132, 25.26668985625460095 ) ) ;
#9303 = CARTESIAN_POINT ( 'NONE',  ( -10.37757302488624411, 78.97500000273120691, -31.93888565452638417 ) ) ;
#9304 = EDGE_LOOP ( 'NONE', ( #20510, #12779, #2816, #31753 ) ) ;
#9305 = CARTESIAN_POINT ( 'NONE',  ( -14.47279130897152122, 4.424999997268826313, 19.92008829642072243 ) ) ;
#9306 = DIRECTION ( 'NONE',  ( -0.000000000000000000, 1.000000000000000000, -0.000000000000000000 ) ) ;
#9307 = CARTESIAN_POINT ( 'NONE',  ( 2.584737979205441561E-13, 45.08593750000000711, 27.95245687107222921 ) ) ;
#9308 = CARTESIAN_POINT ( 'NONE',  ( 27.16883889988624290, 67.92500000273120975, 19.73931689729373673 ) ) ;
#9309 = CARTESIAN_POINT ( 'NONE',  ( 6.486482029760649416E-15, 23.87500000273117706, 35.31076352940723240 ) ) ;
#9310 = CARTESIAN_POINT ( 'NONE',  ( 33.58253175000000113, 14.47500000273118737, -10.91162601494193751 ) ) ;
#9311 = CARTESIAN_POINT ( 'NONE',  ( 10.37757302488624767, 7.975000002731186477, 31.93888565452638417 ) ) ;
#9312 = CARTESIAN_POINT ( 'NONE',  ( 20.53372385742072481, 14.29725666759064318, -20.47846945139902175 ) ) ;
#9313 = CARTESIAN_POINT ( 'NONE',  ( 26.00068869287367335, 51.38802083333332149, 15.01150461594596308 ) ) ;
#9314 = CARTESIAN_POINT ( 'NONE',  ( 26.29305231718579350, 2.799999999999997158, 19.10302069950537529 ) ) ;
#9315 = CARTESIAN_POINT ( 'NONE',  ( 10.04305231718579705, 50.59999999999999432, 30.90933677959248982 ) ) ;
#9316 = CARTESIAN_POINT ( 'NONE',  ( -19.82091636218621389, 2.949999994537627401, 14.40073868116558842 ) ) ;
#9317 = CARTESIAN_POINT ( 'NONE',  ( -27.16883889988623935, 53.32500000273118701, 19.73931689729374739 ) ) ;
#9318 = CARTESIAN_POINT ( 'NONE',  ( -14.47279130897152122, 3.924999997268813434, 19.92008829642072243 ) ) ;
#9319 = VERTEX_POINT ( 'NONE', #2175 ) ;
#9320 = CARTESIAN_POINT ( 'NONE',  ( -10.37757302488623701, 61.77500000273118985, 31.93888565452638417 ) ) ;
#9321 = CYLINDRICAL_SURFACE ( 'NONE', #4769, 32.50000000000000000 ) ;
#9322 = CARTESIAN_POINT ( 'NONE',  ( -7.236395654485763274, 14.02499999726880553, 22.27133577429736633 ) ) ;
#9323 = CARTESIAN_POINT ( 'NONE',  ( -7.025853678916393008, 36.35454833425730925, 26.06988505166735592 ) ) ;
#9324 = PRODUCT_DEFINITION_FORMATION_WITH_SPECIFIED_SOURCE ( 'ANY', '', #12, .NOT_KNOWN. ) ;
#9325 = ORIENTED_EDGE ( 'NONE', *, *, #25677, .F. ) ;
#9326 = CARTESIAN_POINT ( 'NONE',  ( -33.58253175000000113, 31.22500000273118559, 10.91162601494193929 ) ) ;
#9327 = LINE ( 'NONE', #11744, #14319 ) ;
#9328 = VERTEX_POINT ( 'NONE', #15753 ) ;
#9329 = CARTESIAN_POINT ( 'NONE',  ( -7.505752307972844761, 58.97916666666666430, 28.01184896238304134 ) ) ;
#9330 = CARTESIAN_POINT ( 'NONE',  ( -27.16883889988624290, 63.17500000273118843, -19.73931689729374028 ) ) ;
#9331 = CARTESIAN_POINT ( 'NONE',  ( 0.000000000000000000, 82.00000000000001421, -32.50000000000000000 ) ) ;
#9332 = CARTESIAN_POINT ( 'NONE',  ( -10.37757302488624411, 70.72500000273119269, -31.93888565452638417 ) ) ;
#9333 = CARTESIAN_POINT ( 'NONE',  ( 7.505752307972854531, 33.19791666666665719, -28.01184896238303423 ) ) ;
#9334 = EDGE_CURVE ( 'NONE', #20206, #4188, #344, .T. ) ;
#9335 = CARTESIAN_POINT ( 'NONE',  ( -19.82091636218621034, 10.80000000000000426, -14.40073868116559552 ) ) ;
#9336 = CARTESIAN_POINT ( 'NONE',  ( 20.75514604977248467, 2.675000002731181770, -28.56700777964554305 ) ) ;
#9337 = CARTESIAN_POINT ( 'NONE',  ( 27.16883889988623935, 12.32500000273117990, -19.73931689729374384 ) ) ;
#9338 = CARTESIAN_POINT ( 'NONE',  ( -32.50000000000000000, 0.5000000054623809920, 0.000000000000000000 ) ) ;
#9339 = CARTESIAN_POINT ( 'NONE',  ( -28.00173670424535644, 44.36420166574269075, 7.543491769121936308 ) ) ;
#9340 = CARTESIAN_POINT ( 'NONE',  ( 12.13525491562421088, 80.79999999999998295, 8.816778784387095058 ) ) ;
#9341 = CARTESIAN_POINT ( 'NONE',  ( -15.01150461594595775, 55.68489583333332860, 26.00068869287368756 ) ) ;
#9342 = EDGE_CURVE ( 'NONE', #21143, #12035, #7365, .T. ) ;
#9343 = EDGE_CURVE ( 'NONE', #29552, #19947, #19204, .T. ) ;
#9344 = DIRECTION ( 'NONE',  ( -1.224646799147353454E-16, 1.000000000000000000, -0.000000000000000000 ) ) ;
#9345 = CARTESIAN_POINT ( 'NONE',  ( -4.732186688966233175E-15, 5.249999994537621895, 25.76082449383753925 ) ) ;
#9346 = CARTESIAN_POINT ( 'NONE',  ( 12.13525491562421088, 79.05000000546236549, 8.816778784387095058 ) ) ;
#9347 = CARTESIAN_POINT ( 'NONE',  ( 27.95245687107222921, 16.72656249999999645, -2.463307335887066074E-13 ) ) ;
#9348 = CARTESIAN_POINT ( 'NONE',  ( -27.16883889988623935, 35.32500000273120122, 19.73931689729374739 ) ) ;
#9349 = CARTESIAN_POINT ( 'NONE',  ( -13.91746824999999887, 76.87500000273116996, 0.000000000000000000 ) ) ;
#9350 = VECTOR ( 'NONE', #11885, 1000.000000000000000 ) ;
#9351 = CARTESIAN_POINT ( 'NONE',  ( -27.16883889988624290, 45.17500000273118133, -19.73931689729374028 ) ) ;
#9352 = CARTESIAN_POINT ( 'NONE',  ( -2.162160676586882350E-15, 30.87500000273119483, -35.31076352940722529 ) ) ;
#9353 = CARTESIAN_POINT ( 'NONE',  ( -32.50000000000000000, 68.09999999999996589, 10.55989012756946366 ) ) ;
#9354 = EDGE_CURVE ( 'NONE', #18278, #11746, #13813, .T. ) ;
#9355 = CARTESIAN_POINT ( 'NONE',  ( 24.50000000000000000, 2.000000000000001776, 0.000000000000000000 ) ) ;
#9356 =( BOUNDED_CURVE ( )  B_SPLINE_CURVE ( 2, ( #22103, #19526, #21604, #32047, #24343, #29633, #6135, #975, #16620, #6481, #16953, #27412, #3901 ),
 .UNSPECIFIED., .F., .T. ) 
 B_SPLINE_CURVE_WITH_KNOTS ( ( 3, 2, 2, 2, 2, 2, 3 ),
 ( 0.7500000000000000000, 0.7555555555555555358, 0.7666666666666667185, 0.7777777777777777901, 0.7888888888888888618, 0.8000000000000000444, 0.8055555555555555802 ),
 .UNSPECIFIED. ) 
 CURVE ( )  GEOMETRIC_REPRESENTATION_ITEM ( )  RATIONAL_B_SPLINE_CURVE ( ( 0.9755282581475768211, 0.9755282581475768211, 1.000000000000000000, 0.9510565162951535312, 1.000000000000000000, 0.9510565162951535312, 1.000000000000000000, 0.9510565162951535312, 1.000000000000000000, 0.9510565162951535312, 1.000000000000000000, 0.9755282581475768211, 0.9755282581475768211 ) ) 
 REPRESENTATION_ITEM ( '' )  );
#9357 = CARTESIAN_POINT ( 'NONE',  ( -26.29305231718579350, 65.80000000000001137, -19.10302069950537884 ) ) ;
#9358 = CARTESIAN_POINT ( 'NONE',  ( 1.507698388325705758E-15, 13.12499999726881228, -24.62258325217400312 ) ) ;
#9359 = CARTESIAN_POINT ( 'NONE',  ( 15.04653450569339945, 22.73659749907601935, 25.98046417659831775 ) ) ;
#9360 = CARTESIAN_POINT ( 'NONE',  ( 23.41746825000000243, 5.024999997268808194, 7.608796670333735079 ) ) ;
#9361 = CARTESIAN_POINT ( 'NONE',  ( 13.94119854578893580, 35.34076416574268364, -24.22776226481265383 ) ) ;
#9362 = CARTESIAN_POINT ( 'NONE',  ( 3.980102097228898626E-15, 52.00000000000000711, -32.50000000000000000 ) ) ;
#9363 = CARTESIAN_POINT ( 'NONE',  ( 33.58253175000000113, 10.22500000273117671, -10.91162601494193574 ) ) ;
#9364 = CARTESIAN_POINT ( 'NONE',  ( 14.47279130897151589, 14.82499999726881690, 19.92008829642072953 ) ) ;
#9365 = CARTESIAN_POINT ( 'NONE',  ( -27.95245687107222921, 59.69531250000000711, 2.498001805406602216E-13 ) ) ;
#9366 = ORIENTED_EDGE ( 'NONE', *, *, #21542, .T. ) ;
#9367 = CARTESIAN_POINT ( 'NONE',  ( -27.16883889988624290, 50.92500000273118843, -19.73931689729374028 ) ) ;
#9368 = CARTESIAN_POINT ( 'NONE',  ( 33.58253175000000823, 22.27500000273116854, 10.91162601494192863 ) ) ;
#9369 = ORIENTED_EDGE ( 'NONE', *, *, #1782, .T. ) ;
#9370 = CARTESIAN_POINT ( 'NONE',  ( 28.01184896238304134, 37.49479166666666430, 7.505752307972846538 ) ) ;
#9371 = CARTESIAN_POINT ( 'NONE',  ( 28.00173670424549499, 32.05767333425730214, 7.543491769121417612 ) ) ;
#9372 = CIRCLE ( 'NONE', #25834, 31.38736896855613523 ) ;
#9373 = VECTOR ( 'NONE', #3362, 1000.000000000000000 ) ;
#9374 = CARTESIAN_POINT ( 'NONE',  ( -19.82091636218621389, 3.200000000000008171, 14.40073868116558842 ) ) ;
#9375 = CARTESIAN_POINT ( 'NONE',  ( 24.50000000000000355, 13.64999999453761781, 7.960532557706212486 ) ) ;
#9376 = CARTESIAN_POINT ( 'NONE',  ( -7.236395654485757944, 15.22499999726881192, -22.27133577429736988 ) ) ;
#9377 = CARTESIAN_POINT ( 'NONE',  ( 33.58253175000000113, 20.47500000273120335, -10.91162601494193751 ) ) ;
#9378 = CARTESIAN_POINT ( 'NONE',  ( 32.50000000000000000, 25.60000000546239107, -10.55989012756945833 ) ) ;
#9379 = CARTESIAN_POINT ( 'NONE',  ( -10.04305231718578462, 70.40000000000001990, 30.90933677959249337 ) ) ;
#9380 = CARTESIAN_POINT ( 'NONE',  ( -20.08610463437156923, 6.800000005462376151, 27.64615127144130113 ) ) ;
#9381 = CARTESIAN_POINT ( 'NONE',  ( -11.54700538379251995, 86.00000000000001421, -19.99999999999999645 ) ) ;
#9382 = CARTESIAN_POINT ( 'NONE',  ( 20.53372385742072481, 58.98475666759065206, -20.47846945139902175 ) ) ;
#9383 = CARTESIAN_POINT ( 'NONE',  ( -2.162160676586881955E-15, 36.87500000273116996, -35.31076352940723240 ) ) ;
#9384 = CARTESIAN_POINT ( 'NONE',  ( -27.16883889988624290, 52.92500000273118843, -19.73931689729374028 ) ) ;
#9385 = CARTESIAN_POINT ( 'NONE',  ( -7.505752307972844761, 31.47916666666666075, 28.01184896238304134 ) ) ;
#9386 = CARTESIAN_POINT ( 'NONE',  ( -18.94512977948576093, 12.32499999726882578, 13.76444248337722698 ) ) ;
#9387 = CARTESIAN_POINT ( 'NONE',  ( 32.50000000000000000, 15.09999999999998899, -10.55989012756945833 ) ) ;
#9388 = CARTESIAN_POINT ( 'NONE',  ( 5.147494310547426899, 9.948745723915520145, -32.50000000000000000 ) ) ;
#9389 = CARTESIAN_POINT ( 'NONE',  ( -26.09010956794245217, 44.65065999907601935, -6.950374756619243755 ) ) ;
#9390 = CARTESIAN_POINT ( 'NONE',  ( 27.16883889988623935, 58.32500000273119412, -19.73931689729374384 ) ) ;
#9391 = CARTESIAN_POINT ( 'NONE',  ( 10.37757302488624056, 48.77500000273118985, -31.93888565452638417 ) ) ;
#9392 = CARTESIAN_POINT ( 'NONE',  ( 26.29305231718578995, 45.19999999999998863, -19.10302069950538240 ) ) ;
#9393 = CARTESIAN_POINT ( 'NONE',  ( -19.79898987322349768, 11.99999999999999645, -19.79898987322315307 ) ) ;
#9394 = CARTESIAN_POINT ( 'NONE',  ( 10.37757302488624767, 1.725000002731180704, 31.93888565452638417 ) ) ;
#9395 = CARTESIAN_POINT ( 'NONE',  ( 6.950374756619721595, 46.38059000092397355, 26.09010956794232428 ) ) ;
#9396 = EDGE_CURVE ( 'NONE', #30438, #16413, #33522, .T. ) ;
#9397 = CARTESIAN_POINT ( 'NONE',  ( -22.34336606078432652, 16.99999999999999645, -9.508438583994943016 ) ) ;
#9398 = CARTESIAN_POINT ( 'NONE',  ( 24.50000000000000000, 4.000000000000003553, 0.000000000000000000 ) ) ;
#9399 = CARTESIAN_POINT ( 'NONE',  ( -33.58253175000000113, 21.22500000273117848, 10.91162601494193929 ) ) ;
#9401 = PRESENTATION_LAYER_ASSIGNMENT (  '', '', ( #24223 ) ) ;
#9400 = DIRECTION ( 'NONE',  ( -1.224646799147353454E-16, 1.000000000000000000, -0.000000000000000000 ) ) ;
#9402 = CARTESIAN_POINT ( 'NONE',  ( 20.08610463437157279, 55.80000000546236549, -27.64615127144129758 ) ) ;
#9403 = CARTESIAN_POINT ( 'NONE',  ( 10.04305231718578817, 41.90000000546237402, -30.90933677959249337 ) ) ;
#9404 = CARTESIAN_POINT ( 'NONE',  ( 14.97647472619900455, 66.27826416574268364, -26.02091320914876960 ) ) ;
#9405 = CARTESIAN_POINT ( 'NONE',  ( -26.29305231718578995, 42.70000000546238539, 19.10302069950538595 ) ) ;
#9406 = CARTESIAN_POINT ( 'NONE',  ( 10.04305231718578817, 35.39999999999998437, -30.90933677959249337 ) ) ;
#9407 = CARTESIAN_POINT ( 'NONE',  ( 20.75514604977248467, 32.42500000273117422, -28.56700777964554305 ) ) ;
#9408 = CARTESIAN_POINT ( 'NONE',  ( -27.16883889988624290, 65.17500000273118133, -19.73931689729374028 ) ) ;
#9409 = CARTESIAN_POINT ( 'NONE',  ( 13.97622843553589966, 36.77864583333332860, -24.20753774853756113 ) ) ;
#9410 = EDGE_LOOP ( 'NONE', ( #13092, #5537, #8165, #3241 ) ) ;
#9411 = CARTESIAN_POINT ( 'NONE',  ( -33.58253175000000113, 71.02500000273118985, -10.91162601494193218 ) ) ;
#9412 = CARTESIAN_POINT ( 'NONE',  ( -26.00068869287368756, 39.35677083333331439, -15.01150461594595775 ) ) ;
#9413 = CARTESIAN_POINT ( 'NONE',  ( 0.000000000000000000, 82.00000000000001421, 0.000000000000000000 ) ) ;
#9414 = VERTEX_POINT ( 'NONE', #1105 ) ;
#9415 = CARTESIAN_POINT ( 'NONE',  ( -15.04653450569291984, 57.12277750092398065, 25.98046417659859486 ) ) ;
#9416 = CARTESIAN_POINT ( 'NONE',  ( -26.06988505166735237, 61.27642333425730925, -7.025853678916388567 ) ) ;
#9417 = CARTESIAN_POINT ( 'NONE',  ( -32.50000000000000000, 8.400000005462368691, -10.55989012756945478 ) ) ;
#9418 = CARTESIAN_POINT ( 'NONE',  ( -15.01150461594595775, 65.99739583333334281, 26.00068869287368756 ) ) ;
#9419 = CYLINDRICAL_SURFACE ( 'NONE', #27255, 32.50000000000000000 ) ;
#9420 = CARTESIAN_POINT ( 'NONE',  ( -27.16883889988623935, 39.57500000273117280, 19.73931689729374739 ) ) ;
#9421 = CARTESIAN_POINT ( 'NONE',  ( -20.08610463437156923, 40.80000000546237260, 27.64615127144130113 ) ) ;
#9422 = CARTESIAN_POINT ( 'NONE',  ( 11.25946833292375793, 74.17500000273119554, 8.180482586598731842 ) ) ;
#9423 = CARTESIAN_POINT ( 'NONE',  ( 20.75514604977248467, 26.42500000273118843, -28.56700777964554305 ) ) ;
#9424 = CARTESIAN_POINT ( 'NONE',  ( 19.82091636218621389, 13.94999999453763806, -14.40073868116559197 ) ) ;
#9425 = CARTESIAN_POINT ( 'NONE',  ( -20.75514604977248112, 57.67500000273118133, 28.56700777964554661 ) ) ;
#9426 = SURFACE_STYLE_FILL_AREA ( #32927 ) ;
#9427 = CARTESIAN_POINT ( 'NONE',  ( 26.29305231718579350, 32.80000000000001137, 19.10302069950537529 ) ) ;
#9428 = CARTESIAN_POINT ( 'NONE',  ( 6.277390505771533514E-15, 34.49999999999998579, 34.17252228774368916 ) ) ;
#9429 = CARTESIAN_POINT ( 'NONE',  ( 18.94512977948576093, 16.82499999726880091, -13.76444248337722875 ) ) ;
#9430 = CARTESIAN_POINT ( 'NONE',  ( -33.58253175000000113, 75.12500000273119838, 0.000000000000000000 ) ) ;
#9431 = MANIFOLD_SOLID_BREP ( 'Base-Revolve', #27066 ) ;
#9432 = CARTESIAN_POINT ( 'NONE',  ( 0.000000000000000000, 16.99999999999998579, -24.50000000000000000 ) ) ;
#9433 = CARTESIAN_POINT ( 'NONE',  ( 11.25946833292375793, 78.57500000273121543, -8.180482586598735395 ) ) ;
#9434 = CARTESIAN_POINT ( 'NONE',  ( -33.58253175000000113, 67.37500000273119838, 0.000000000000000000 ) ) ;
#9435 = CARTESIAN_POINT ( 'NONE',  ( -9.270509831248421762, 78.55000000546236549, 12.75976212528060039 ) ) ;
#9436 = CARTESIAN_POINT ( 'NONE',  ( -20.08610463437156923, 40.80000000546237260, 27.64615127144130113 ) ) ;
#9437 = CARTESIAN_POINT ( 'NONE',  ( 15.14183272437242245, 4.049999994537630599, -20.84094480462497856 ) ) ;
#9438 = CARTESIAN_POINT ( 'NONE',  ( 24.22776226481241224, 17.87798583425730570, -13.94119854578936923 ) ) ;
#9439 = EDGE_CURVE ( 'NONE', #27031, #22725, #18109, .T. ) ;
#9440 = CARTESIAN_POINT ( 'NONE',  ( 1.555960095263670572E-15, 8.249999994537619230, -24.50000000000000000 ) ) ;
#9441 = CONICAL_SURFACE ( 'NONE', #6169, 13.38432950954957157, 0.2613323016132363952 ) ;
#9442 = AXIS2_PLACEMENT_3D ( 'NONE', #20759, #5632, #12848 ) ;
#9443 = CARTESIAN_POINT ( 'NONE',  ( 20.75514604977249178, 39.82500000273116569, 28.56700777964553950 ) ) ;
#9444 = CARTESIAN_POINT ( 'NONE',  ( -33.58253175000000113, 3.275000002731191628, -10.91162601494193218 ) ) ;
#9445 = CARTESIAN_POINT ( 'NONE',  ( -20.75514604977248112, 53.67500000273119554, 28.56700777964554661 ) ) ;
#9446 = CARTESIAN_POINT ( 'NONE',  ( -15.04653450569291984, 46.81027750092398776, 25.98046417659859486 ) ) ;
#9447 = ADVANCED_FACE ( 'NONE', ( #7285 ), #17769, .F. ) ;
#9448 = CIRCLE ( 'NONE', #16601, 15.00000000000000000 ) ;
#9449 = CARTESIAN_POINT ( 'NONE',  ( 30.02300923189239867, 35.91368083240935505, -0.04044903255044467877 ) ) ;
#9450 = CARTESIAN_POINT ( 'NONE',  ( -20.08610463437157989, 62.20000000546237828, -27.64615127144129758 ) ) ;
#9451 = CARTESIAN_POINT ( 'NONE',  ( 13.91746824999999532, 71.97500000273117848, -4.522059556121118540 ) ) ;
#9452 = CARTESIAN_POINT ( 'NONE',  ( -24.22776226481266448, 68.85638916574269786, -13.94119854578892514 ) ) ;
#9453 = CARTESIAN_POINT ( 'NONE',  ( -26.29305231718579350, 57.80000000000001847, -19.10302069950537884 ) ) ;
#9454 = CARTESIAN_POINT ( 'NONE',  ( 10.04305231718578817, 73.90000000546237402, -30.90933677959249337 ) ) ;
#9455 = CARTESIAN_POINT ( 'NONE',  ( 15.01150461594643204, 13.86197916666666430, 26.00068869287340334 ) ) ;
#9456 = CARTESIAN_POINT ( 'NONE',  ( -33.58253175000000113, 39.37500000273118417, 0.000000000000000000 ) ) ;
#9457 =( BOUNDED_CURVE ( )  B_SPLINE_CURVE ( 2, ( #860, #11340, #19909, #15107, #6860, #27972, #25051, #30877, #30358, #6689, #12006, #4455, #14932 ),
 .UNSPECIFIED., .F., .T. ) 
 B_SPLINE_CURVE_WITH_KNOTS ( ( 3, 2, 2, 2, 2, 2, 3 ),
 ( 0.7115384615384615641, 0.7128205128205128416, 0.7153846153846153966, 0.7179487179487179516, 0.7205128205128205066, 0.7230769230769230616, 0.7243589743589743390 ),
 .UNSPECIFIED. ) 
 CURVE ( )  GEOMETRIC_REPRESENTATION_ITEM ( )  RATIONAL_B_SPLINE_CURVE ( ( 0.9755282581475768211, 0.9755282581475768211, 1.000000000000000000, 0.9510565162951535312, 1.000000000000000000, 0.9510565162951535312, 1.000000000000000000, 0.9510565162951535312, 1.000000000000000000, 0.9510565162951535312, 1.000000000000000000, 0.9755282581475768211, 0.9755282581475768211 ) ) 
 REPRESENTATION_ITEM ( '' )  );
#9458 = DIRECTION ( 'NONE',  ( -0.000000000000000000, -1.000000000000000000, -0.000000000000000000 ) ) ;
#9459 = VERTEX_POINT ( 'NONE', #9693 ) ;
#9460 = CARTESIAN_POINT ( 'NONE',  ( 10.04305231718578817, 31.90000000546237757, -30.90933677959249337 ) ) ;
#9461 = VERTEX_POINT ( 'NONE', #10220 ) ;
#9462 = CARTESIAN_POINT ( 'NONE',  ( -15.01150461594642138, 36.20572916666666430, -26.00068869287340334 ) ) ;
#9463 = CARTESIAN_POINT ( 'NONE',  ( -32.50000000000000000, 62.60000000546238397, 10.55989012756946366 ) ) ;
#9464 = VERTEX_POINT ( 'NONE', #28228 ) ;
#9465 = AXIS2_PLACEMENT_3D ( 'NONE', #7525, #121, #10613 ) ;
#9466 = DIRECTION ( 'NONE',  ( -1.000000000000000000, 0.000000000000000000, 0.000000000000000000 ) ) ;
#9467 = CARTESIAN_POINT ( 'NONE',  ( 10.37757302488624056, 46.52500000273118985, -31.93888565452638417 ) ) ;
#9468 = CARTESIAN_POINT ( 'NONE',  ( -7.236395654485763274, 16.02499999726880731, 22.27133577429736633 ) ) ;
#9469 = CARTESIAN_POINT ( 'NONE',  ( -5.147494310547430452, 47.55125428154683220, -32.49999999999999289 ) ) ;
#9470 = CARTESIAN_POINT ( 'NONE',  ( -2.092463501923844636E-15, 10.00000000546236301, -34.17252228774368916 ) ) ;
#9471 = VECTOR ( 'NONE', #33843, 1000.000000000000000 ) ;
#9472 = CARTESIAN_POINT ( 'NONE',  ( 33.58253175000000823, 66.02500000273118985, 10.91162601494192685 ) ) ;
#9473 = CARTESIAN_POINT ( 'NONE',  ( -14.47279130897151767, 13.82499999726882045, -19.92008829642072598 ) ) ;
#9474 = CARTESIAN_POINT ( 'NONE',  ( -32.50000000000000000, 53.90000000000001279, -10.55989012756945478 ) ) ;
#9475 = CARTESIAN_POINT ( 'NONE',  ( -5.147494310547430452, 13.55125428154684997, -32.49999999999999289 ) ) ;
#9476 = CARTESIAN_POINT ( 'NONE',  ( -33.58253175000000113, 17.27500000273118630, -10.91162601494193218 ) ) ;
#9477 = CARTESIAN_POINT ( 'NONE',  ( 3.980102097228898626E-15, 80.00000000000001421, 32.50000000000000000 ) ) ;
#9478 = CARTESIAN_POINT ( 'NONE',  ( -26.06988505166722803, 27.17670166574268009, 7.025853678916877953 ) ) ;
#9479 = CARTESIAN_POINT ( 'NONE',  ( 13.91746825000000065, 73.77500000273118985, 4.522059556121114987 ) ) ;
#9480 = DIRECTION ( 'NONE',  ( -0.000000000000000000, 1.000000000000000000, -0.000000000000000000 ) ) ;
#9481 = DIRECTION ( 'NONE',  ( -0.000000000000000000, 1.000000000000000000, -0.000000000000000000 ) ) ;
#9482 = CARTESIAN_POINT ( 'NONE',  ( -2.092463501923844636E-15, 5.500000000000000888, -34.17252228774368916 ) ) ;
#9483 = ORIENTED_EDGE ( 'NONE', *, *, #5286, .F. ) ;
#9484 = CARTESIAN_POINT ( 'NONE',  ( 23.41746825000000243, 7.224999997268826135, -7.608796670333727974 ) ) ;
#9485 = CARTESIAN_POINT ( 'NONE',  ( 4.300734207923761154, 71.47500000273119269, 13.23629886949340495 ) ) ;
#9486 = CARTESIAN_POINT ( 'NONE',  ( 26.07999730980490227, 47.80729166666666430, 6.988114217767821046 ) ) ;
#9487 = CARTESIAN_POINT ( 'NONE',  ( 20.75514604977248467, 60.42500000273118133, -28.56700777964554305 ) ) ;
#9488 = CARTESIAN_POINT ( 'NONE',  ( -10.37757302488623701, 25.77500000273118275, 31.93888565452638417 ) ) ;
#9489 = CARTESIAN_POINT ( 'NONE',  ( -20.75514604977248823, 11.07500000273119056, -28.56700777964554305 ) ) ;
#9490 = CARTESIAN_POINT ( 'NONE',  ( 20.75514604977248467, 4.675000002731176885, -28.56700777964554305 ) ) ;
#9491 = CARTESIAN_POINT ( 'NONE',  ( -15.04653450569291984, 15.87277750092397710, 25.98046417659859486 ) ) ;
#9492 = EDGE_CURVE ( 'NONE', #23750, #26696, #21613, .T. ) ;
#9493 = CARTESIAN_POINT ( 'NONE',  ( -15.01150461594595775, 62.55989583333332860, 26.00068869287368756 ) ) ;
#9494 = ADVANCED_FACE ( 'NONE', ( #25994 ), #25855, .T. ) ;
#9495 = CARTESIAN_POINT ( 'NONE',  ( -1.778240108872766143E-15, 69.49999999999998579, -32.49999999999999289 ) ) ;
#9496 = CARTESIAN_POINT ( 'NONE',  ( 20.08610463437158344, 44.69999999999998153, 27.64615127144129403 ) ) ;
#9497 = CARTESIAN_POINT ( 'NONE',  ( 10.37757302488624767, 53.72500000273117138, 31.93888565452638417 ) ) ;
#9498 = VECTOR ( 'NONE', #10652, 1000.000000000000000 ) ;
#9499 = CARTESIAN_POINT ( 'NONE',  ( 23.41746825000000243, 0.7249999972688272454, -7.608796670333727974 ) ) ;
#9500 = CARTESIAN_POINT ( 'NONE',  ( 0.000000000000000000, 74.00000000000001421, 0.000000000000000000 ) ) ;
#9501 = ORIENTED_EDGE ( 'NONE', *, *, #8453, .T. ) ;
#9502 = CARTESIAN_POINT ( 'NONE',  ( 20.75514604977249178, 58.07500000273117990, 28.56700777964553950 ) ) ;
#9503 = CARTESIAN_POINT ( 'NONE',  ( 26.29305231718579350, 16.79999999999998295, 19.10302069950537529 ) ) ;
#9504 = CARTESIAN_POINT ( 'NONE',  ( 14.47279130897151767, 10.92499999726882365, -19.92008829642072598 ) ) ;
#9505 = CARTESIAN_POINT ( 'NONE',  ( 13.94119854578937812, 29.04986083425730570, 24.22776226481240514 ) ) ;
#9506 = ORIENTED_EDGE ( 'NONE', *, *, #14686, .F. ) ;
#9507 = CARTESIAN_POINT ( 'NONE',  ( -27.16883889988624290, 32.92500000273117422, -19.73931689729374028 ) ) ;
#9508 = CARTESIAN_POINT ( 'NONE',  ( 3.445340210940985210E-14, 5.499999999999997335, 24.50000000000000000 ) ) ;
#9509 = ORIENTED_EDGE ( 'NONE', *, *, #22859, .T. ) ;
#9510 = CARTESIAN_POINT ( 'NONE',  ( 15.01150461594596308, 64.27864583333332860, -26.00068869287367335 ) ) ;
#9511 = CARTESIAN_POINT ( 'NONE',  ( -2.162160676586881955E-15, 62.87500000273120548, -35.31076352940723240 ) ) ;
#9512 = LINE ( 'NONE', #14502, #30263 ) ;
#9513 = CARTESIAN_POINT ( 'NONE',  ( 27.16883889988623935, 70.32500000273117280, -19.73931689729374384 ) ) ;
#9514 = CARTESIAN_POINT ( 'NONE',  ( -20.50609665440969209, 35.20312500000000000, 20.50609665441005092 ) ) ;
#9515 = CARTESIAN_POINT ( 'NONE',  ( 15.14183272437242245, 14.29999999999998472, -20.84094480462497856 ) ) ;
#9516 = DIRECTION ( 'NONE',  ( 0.000000000000000000, 0.000000000000000000, -1.000000000000000000 ) ) ;
#9517 = CARTESIAN_POINT ( 'NONE',  ( 20.75514604977248467, 10.42500000273120087, -28.56700777964554305 ) ) ;
#9518 = CARTESIAN_POINT ( 'NONE',  ( 0.000000000000000000, 70.00000000000000000, 0.000000000000000000 ) ) ;
#9519 = CARTESIAN_POINT ( 'NONE',  ( 7.543491769121922985, 53.81732666574268364, 28.00173670424535644 ) ) ;
#9520 = CARTESIAN_POINT ( 'NONE',  ( 12.13525491562420910, 75.19999999999998863, -8.816778784387098611 ) ) ;
#9521 = VECTOR ( 'NONE', #14395, 1000.000000000000000 ) ;
#9522 = CARTESIAN_POINT ( 'NONE',  ( 7.505752307972854531, 57.26041666666666430, -28.01184896238303423 ) ) ;
#9523 = FACE_OUTER_BOUND ( 'NONE', #26108, .T. ) ;
#9524 = CARTESIAN_POINT ( 'NONE',  ( 26.29305231718578995, 61.70000000546238539, -19.10302069950538240 ) ) ;
#9525 = CARTESIAN_POINT ( 'NONE',  ( 1.577395562988744260E-15, 6.249999994537619230, -25.76082449383753925 ) ) ;
#9526 = CARTESIAN_POINT ( 'NONE',  ( -9.657523855033125146E-16, 75.75000000546238255, -15.77193336357400710 ) ) ;
#9527 = CARTESIAN_POINT ( 'NONE',  ( -13.97622843553632421, 19.01822916666666785, -24.20753774853731599 ) ) ;
#9528 = CARTESIAN_POINT ( 'NONE',  ( 27.16883889988623935, 38.32500000273120122, -19.73931689729374384 ) ) ;
#9529 = CARTESIAN_POINT ( 'NONE',  ( -33.58253175000000113, 79.12500000273118417, 0.000000000000000000 ) ) ;
#9530 = CARTESIAN_POINT ( 'NONE',  ( 33.58253175000000113, 40.47500000273118559, -10.91162601494193751 ) ) ;
#9531 = CARTESIAN_POINT ( 'NONE',  ( -27.16883889988624290, 23.17500000273120619, -19.73931689729374028 ) ) ;
#9532 = CARTESIAN_POINT ( 'NONE',  ( 5.147494310547434893, 40.55125428154684641, 32.49999999999999289 ) ) ;
#9533 = DIRECTION ( 'NONE',  ( 0.000000000000000000, -1.000000000000000000, 0.000000000000000000 ) ) ;
#9534 = CARTESIAN_POINT ( 'NONE',  ( -1.778240108872766143E-15, 33.50000000000000000, -32.49999999999999289 ) ) ;
#9535 = CARTESIAN_POINT ( 'NONE',  ( -26.29305231718579350, 67.80000000000001137, -19.10302069950537884 ) ) ;
#9536 = CARTESIAN_POINT ( 'NONE',  ( -18.94512977948575738, 11.42499999726881477, -13.76444248337723231 ) ) ;
#9537 = CARTESIAN_POINT ( 'NONE',  ( -25.98046417659831420, 27.03347249907602290, 15.04653450569339945 ) ) ;
#9538 = CARTESIAN_POINT ( 'NONE',  ( -23.41746825000000598, 4.224999997268803931, 7.608796670333726198 ) ) ;
#9539 = CARTESIAN_POINT ( 'NONE',  ( -19.06425588902558133, 33.76524333240934084, 19.11951029504797006 ) ) ;
#9540 = STYLED_ITEM ( 'NONE', ( #5143 ), #15260 ) ;
#9541 = DIRECTION ( 'NONE',  ( -0.000000000000000000, -1.000000000000000000, -0.000000000000000000 ) ) ;
#9542 = CARTESIAN_POINT ( 'NONE',  ( -33.58253175000000113, 15.22500000273119269, 10.91162601494193929 ) ) ;
#9543 = CARTESIAN_POINT ( 'NONE',  ( 18.94512977948576093, 15.32499999726882933, -13.76444248337722875 ) ) ;
#9544 = CARTESIAN_POINT ( 'NONE',  ( 26.07999730980490227, 61.55729166666666430, 6.988114217767821046 ) ) ;
#9545 = VERTEX_POINT ( 'NONE', #1786 ) ;
#9546 = CARTESIAN_POINT ( 'NONE',  ( 33.58253175000000113, 48.22500000273119269, -10.91162601494193751 ) ) ;
#9547 = EDGE_CURVE ( 'NONE', #12231, #23106, #14342, .T. ) ;
#9548 = CARTESIAN_POINT ( 'NONE',  ( -33.58253175000000113, 25.27500000273119696, -10.91162601494193218 ) ) ;
#9549 = ORIENTED_EDGE ( 'NONE', *, *, #26976, .T. ) ;
#9550 = CARTESIAN_POINT ( 'NONE',  ( -30.02300923189239512, 32.19531250000000000, 2.654126918244515359E-13 ) ) ;
#9551 = CARTESIAN_POINT ( 'NONE',  ( 28.00173670424549499, 28.62017333425730925, 7.543491769121417612 ) ) ;
#9552 = MANIFOLD_SOLID_BREP ( 'Extrude-Thin2', #5149 ) ;
#9553 = CARTESIAN_POINT ( 'NONE',  ( -19.82091636218621034, 8.549999994537621717, -14.40073868116559552 ) ) ;
#9554 = CARTESIAN_POINT ( 'NONE',  ( -15.14183272437241889, 18.44999999453760964, -20.84094480462497856 ) ) ;
#9555 = EDGE_CURVE ( 'NONE', #2565, #19940, #13472, .T. ) ;
#9556 = CARTESIAN_POINT ( 'NONE',  ( -18.94512977948576093, 11.82499999726882578, 13.76444248337722698 ) ) ;
#9557 = PRODUCT ( 'primary mounting nut', 'primary mounting nut', '', ( #20743 ) ) ;
#9558 = CARTESIAN_POINT ( 'NONE',  ( 20.75514604977249178, 24.07500000273120122, 28.56700777964553950 ) ) ;
#9559 = CARTESIAN_POINT ( 'NONE',  ( -10.04305231718579172, 26.10000000546236620, -30.90933677959248982 ) ) ;
#9560 = CARTESIAN_POINT ( 'NONE',  ( -20.08610463437156923, 66.30000000000001137, 27.64615127144130113 ) ) ;
#9561 = CYLINDRICAL_SURFACE ( 'NONE', #22012, 32.50000000000000000 ) ;
#9562 = CARTESIAN_POINT ( 'NONE',  ( -4.491574677915616043, 74.00000000000000000, 13.59926041343836012 ) ) ;
#9563 = CARTESIAN_POINT ( 'NONE',  ( -7.505752307973343918, 15.72395833333332860, -28.01184896238290989 ) ) ;
#9564 = CARTESIAN_POINT ( 'NONE',  ( 20.75514604977249178, 38.07500000273116569, 28.56700777964553950 ) ) ;
#9565 = CARTESIAN_POINT ( 'NONE',  ( -2.584737979205442066E-13, 29.61718749999999645, -30.02300923189239867 ) ) ;
#9566 = SHAPE_DEFINITION_REPRESENTATION ( #2498, #10290 ) ;
#9567 = EDGE_CURVE ( 'NONE', #33751, #12166, #31914, .T. ) ;
#9568 = CARTESIAN_POINT ( 'NONE',  ( -4.523095164977116484E-15, 18.62499999726881583, 24.62258325217400312 ) ) ;
#9569 = CARTESIAN_POINT ( 'NONE',  ( -26.29305231718578995, 16.19999999999999218, 19.10302069950538595 ) ) ;
#9570 = CARTESIAN_POINT ( 'NONE',  ( -10.04305231718579172, 51.60000000000000853, -30.90933677959248982 ) ) ;
#9571 = CARTESIAN_POINT ( 'NONE',  ( 27.95245687107223276, 39.35118083240935505, -0.04044903255042905932 ) ) ;
#9572 =( BOUNDED_CURVE ( )  B_SPLINE_CURVE ( 2, ( #28232, #15024, #1972, #12447, #4718, #15198, #15546, #10896, #15718, #10724, #2491, #26173, #239 ),
 .UNSPECIFIED., .F., .T. ) 
 B_SPLINE_CURVE_WITH_KNOTS ( ( 3, 2, 2, 2, 2, 2, 3 ),
 ( 0.1217948717948718063, 0.1230769230769230838, 0.1256410256410256387, 0.1282051282051281937, 0.1307692307692307765, 0.1333333333333333315, 0.1346153846153846090 ),
 .UNSPECIFIED. ) 
 CURVE ( )  GEOMETRIC_REPRESENTATION_ITEM ( )  RATIONAL_B_SPLINE_CURVE ( ( 0.9755282581475767101, 0.9755282581475768211, 1.000000000000000000, 0.9510565162951535312, 1.000000000000000000, 0.9510565162951535312, 1.000000000000000000, 0.9510565162951535312, 1.000000000000000000, 0.9510565162951535312, 1.000000000000000000, 0.9755282581475768211, 0.9755282581475768211 ) ) 
 REPRESENTATION_ITEM ( '' )  );
#9573 = CARTESIAN_POINT ( 'NONE',  ( -33.58253175000000113, 59.22500000273119269, 10.91162601494193929 ) ) ;
#9574 = CARTESIAN_POINT ( 'NONE',  ( 10.37757302488624767, 59.97500000273119269, 31.93888565452638417 ) ) ;
#9575 = CARTESIAN_POINT ( 'NONE',  ( 33.58253175000000823, 46.27500000273120406, 10.91162601494192685 ) ) ;
#9576 = CARTESIAN_POINT ( 'NONE',  ( 5.147494310547434893, 44.55125428154684641, 32.49999999999999289 ) ) ;
#9577 = CARTESIAN_POINT ( 'NONE',  ( 5.779280353836490358E-15, 67.00000000546236834, 32.49999999999999289 ) ) ;
#9578 = CARTESIAN_POINT ( 'NONE',  ( -32.50000000000000000, 50.09999999999998721, 10.55989012756946366 ) ) ;
#9579 = CARTESIAN_POINT ( 'NONE',  ( 26.06988505166735592, 49.24517333425730925, 7.025853678916393896 ) ) ;
#9580 = CARTESIAN_POINT ( 'NONE',  ( 5.147494310547426899, 63.94874572391552903, -32.50000000000000000 ) ) ;
#9581 = CARTESIAN_POINT ( 'NONE',  ( -26.29305231718579350, 41.80000000000000426, -19.10302069950537884 ) ) ;
#9582 = CARTESIAN_POINT ( 'NONE',  ( -10.37757302488623701, 21.52500000273117919, 31.93888565452638417 ) ) ;
#9583 = DIRECTION ( 'NONE',  ( 0.000000000000000000, 0.000000000000000000, -1.000000000000000000 ) ) ;
#9584 = CARTESIAN_POINT ( 'NONE',  ( 11.54700538379251107, 96.00000000000002842, -19.99999999999999645 ) ) ;
#9585 = CARTESIAN_POINT ( 'NONE',  ( 20.53372385742108008, 63.84336833240935505, 20.47846945139866648 ) ) ;
#9586 = CARTESIAN_POINT ( 'NONE',  ( 10.04305231718578817, 41.90000000546238823, -30.90933677959249337 ) ) ;
#9587 = DIRECTION ( 'NONE',  ( -1.224646799147353454E-16, 1.000000000000000000, -0.000000000000000000 ) ) ;
#9588 = CARTESIAN_POINT ( 'NONE',  ( 10.37757302488624056, 34.52500000273117564, -31.93888565452638417 ) ) ;
#9589 = CARTESIAN_POINT ( 'NONE',  ( -13.97622843553632421, 36.20572916666666430, -24.20753774853731599 ) ) ;
#9590 = ORIENTED_EDGE ( 'NONE', *, *, #30738, .T. ) ;
#9591 = CARTESIAN_POINT ( 'NONE',  ( -2.162160676586881955E-15, 70.62500000273118417, -35.31076352940723240 ) ) ;
#9592 = CARTESIAN_POINT ( 'NONE',  ( 15.01150461594643204, 37.92447916666666430, 26.00068869287340334 ) ) ;
#9593 = AXIS2_PLACEMENT_3D ( 'NONE', #17629, #20555, #28090 ) ;
#9594 = DIRECTION ( 'NONE',  ( 0.7071067811865460184, 0.7071067811865489050, 8.659560562354914369E-17 ) ) ;
#9595 = VERTEX_POINT ( 'NONE', #62 ) ;
#9596 = CARTESIAN_POINT ( 'NONE',  ( -28.00173670424549499, 57.83892333425730214, -7.543491769121417612 ) ) ;
#9597 = CARTESIAN_POINT ( 'NONE',  ( 19.06425588902592239, 63.28163166759064495, 19.11951029504763611 ) ) ;
#9598 = CARTESIAN_POINT ( 'NONE',  ( -10.37757302488623701, 13.52500000273119873, 31.93888565452638417 ) ) ;
#9599 = CARTESIAN_POINT ( 'NONE',  ( 15.04653450569339945, 15.86159749907602112, 25.98046417659831775 ) ) ;
#9600 = CARTESIAN_POINT ( 'NONE',  ( -5.147494310547531704, 46.44874571845316780, 32.49999999999996447 ) ) ;
#9601 = CARTESIAN_POINT ( 'NONE',  ( 33.58253175000000823, 42.27500000273118275, 10.91162601494192863 ) ) ;
#9602 = CARTESIAN_POINT ( 'NONE',  ( 20.08610463437158344, 45.20000000546239249, 27.64615127144129403 ) ) ;
#9603 = CARTESIAN_POINT ( 'NONE',  ( -15.00000000000000000, 81.89999999999997726, -4.873795443493594171 ) ) ;
#9604 = CARTESIAN_POINT ( 'NONE',  ( -10.37757302488623701, 31.52500000273117564, 31.93888565452638417 ) ) ;
#9605 = CARTESIAN_POINT ( 'NONE',  ( 15.14183272437242422, 14.04999999453763593, -20.84094480462497856 ) ) ;
#9606 = CARTESIAN_POINT ( 'NONE',  ( 27.16883889988623935, 52.57500000273118701, -19.73931689729374384 ) ) ;
#9607 = SHAPE_REPRESENTATION_RELATIONSHIP ( 'NONE' , 'NONE' ,  #31529, #10725 ) ;
#9608 = CARTESIAN_POINT ( 'NONE',  ( -32.50000000000000000, 33.90000000000001279, -10.55989012756945478 ) ) ;
#9609 = CARTESIAN_POINT ( 'NONE',  ( 10.04305231718579705, 36.59999999999999432, 30.90933677959248982 ) ) ;
#9610 = CARTESIAN_POINT ( 'NONE',  ( -14.47279130897152122, 15.92499999726881121, 19.92008829642072243 ) ) ;
#9611 = CARTESIAN_POINT ( 'NONE',  ( 33.58253175000000113, 76.12500000273119838, -4.112674001490185761E-15 ) ) ;
#9612 = CARTESIAN_POINT ( 'NONE',  ( 5.147494310547434893, 62.55125428154684641, 32.49999999999999289 ) ) ;
#9613 = CARTESIAN_POINT ( 'NONE',  ( -27.16883889988624290, 67.17500000273119554, -19.73931689729374028 ) ) ;
#9614 = CARTESIAN_POINT ( 'NONE',  ( 4.635254915624209993, 79.65000000546234560, -14.26584774442730463 ) ) ;
#9615 = VERTEX_POINT ( 'NONE', #28901 ) ;
#9616 = CARTESIAN_POINT ( 'NONE',  ( 20.75514604977248467, 16.42500000273118133, -28.56700777964554305 ) ) ;
#9617 = CARTESIAN_POINT ( 'NONE',  ( -19.82091636218621389, 10.94999999453763451, 14.40073868116558842 ) ) ;
#9618 =( GEOMETRIC_REPRESENTATION_CONTEXT ( 3 ) GLOBAL_UNCERTAINTY_ASSIGNED_CONTEXT ( ( #16812 ) ) GLOBAL_UNIT_ASSIGNED_CONTEXT ( ( #6530, #8594, #19911 ) ) REPRESENTATION_CONTEXT ( 'NONE', 'WORKASPACE' ) );
#9619 = CARTESIAN_POINT ( 'NONE',  ( 26.06988505166735592, 25.18267333425730214, 7.025853678916393896 ) ) ;
#9620 = LINE ( 'NONE', #33985, #3656 ) ;
#9621 = CARTESIAN_POINT ( 'NONE',  ( -2.162160676586881955E-15, 42.62500000273119838, -35.31076352940723240 ) ) ;
#9622 = CARTESIAN_POINT ( 'NONE',  ( -20.75514604977248823, 7.075000002731188786, -28.56700777964554305 ) ) ;
#9623 = CARTESIAN_POINT ( 'NONE',  ( -20.75514604977248823, 57.07500000273117990, -28.56700777964554305 ) ) ;
#9624 = CARTESIAN_POINT ( 'NONE',  ( 28.02196122052045268, 48.95871500092396644, -7.468012846824774620 ) ) ;
#9625 = CARTESIAN_POINT ( 'NONE',  ( 0.04044903255045854962, 33.33555583240935505, 30.02300923189239867 ) ) ;
#9626 = CARTESIAN_POINT ( 'NONE',  ( 10.04305231718578817, 57.90000000546240244, -30.90933677959249337 ) ) ;
#9627 = CARTESIAN_POINT ( 'NONE',  ( -13.91746824999999532, 74.97500000273117848, 4.522059556121122093 ) ) ;
#9628 = AXIS2_PLACEMENT_3D ( 'NONE', #6535, #27298, #19082 ) ;
#9629 = CARTESIAN_POINT ( 'NONE',  ( -13.97622843553632421, 12.14322916666666430, -24.20753774853731599 ) ) ;
#9630 = CARTESIAN_POINT ( 'NONE',  ( 3.980102097228898626E-15, 80.00000000000001421, 32.50000000000000000 ) ) ;
#9631 = CARTESIAN_POINT ( 'NONE',  ( -32.50000000000000000, 76.60000000546239107, 10.55989012756946366 ) ) ;
#9632 = CARTESIAN_POINT ( 'NONE',  ( 4.635254915624209993, 79.39999999999997726, -14.26584774442730463 ) ) ;
#9633 = CARTESIAN_POINT ( 'NONE',  ( 27.16883889988624290, 42.17500000273118133, 19.73931689729373673 ) ) ;
#9634 = CARTESIAN_POINT ( 'NONE',  ( -7.236395654485757944, 9.724999997268806595, -22.27133577429736988 ) ) ;
#9635 = EDGE_LOOP ( 'NONE', ( #29393, #11737, #4444, #12558 ) ) ;
#9636 = CARTESIAN_POINT ( 'NONE',  ( -10.37757302488623701, 71.77500000273117564, 31.93888565452638417 ) ) ;
#9637 = CARTESIAN_POINT ( 'NONE',  ( 10.04305231718579705, 31.10000000546238397, 30.90933677959248982 ) ) ;
#9638 = ORIENTED_EDGE ( 'NONE', *, *, #1940, .F. ) ;
#9639 = CARTESIAN_POINT ( 'NONE',  ( -15.01150461594595775, 35.05989583333332860, 26.00068869287368756 ) ) ;
#9640 = CARTESIAN_POINT ( 'NONE',  ( 10.04305231718578817, 63.90000000546236691, -30.90933677959249337 ) ) ;
#9642 = ORIENTED_EDGE ( 'NONE', *, *, #18618, .T. ) ;
#9641 = EDGE_CURVE ( 'NONE', #9615, #25517, #29700, .T. ) ;
#9643 = DIRECTION ( 'NONE',  ( -1.000000000000000000, -1.239088197126291063E-16, 0.000000000000000000 ) ) ;
#9644 = CARTESIAN_POINT ( 'NONE',  ( -20.75514604977248112, 45.42500000273119554, 28.56700777964554661 ) ) ;
#9645 = CARTESIAN_POINT ( 'NONE',  ( -8.891200544363830713E-16, 73.75000000546239676, -15.00000000000000000 ) ) ;
#9646 = ADVANCED_FACE ( 'NONE', ( #2999 ), #3170, .F. ) ;
#9647 = APPLICATION_CONTEXT ( 'automotive_design' ) ;
#9648 = CARTESIAN_POINT ( 'NONE',  ( -26.29305231718579350, 2.300000005462377040, -19.10302069950537884 ) ) ;
#9649 = CARTESIAN_POINT ( 'NONE',  ( 33.58253175000000113, 66.22500000273120691, -10.91162601494193574 ) ) ;
#9650 = LINE ( 'NONE', #31096, #13342 ) ;
#9651 = CARTESIAN_POINT ( 'NONE',  ( 20.08610463437158344, 50.69999999999999574, 27.64615127144129403 ) ) ;
#9652 = CARTESIAN_POINT ( 'NONE',  ( -10.04305231718578462, 14.39999999999999680, 30.90933677959249337 ) ) ;
#9653 = CARTESIAN_POINT ( 'NONE',  ( -33.58253175000000113, 17.37500000273117706, 0.000000000000000000 ) ) ;
#9654 = CARTESIAN_POINT ( 'NONE',  ( -5.147494310547430452, 24.05125428700921830, -32.49999999999999289 ) ) ;
#9655 = CARTESIAN_POINT ( 'NONE',  ( 24.18731323226221974, 25.31472249907601579, -14.01125832528328985 ) ) ;
#9656 = CARTESIAN_POINT ( 'NONE',  ( -11.25946833292375793, 77.57500000273121543, 8.180482586598737171 ) ) ;
#9657 = CARTESIAN_POINT ( 'NONE',  ( 0.000000000000000000, 52.00000000000000711, 0.000000000000000000 ) ) ;
#9658 = CARTESIAN_POINT ( 'NONE',  ( 5.147494310547426899, 53.94874572391552192, -32.50000000000000000 ) ) ;
#9659 = CARTESIAN_POINT ( 'NONE',  ( 27.16883889988624290, 78.17500000273118133, 19.73931689729373673 ) ) ;
#9660 = ORIENTED_EDGE ( 'NONE', *, *, #20647, .F. ) ;
#9661 = CARTESIAN_POINT ( 'NONE',  ( -23.41746824999999887, 14.12499999726882294, -2.867812753649727150E-15 ) ) ;
#9662 = CARTESIAN_POINT ( 'NONE',  ( 5.334720326618300005E-14, 72.00000000546238255, -32.50000000000000000 ) ) ;
#9663 = CARTESIAN_POINT ( 'NONE',  ( -19.09188309203694445, 53.25000000000000000, -19.09188309203661049 ) ) ;
#9664 = CARTESIAN_POINT ( 'NONE',  ( -10.37757302488624411, 60.72500000273119269, -31.93888565452638417 ) ) ;
#9665 = CARTESIAN_POINT ( 'NONE',  ( 27.16883889988623935, 24.57500000273120477, -19.73931689729374384 ) ) ;
#9666 = CARTESIAN_POINT ( 'NONE',  ( -27.16883889988624290, 13.17500000273118310, -19.73931689729374028 ) ) ;
#9667 = CARTESIAN_POINT ( 'NONE',  ( 6.486482029760648627E-15, 1.875000002731177950, 35.31076352940722529 ) ) ;
#9668 = CARTESIAN_POINT ( 'NONE',  ( 14.97647472619947351, 22.17486083425730925, 26.02091320914850314 ) ) ;
#9669 = CARTESIAN_POINT ( 'NONE',  ( -20.50609665440969209, 62.70312500000000000, 20.50609665441005092 ) ) ;
#9670 = CARTESIAN_POINT ( 'NONE',  ( 32.50000000000000711, 77.40000000546240244, 10.55989012756945122 ) ) ;
#9671 =( BOUNDED_CURVE ( )  B_SPLINE_CURVE ( 2, ( #18241, #5009, #15, #15492, #2615, #33845, #5185 ),
 .UNSPECIFIED., .F., .T. ) 
 B_SPLINE_CURVE_WITH_KNOTS ( ( 3, 2, 2, 3 ),
 ( 0.9499999999999999556, 0.9599999999999999645, 0.9799999999999999822, 1.000000000000000000 ),
 .UNSPECIFIED. ) 
 CURVE ( )  GEOMETRIC_REPRESENTATION_ITEM ( )  RATIONAL_B_SPLINE_CURVE ( ( 0.9755282581475768211, 0.9755282581475768211, 1.000000000000000000, 0.9510565162951535312, 1.000000000000000000, 0.9510565162951535312, 1.000000000000000000 ) ) 
 REPRESENTATION_ITEM ( '' )  );
#9672 = CARTESIAN_POINT ( 'NONE',  ( 2.688165632520823219E-15, 73.87500000273119838, 14.63369212191046209 ) ) ;
#9673 = CARTESIAN_POINT ( 'NONE',  ( -20.08610463437156923, 44.30000000000000426, 27.64615127144130113 ) ) ;
#9674 = CARTESIAN_POINT ( 'NONE',  ( -33.58253175000000113, 43.12500000273116996, 0.000000000000000000 ) ) ;
#9675 = CARTESIAN_POINT ( 'NONE',  ( 7.236395654485755280, 18.72499999726881370, 22.27133577429736988 ) ) ;
#9676 = ORIENTED_EDGE ( 'NONE', *, *, #33754, .T. ) ;
#9677 = CARTESIAN_POINT ( 'NONE',  ( -27.16883889988623935, 57.57500000273117990, 19.73931689729374739 ) ) ;
#9678 = DIRECTION ( 'NONE',  ( 0.000000000000000000, 0.000000000000000000, -1.000000000000000000 ) ) ;
#9679 = CARTESIAN_POINT ( 'NONE',  ( 18.94512977948575738, 12.42499999726881477, 13.76444248337723408 ) ) ;
#9680 = CARTESIAN_POINT ( 'NONE',  ( -6.950374756619716266, 34.34934000092397355, -26.09010956794232428 ) ) ;
#9681 = VERTEX_POINT ( 'NONE', #10549 ) ;
#9682 = CARTESIAN_POINT ( 'NONE',  ( 33.58253175000000113, 32.22500000273117848, -10.91162601494193751 ) ) ;
#9684 = CARTESIAN_POINT ( 'NONE',  ( -20.08610463437157989, 34.20000000546237828, -27.64615127144129758 ) ) ;
#9683 = CIRCLE ( 'NONE', #9133, 30.00000000000000000 ) ;
#9685 = EDGE_CURVE ( 'NONE', #21231, #11786, #21528, .T. ) ;
#9686 = ORIENTED_EDGE ( 'NONE', *, *, #26712, .T. ) ;
#9687 = CARTESIAN_POINT ( 'NONE',  ( -4.934616302121927505E-14, 69.00000000546236834, 32.50000000000000000 ) ) ;
#9688 = CARTESIAN_POINT ( 'NONE',  ( 10.37757302488624767, 69.72500000273117848, 31.93888565452638417 ) ) ;
#9689 = CARTESIAN_POINT ( 'NONE',  ( 26.00068869287340334, 37.06510416666666430, -15.01150461594642316 ) ) ;
#9690 = CARTESIAN_POINT ( 'NONE',  ( 24.50000000000000000, 14.00000000000001243, 0.000000000000000000 ) ) ;
#9691 = DIRECTION ( 'NONE',  ( 0.000000000000000000, -1.000000000000000000, 0.000000000000000000 ) ) ;
#9692 = CARTESIAN_POINT ( 'NONE',  ( 27.16883889988623935, 8.325000002731176352, -19.73931689729374384 ) ) ;
#9693 = CARTESIAN_POINT ( 'NONE',  ( 5.779280353836490358E-15, 60.49999999999998579, 32.49999999999999289 ) ) ;
#9694 = CARTESIAN_POINT ( 'NONE',  ( 28.00173670424535644, 56.39545166574268364, -7.543491769121920321 ) ) ;
#9695 = CARTESIAN_POINT ( 'NONE',  ( -9.270509831248421762, 76.30000000000001137, 12.75976212528060039 ) ) ;
#9696 = CARTESIAN_POINT ( 'NONE',  ( -20.50609665440969209, 55.82812499999999289, 20.50609665441005092 ) ) ;
#9697 = DIRECTION ( 'NONE',  ( -0.000000000000000000, -1.000000000000000000, -0.000000000000000000 ) ) ;
#9698 = CARTESIAN_POINT ( 'NONE',  ( -1.778240108872766143E-15, 62.00000000546238255, -32.49999999999999289 ) ) ;
#9699 = CARTESIAN_POINT ( 'NONE',  ( -15.14183272437242600, 15.04999999453763238, 20.84094480462497856 ) ) ;
#9700 = CARTESIAN_POINT ( 'NONE',  ( 9.270509831248425314, 76.95000000546239960, 12.75976212528059683 ) ) ;
#9701 = CARTESIAN_POINT ( 'NONE',  ( -2.428612866367529427E-13, 19.30468749999999645, -27.95245687107222921 ) ) ;
#9702 = CARTESIAN_POINT ( 'NONE',  ( -20.75514604977248112, 35.42500000273119554, 28.56700777964554661 ) ) ;
#9703 = CARTESIAN_POINT ( 'NONE',  ( -10.37757302488624411, 76.72500000273117848, -31.93888565452638417 ) ) ;
#9704 = CARTESIAN_POINT ( 'NONE',  ( -33.58253175000000113, 45.37500000273119127, 0.000000000000000000 ) ) ;
#9705 = CARTESIAN_POINT ( 'NONE',  ( 6.486482029760648627E-15, 23.87500000273118417, 35.31076352940722529 ) ) ;
#9706 = DIRECTION ( 'NONE',  ( -1.000000000000000000, -1.309225264888156377E-16, 0.000000000000000000 ) ) ;
#9707 = CARTESIAN_POINT ( 'NONE',  ( -4.405589869732278832E-13, 9.000000005462366559, 32.50000000000000000 ) ) ;
#9708 = DIRECTION ( 'NONE',  ( 0.7202789989107551971, -0.6936844842780615084, 0.000000000000000000 ) ) ;
#9709 = CARTESIAN_POINT ( 'NONE',  ( 32.50000000000000000, 59.09999999999999432, -10.55989012756945833 ) ) ;
#9710 = CARTESIAN_POINT ( 'NONE',  ( 1.507698388325705758E-15, 9.124999997268822938, -24.62258325217400312 ) ) ;
#9711 = CARTESIAN_POINT ( 'NONE',  ( 33.58253175000000113, 62.12500000273119127, -4.112674001490185761E-15 ) ) ;
#9712 = CARTESIAN_POINT ( 'NONE',  ( -4.523095164977116484E-15, 2.624999997268825158, 24.62258325217400312 ) ) ;
#9713 = CARTESIAN_POINT ( 'NONE',  ( -14.01125832528328985, 38.20534749907601935, -24.18731323226223040 ) ) ;
#9714 = CARTESIAN_POINT ( 'NONE',  ( -10.37757302488624411, 14.72500000273119269, -31.93888565452638417 ) ) ;
#9715 = CARTESIAN_POINT ( 'NONE',  ( -23.41746824999999887, 12.12499999726882116, -2.867812753649727150E-15 ) ) ;
#9716 = CARTESIAN_POINT ( 'NONE',  ( 13.97622843553633665, 65.42447916666667140, 24.20753774853730889 ) ) ;
#9717 = ORIENTED_EDGE ( 'NONE', *, *, #16366, .F. ) ;
#9718 = CARTESIAN_POINT ( 'NONE',  ( -20.75514604977248823, 48.82500000273117280, -28.56700777964554305 ) ) ;
#9719 = CARTESIAN_POINT ( 'NONE',  ( -20.75514604977248112, 23.67500000273118843, 28.56700777964554661 ) ) ;
#9720 = ORIENTED_EDGE ( 'NONE', *, *, #24746, .F. ) ;
#9721 = CARTESIAN_POINT ( 'NONE',  ( -28.01184896238304134, 32.33854166666666430, -7.505752307972844761 ) ) ;
#9722 = CARTESIAN_POINT ( 'NONE',  ( -25.98046417659859486, 33.91965250092398065, -15.04653450569291628 ) ) ;
#9723 = CARTESIAN_POINT ( 'NONE',  ( -10.04305231718579172, 79.60000000000000853, -30.90933677959248982 ) ) ;
#9724 = CARTESIAN_POINT ( 'NONE',  ( -24.50000000000000711, 8.849999994537624204, 7.960532557706201828 ) ) ;
#9725 = CARTESIAN_POINT ( 'NONE',  ( -18.94512977948576093, 6.324999997268820451, 13.76444248337722698 ) ) ;
#9726 = CARTESIAN_POINT ( 'NONE',  ( 14.47279130897151589, 10.32499999726881335, 19.92008829642072953 ) ) ;
#9727 = CARTESIAN_POINT ( 'NONE',  ( -20.75514604977248823, 19.07500000273118701, -28.56700777964554305 ) ) ;
#9728 = CARTESIAN_POINT ( 'NONE',  ( 32.50000000000000000, 27.60000000546238752, -10.55989012756945833 ) ) ;
#9729 = CARTESIAN_POINT ( 'NONE',  ( -32.50000000000000000, 64.00000000000000000, 0.000000000000000000 ) ) ;
#9730 = FACE_OUTER_BOUND ( 'NONE', #27660, .T. ) ;
#9731 = CARTESIAN_POINT ( 'NONE',  ( 32.50000000000000000, 66.99999999999998579, -3.980102097228898626E-15 ) ) ;
#9732 = CARTESIAN_POINT ( 'NONE',  ( 26.02091320914851025, 62.56548583425730925, -14.97647472619946463 ) ) ;
#9733 = CARTESIAN_POINT ( 'NONE',  ( 10.37757302488624767, 33.97500000273117848, 31.93888565452638417 ) ) ;
#9734 = CARTESIAN_POINT ( 'NONE',  ( -32.50000000000000000, 32.40000000546238113, -10.55989012756945300 ) ) ;
#9735 = CARTESIAN_POINT ( 'NONE',  ( -20.50609665441004736, 29.18749999999999645, -20.50609665440969565 ) ) ;
#9736 = DIRECTION ( 'NONE',  ( 0.000000000000000000, 0.000000000000000000, 1.000000000000000000 ) ) ;
#9737 = CARTESIAN_POINT ( 'NONE',  ( 7.236395654485760609, 17.52499999726880731, -22.27133577429736633 ) ) ;
#9738 = CARTESIAN_POINT ( 'NONE',  ( 6.277390505771533514E-15, 10.49999999999998757, 34.17252228774368916 ) ) ;
#9739 = CARTESIAN_POINT ( 'NONE',  ( 5.147494310547217289, 9.051254287009214750, 32.50000000000007105 ) ) ;
#9740 = CARTESIAN_POINT ( 'NONE',  ( 19.06425588902558133, 56.10899333240935505, -19.11951029504797006 ) ) ;
#9741 = CARTESIAN_POINT ( 'NONE',  ( 33.58253175000000823, 56.02500000273117564, 10.91162601494192863 ) ) ;
#9742 = CARTESIAN_POINT ( 'NONE',  ( -2.162160676586881955E-15, 60.87500000273116996, -35.31076352940723240 ) ) ;
#9743 = CARTESIAN_POINT ( 'NONE',  ( 27.16883889988623935, 42.57500000273117990, -19.73931689729374384 ) ) ;
#9744 = CARTESIAN_POINT ( 'NONE',  ( -4.523095164977117273E-15, 16.12499999726880517, 24.62258325217400312 ) ) ;
#9745 = CARTESIAN_POINT ( 'NONE',  ( -33.58253175000000113, 79.25000000273118417, 0.000000000000000000 ) ) ;
#9746 = CARTESIAN_POINT ( 'NONE',  ( -5.147494310547423346, 6.448745718453161579, 32.50000000000000000 ) ) ;
#9747 = CARTESIAN_POINT ( 'NONE',  ( 14.01125832528286352, 48.52902750092398065, -24.18731323226246843 ) ) ;
#9748 = CARTESIAN_POINT ( 'NONE',  ( -15.12631959005131321, 16.99999999999998579, -18.67163132193408259 ) ) ;
#9749 = CYLINDRICAL_SURFACE ( 'NONE', #18808, 32.50000000000000000 ) ;
#9750 = CARTESIAN_POINT ( 'NONE',  ( -33.58253175000000113, 23.12500000273119838, 0.000000000000000000 ) ) ;
#9751 = DIRECTION ( 'NONE',  ( -0.000000000000000000, -1.000000000000000000, -0.000000000000000000 ) ) ;
#9752 = CARTESIAN_POINT ( 'NONE',  ( -2.375766604868044585, 78.69874572391550771, 14.99999999999999822 ) ) ;
#9753 = CARTESIAN_POINT ( 'NONE',  ( 0.000000000000000000, 80.00000000000001421, 0.000000000000000000 ) ) ;
#9754 = CARTESIAN_POINT ( 'NONE',  ( -26.02091320914878025, 61.98138916574268364, -14.97647472619899389 ) ) ;
#9755 = CARTESIAN_POINT ( 'NONE',  ( -32.50000000000000000, 42.60000000546238397, 10.55989012756946366 ) ) ;
#9756 = CARTESIAN_POINT ( 'NONE',  ( -2.571758278209442450E-15, -1.999999999999998224, 0.000000000000000000 ) ) ;
#9757 = CARTESIAN_POINT ( 'NONE',  ( -20.75514604977248823, 32.82500000273118701, -28.56700777964554305 ) ) ;
#9758 = CARTESIAN_POINT ( 'NONE',  ( 20.75514604977248467, 64.67500000273118133, -28.56700777964554305 ) ) ;
#9759 = CARTESIAN_POINT ( 'NONE',  ( -24.20753774853730889, 31.90885416666666430, 13.97622843553633842 ) ) ;
#9760 = ORIENTED_EDGE ( 'NONE', *, *, #6694, .T. ) ;
#9761 = CARTESIAN_POINT ( 'NONE',  ( 10.37757302488624767, 67.72500000273116427, 31.93888565452638417 ) ) ;
#9762 = CARTESIAN_POINT ( 'NONE',  ( 7.505752307973351023, 41.50520833333333570, 28.01184896238290278 ) ) ;
#9763 = VECTOR ( 'NONE', #13178, 1000.000000000000000 ) ;
#9764 = CARTESIAN_POINT ( 'NONE',  ( 0.000000000000000000, 102.0000000000000284, 0.000000000000000000 ) ) ;
#9765 = EDGE_LOOP ( 'NONE', ( #32664, #28126, #33399, #21516 ) ) ;
#9766 = CARTESIAN_POINT ( 'NONE',  ( -30.02300923189239867, 61.13319416759063785, -0.04044903254991731589 ) ) ;
#9767 = CARTESIAN_POINT ( 'NONE',  ( -27.95245687107223986, 57.69569416759065206, -0.04044903254993292840 ) ) ;
#9768 = CARTESIAN_POINT ( 'NONE',  ( 10.37757302488624056, 10.52500000273119696, -31.93888565452638417 ) ) ;
#9769 =( BOUNDED_CURVE ( )  B_SPLINE_CURVE ( 2, ( #32718, #12130, #11626, #25177, #32389, #6985, #14214, #16959, #1655, #33056, #20039, #30484, #17468 ),
 .UNSPECIFIED., .F., .T. ) 
 B_SPLINE_CURVE_WITH_KNOTS ( ( 3, 2, 2, 2, 2, 2, 3 ),
 ( 0.3910256410256410242, 0.3923076923076923017, 0.3948717948717948567, 0.3974358974358974117, 0.4000000000000000222, 0.4025641025641025772, 0.4038461538461538547 ),
 .UNSPECIFIED. ) 
 CURVE ( )  GEOMETRIC_REPRESENTATION_ITEM ( )  RATIONAL_B_SPLINE_CURVE ( ( 0.9755282581475768211, 0.9755282581475768211, 1.000000000000000000, 0.9510565162951535312, 1.000000000000000000, 0.9510565162951535312, 1.000000000000000000, 0.9510565162951535312, 1.000000000000000000, 0.9510565162951535312, 1.000000000000000000, 0.9755282581475768211, 0.9755282581475768211 ) ) 
 REPRESENTATION_ITEM ( '' )  );
#9770 = CARTESIAN_POINT ( 'NONE',  ( 20.53372385742108008, 15.71836833240935327, 20.47846945139866648 ) ) ;
#9771 = CARTESIAN_POINT ( 'NONE',  ( 15.00000000000000355, 79.15000000546235981, 4.873795443493592394 ) ) ;
#9772 = CARTESIAN_POINT ( 'NONE',  ( 27.16883889988624290, 40.17500000273119554, 19.73931689729373673 ) ) ;
#9773 = CARTESIAN_POINT ( 'NONE',  ( -20.08610463437157989, 46.20000000546237828, -27.64615127144129758 ) ) ;
#9774 =( BOUNDED_CURVE ( )  B_SPLINE_CURVE ( 2, ( #26329, #20854, #10213, #28728, #15706, #33884, #25988, #31300, #2817, #23760, #2131, #30961, #7459 ),
 .UNSPECIFIED., .F., .T. ) 
 B_SPLINE_CURVE_WITH_KNOTS ( ( 3, 2, 2, 2, 2, 2, 3 ),
 ( 0.8141025641025640969, 0.8153846153846153744, 0.8179487179487179294, 0.8205128205128204844, 0.8230769230769230393, 0.8256410256410255943, 0.8269230769230769829 ),
 .UNSPECIFIED. ) 
 CURVE ( )  GEOMETRIC_REPRESENTATION_ITEM ( )  RATIONAL_B_SPLINE_CURVE ( ( 0.9755282581475768211, 0.9755282581475768211, 1.000000000000000000, 0.9510565162951535312, 1.000000000000000000, 0.9510565162951535312, 1.000000000000000000, 0.9510565162951535312, 1.000000000000000000, 0.9510565162951535312, 1.000000000000000000, 0.9755282581475757109, 0.9755282581475768211 ) ) 
 REPRESENTATION_ITEM ( '' )  );
#9775 = CARTESIAN_POINT ( 'NONE',  ( 2.897257156509938333E-15, 78.49999999999994316, 15.77193336357400710 ) ) ;
#9776 = CARTESIAN_POINT ( 'NONE',  ( 10.37757302488624056, 26.52500000273119696, -31.93888565452638417 ) ) ;
#9777 = CARTESIAN_POINT ( 'NONE',  ( 7.570916362186213000, 14.14999999453761603, -23.30088464923126423 ) ) ;
#9778 = CARTESIAN_POINT ( 'NONE',  ( 27.16883889988624290, 56.17500000273118133, 19.73931689729373673 ) ) ;
#9779 =( NAMED_UNIT ( * ) PLANE_ANGLE_UNIT ( ) SI_UNIT ( $, .RADIAN. ) );
#9780 = EDGE_CURVE ( 'NONE', #10039, #15956, #17913, .T. ) ;
#9781 = CARTESIAN_POINT ( 'NONE',  ( 32.50000000000000000, 27.09999999999999076, -10.55989012756945833 ) ) ;
#9782 = CARTESIAN_POINT ( 'NONE',  ( 6.277390505771533514E-15, 24.50000000000001421, 34.17252228774368916 ) ) ;
#9783 = CARTESIAN_POINT ( 'NONE',  ( -18.94512977948575738, 15.42499999726881832, -13.76444248337723231 ) ) ;
#9784 = CARTESIAN_POINT ( 'NONE',  ( -20.75514604977248112, 75.42500000273120975, 28.56700777964554661 ) ) ;
#9785 = MANIFOLD_SOLID_BREP ( 'Cavity1', #15578 ) ;
#9786 = CARTESIAN_POINT ( 'NONE',  ( -1.778240108872766143E-15, 70.00000000546238255, -32.49999999999999289 ) ) ;
#9787 = CARTESIAN_POINT ( 'NONE',  ( -5.147494310547430452, 20.05125428700922185, -32.49999999999999289 ) ) ;
#9788 = CARTESIAN_POINT ( 'NONE',  ( -27.16883889988623935, 61.57500000273119412, 19.73931689729374739 ) ) ;
#9789 = CARTESIAN_POINT ( 'NONE',  ( -12.13525491562420910, 78.45000000546237118, 8.816778784387098611 ) ) ;
#9790 = EDGE_CURVE ( 'NONE', #30951, #6130, #17044, .T. ) ;
#9791 = EDGE_CURVE ( 'NONE', #12563, #33486, #25540, .T. ) ;
#9792 = CARTESIAN_POINT ( 'NONE',  ( 0.000000000000000000, -12.99999999999999822, 0.000000000000000000 ) ) ;
#9793 = CARTESIAN_POINT ( 'NONE',  ( -33.58253175000000113, 19.02500000273118630, -10.91162601494193218 ) ) ;
#9794 = CARTESIAN_POINT ( 'NONE',  ( -24.50000000000001066, 12.84999999453761532, 7.960532557706201828 ) ) ;
#9795 = CARTESIAN_POINT ( 'NONE',  ( -26.06988505166735237, 20.02642333425731280, -7.025853678916388567 ) ) ;
#9796 = CARTESIAN_POINT ( 'NONE',  ( 10.04305231718579705, 46.60000000000000142, 30.90933677959248982 ) ) ;
#9797 = CARTESIAN_POINT ( 'NONE',  ( -10.37757302488623701, 41.52500000273119696, 31.93888565452638417 ) ) ;
#9798 = CARTESIAN_POINT ( 'NONE',  ( -2.162160676586881955E-15, 4.875000002731200155, -35.31076352940723240 ) ) ;
#9799 = CARTESIAN_POINT ( 'NONE',  ( 10.37757302488624056, 56.77500000273121117, -31.93888565452638417 ) ) ;
#9800 = CARTESIAN_POINT ( 'NONE',  ( -14.97647472619946285, 51.39361083425730925, -26.02091320914851025 ) ) ;
#9801 = CARTESIAN_POINT ( 'NONE',  ( 10.04305231718579705, 3.100000005462372421, 30.90933677959248982 ) ) ;
#9802 = CARTESIAN_POINT ( 'NONE',  ( -28.02196122052058413, 37.77565999907600514, -7.468012846824272799 ) ) ;
#9803 = CARTESIAN_POINT ( 'NONE',  ( 32.50000000000000000, 63.60000000546238397, -10.55989012756945833 ) ) ;
#9804 = CARTESIAN_POINT ( 'NONE',  ( -13.91746824999999532, 72.77500000273120406, -4.522059556121115875 ) ) ;
#9805 = CARTESIAN_POINT ( 'NONE',  ( 19.06425588902558133, 62.98399333240935505, -19.11951029504797006 ) ) ;
#9806 = CARTESIAN_POINT ( 'NONE',  ( 0.000000000000000000, 80.00000000000001421, 0.000000000000000000 ) ) ;
#9807 = CARTESIAN_POINT ( 'NONE',  ( 32.50000000000000000, 77.50000000546236834, -3.980102097228898626E-15 ) ) ;
#9808 = DIRECTION ( 'NONE',  ( -0.5000000000000000000, 0.000000000000000000, -0.8660254037844385966 ) ) ;
#9809 = CARTESIAN_POINT ( 'NONE',  ( 33.58253175000000113, 34.37500000273117706, -4.112674001490185761E-15 ) ) ;
#9810 = CARTESIAN_POINT ( 'NONE',  ( -7.236395654485763274, 10.52499999726880198, 22.27133577429736633 ) ) ;
#9811 = ORIENTED_EDGE ( 'NONE', *, *, #4319, .T. ) ;
#9812 = CARTESIAN_POINT ( 'NONE',  ( 20.75514604977248467, 72.67500000273118133, -28.56700777964554305 ) ) ;
#9813 = CARTESIAN_POINT ( 'NONE',  ( -20.08610463437156923, 22.80000000546236194, 27.64615127144130113 ) ) ;
#9814 = CARTESIAN_POINT ( 'NONE',  ( 30.02300923189239512, 47.66406249999998579, -2.619432448724977703E-13 ) ) ;
#9815 = CARTESIAN_POINT ( 'NONE',  ( -32.50000000000000000, 62.50000000546238255, 0.000000000000000000 ) ) ;
#9816 = ORIENTED_EDGE ( 'NONE', *, *, #24940, .T. ) ;
#9817 = CARTESIAN_POINT ( 'NONE',  ( -26.29305231718578995, 10.70000000546239605, 19.10302069950538595 ) ) ;
#9818 = CARTESIAN_POINT ( 'NONE',  ( -33.58253175000000113, 47.22500000273117138, 10.91162601494193929 ) ) ;
#9819 = CARTESIAN_POINT ( 'NONE',  ( -7.236395654485757944, 15.22499999726881192, -22.27133577429736988 ) ) ;
#9820 = CARTESIAN_POINT ( 'NONE',  ( -32.50000000000000000, 6.600000005462382191, 10.55989012756946366 ) ) ;
#9821 = CARTESIAN_POINT ( 'NONE',  ( -5.147494310547430452, 7.551254281546841085, -32.49999999999999289 ) ) ;
#9822 = DIRECTION ( 'NONE',  ( 0.000000000000000000, 0.000000000000000000, -1.000000000000000000 ) ) ;
#9823 = CARTESIAN_POINT ( 'NONE',  ( -32.50000000000000000, 50.09999999999998721, 10.55989012756946366 ) ) ;
#9824 = CARTESIAN_POINT ( 'NONE',  ( -1.778240108872766143E-15, 10.00000000546236834, -32.49999999999999289 ) ) ;
#9825 = CARTESIAN_POINT ( 'NONE',  ( 20.75514604977249178, 18.07500000273119056, 28.56700777964553950 ) ) ;
#9826 = CARTESIAN_POINT ( 'NONE',  ( 0.000000000000000000, 0.000000000000000000, 0.000000000000000000 ) ) ;
#9827 = CARTESIAN_POINT ( 'NONE',  ( 6.950374756619257965, 24.88503499907601935, -26.09010956794244507 ) ) ;
#9828 = CARTESIAN_POINT ( 'NONE',  ( 11.25946833292375793, 78.57500000273121543, -8.180482586598735395 ) ) ;
#9829 = DIRECTION ( 'NONE',  ( -0.2583678462756388572, 0.9660466117175131595, 0.000000000000000000 ) ) ;
#9830 = FACE_OUTER_BOUND ( 'NONE', #1767, .T. ) ;
#9831 = CARTESIAN_POINT ( 'NONE',  ( 20.08610463437158344, 2.700000000000001954, 27.64615127144129403 ) ) ;
#9832 = ORIENTED_EDGE ( 'NONE', *, *, #27334, .F. ) ;
#9833 = CARTESIAN_POINT ( 'NONE',  ( -7.236395654485763274, 16.52499999726880731, 22.27133577429736633 ) ) ;
#9834 = CARTESIAN_POINT ( 'NONE',  ( -18.94512977948576093, 1.824999997268816898, 13.76444248337722698 ) ) ;
#9835 = CARTESIAN_POINT ( 'NONE',  ( -19.09188309203694445, 46.37500000000000000, -19.09188309203661049 ) ) ;
#9836 = CARTESIAN_POINT ( 'NONE',  ( 20.75514604977249178, 59.82500000273117280, 28.56700777964553950 ) ) ;
#9837 = CARTESIAN_POINT ( 'NONE',  ( -33.58253175000000113, 25.47500000273118914, 10.91162601494193929 ) ) ;
#9838 = CARTESIAN_POINT ( 'NONE',  ( 10.37757302488624056, 10.77500000273116854, -31.93888565452638417 ) ) ;
#9839 = CARTESIAN_POINT ( 'NONE',  ( 19.09188309203661049, 30.04687500000000000, -19.09188309203694445 ) ) ;
#9840 = CARTESIAN_POINT ( 'NONE',  ( 27.16883889988624290, 2.175000002731186655, 19.73931689729373673 ) ) ;
#9841 = CARTESIAN_POINT ( 'NONE',  ( -28.00173670424549499, 20.02642333425731280, -7.543491769121417612 ) ) ;
#9842 = CARTESIAN_POINT ( 'NONE',  ( -20.50609665440969209, 59.26562500000000000, 20.50609665441005092 ) ) ;
#9843 = CARTESIAN_POINT ( 'NONE',  ( 33.58253175000000113, 4.125000002731193938, -4.112674001490185761E-15 ) ) ;
#9844 = EDGE_CURVE ( 'NONE', #24911, #29266, #14638, .T. ) ;
#9845 = CARTESIAN_POINT ( 'NONE',  ( -11.25946833292375793, 71.57500000273120122, 8.180482586598737171 ) ) ;
#9846 = CARTESIAN_POINT ( 'NONE',  ( -32.50000000000000000, 39.89999999999999858, -10.55989012756945478 ) ) ;
#9847 = CARTESIAN_POINT ( 'NONE',  ( -33.58253175000000113, 45.12500000273117706, 0.000000000000000000 ) ) ;
#9848 = CARTESIAN_POINT ( 'NONE',  ( 14.47279130897151589, 4.324999997268801799, 19.92008829642072953 ) ) ;
#9849 = PLANE ( 'NONE',  #33079 ) ;
#9850 = ORIENTED_EDGE ( 'NONE', *, *, #13566, .F. ) ;
#9851 = CARTESIAN_POINT ( 'NONE',  ( -33.58253175000000113, 57.27500000273120406, -10.91162601494193218 ) ) ;
#9852 = CARTESIAN_POINT ( 'NONE',  ( -5.147494310547423346, 4.948745723915524586, 32.50000000000000000 ) ) ;
#9853 = CARTESIAN_POINT ( 'NONE',  ( -24.18731323226248264, 33.91965250092398065, -14.01125832528284931 ) ) ;
#9854 = CARTESIAN_POINT ( 'NONE',  ( 10.37757302488624056, 74.77500000273118985, -31.93888565452638417 ) ) ;
#9855 = ORIENTED_EDGE ( 'NONE', *, *, #19956, .F. ) ;
#9856 = CARTESIAN_POINT ( 'NONE',  ( -27.16883889988623935, 29.32500000273117990, 19.73931689729374739 ) ) ;
#9857 = CARTESIAN_POINT ( 'NONE',  ( 15.01150461594596308, 16.15364583333333215, -26.00068869287367335 ) ) ;
#9858 = ORIENTED_EDGE ( 'NONE', *, *, #2571, .F. ) ;
#9859 = FACE_OUTER_BOUND ( 'NONE', #22768, .T. ) ;
#9860 = CARTESIAN_POINT ( 'NONE',  ( -33.58253175000000113, 65.22500000273117848, 10.91162601494193929 ) ) ;
#9861 = CARTESIAN_POINT ( 'NONE',  ( -28.01184896238290278, 42.36458333333332860, 7.505752307973363457 ) ) ;
#9862 = CARTESIAN_POINT ( 'NONE',  ( 7.570916362186213000, 14.39999999999999680, -23.30088464923126423 ) ) ;
#9863 = CARTESIAN_POINT ( 'NONE',  ( 23.41746824999999887, 1.124999997268810725, 0.000000000000000000 ) ) ;
#9864 = CARTESIAN_POINT ( 'NONE',  ( -20.75514604977248823, 12.82500000273118168, -28.56700777964554305 ) ) ;
#9865 = DIRECTION ( 'NONE',  ( -1.000000000000000000, -1.224646799147353454E-16, 0.000000000000000000 ) ) ;
#9866 = CARTESIAN_POINT ( 'NONE',  ( -7.543491769121917656, 48.66107666574268364, -28.00173670424536354 ) ) ;
#9867 = CARTESIAN_POINT ( 'NONE',  ( -1.778240108872766143E-15, 37.50000000000000000, -32.49999999999999289 ) ) ;
#9868 = CARTESIAN_POINT ( 'NONE',  ( 30.02300923189239867, 64.85156249999997158, -2.619432448724978208E-13 ) ) ;
#9869 = CARTESIAN_POINT ( 'NONE',  ( 26.29305231718579350, 22.79999999999998650, 19.10302069950537529 ) ) ;
#9870 = CARTESIAN_POINT ( 'NONE',  ( 1.577395562988744260E-15, 14.24999999453762989, -25.76082449383753925 ) ) ;
#9871 = CARTESIAN_POINT ( 'NONE',  ( -4.635254915624211769, 77.85000000546237686, -14.26584774442730286 ) ) ;
#9872 = CARTESIAN_POINT ( 'NONE',  ( 19.09188309203661049, 19.73437500000000000, -19.09188309203694445 ) ) ;
#9873 =( BOUNDED_CURVE ( )  B_SPLINE_CURVE ( 2, ( #21546, #13018, #10442, #5292, #31993, #28117, #25549, #2195, #27523, #14152, #3679, #24609, #14485, #1425, #22212, #24773, #22045, #26854, #1251, #11401, #29578, #9154, #8991, #32659, #8489, #8656, #14317, #29921, #32490, #24446, #3513, #19637, #21878, #922, #19141, #11731, #17062, #6080, #13820, #30080, #16563, #3350, #24288, #1083, #5923, #760, #11241, #6586, #4010, #24941, #19471, #32163, #11903, #22375, #18976, #29421, #29746, #27016, #16400, #21718, #13984, #32328, #8819, #19304, #6252, #6424, #16731, #27187, #11563, #16896, #27358, #3843, #28378, #1591, #23061, #9672, #10024, #17747, #25801, #33168, #20497, #6752, #22890, #2292, #4350, #14656, #19799, #12242, #4867, #7443, #27692, #22539, #2117, #14826, #30249, #33520, #30946, #15347, #9845, #25638, #17405 ),
 .UNSPECIFIED., .F., .T. ) 
 B_SPLINE_CURVE_WITH_KNOTS ( ( 3, 2, 2, 2, 2, 2, 2, 2, 2, 2, 2, 2, 2, 2, 2, 2, 2, 2, 2, 2, 2, 2, 2, 2, 2, 2, 2, 2, 2, 2, 2, 2, 2, 2, 2, 2, 2, 2, 2, 2, 2, 2, 2, 2, 2, 2, 2, 2, 2, 2, 3 ),
 ( 0.000000000000000000, 0.02000000000000000042, 0.04000000000000000083, 0.05999999999999999778, 0.08000000000000000167, 0.1000000000000000056, 0.1199999999999999956, 0.1400000000000000133, 0.1600000000000000033, 0.1799999999999999933, 0.2000000000000000111, 0.2200000000000000011, 0.2399999999999999911, 0.2600000000000000089, 0.2800000000000000266, 0.2999999999999999889, 0.3200000000000000067, 0.3400000000000000244, 0.3599999999999999867, 0.3800000000000000044, 0.4000000000000000222, 0.4199999999999999845, 0.4400000000000000022, 0.4600000000000000200, 0.4799999999999999822, 0.5000000000000000000, 0.5200000000000000178, 0.5400000000000000355, 0.5600000000000000533, 0.5799999999999999600, 0.5999999999999999778, 0.6199999999999999956, 0.6400000000000000133, 0.6600000000000000311, 0.6800000000000000488, 0.6999999999999999556, 0.7199999999999999734, 0.7399999999999999911, 0.7600000000000000089, 0.7800000000000000266, 0.8000000000000000444, 0.8199999999999999512, 0.8399999999999999689, 0.8599999999999999867, 0.8800000000000000044, 0.9000000000000000222, 0.9200000000000000400, 0.9399999999999999467, 0.9599999999999999645, 0.9799999999999999822, 1.000000000000000000 ),
 .UNSPECIFIED. ) 
 CURVE ( )  GEOMETRIC_REPRESENTATION_ITEM ( )  RATIONAL_B_SPLINE_CURVE ( ( 1.000000000000000000, 0.9510565162951535312, 1.000000000000000000, 0.9510565162951535312, 1.000000000000000000, 0.9510565162951535312, 1.000000000000000000, 0.9510565162951535312, 1.000000000000000000, 0.9510565162951535312, 1.000000000000000000, 0.9510565162951535312, 1.000000000000000000, 0.9510565162951535312, 1.000000000000000000, 0.9510565162951535312, 1.000000000000000000, 0.9510565162951535312, 1.000000000000000000, 0.9510565162951535312, 1.000000000000000000, 0.9510565162951535312, 1.000000000000000000, 0.9510565162951535312, 1.000000000000000000, 0.9510565162951535312, 1.000000000000000000, 0.9510565162951535312, 1.000000000000000000, 0.9510565162951535312, 1.000000000000000000, 0.9510565162951535312, 1.000000000000000000, 0.9510565162951535312, 1.000000000000000000, 0.9510565162951535312, 1.000000000000000000, 0.9510565162951535312, 1.000000000000000000, 0.9510565162951535312, 1.000000000000000000, 0.9510565162951535312, 1.000000000000000000, 0.9510565162951535312, 1.000000000000000000, 0.9510565162951535312, 1.000000000000000000, 0.9510565162951535312, 1.000000000000000000, 0.9510565162951535312, 1.000000000000000000, 0.9510565162951535312, 1.000000000000000000, 0.9510565162951535312, 1.000000000000000000, 0.9510565162951535312, 1.000000000000000000, 0.9510565162951535312, 1.000000000000000000, 0.9510565162951535312, 1.000000000000000000, 0.9510565162951535312, 1.000000000000000000, 0.9510565162951535312, 1.000000000000000000, 0.9510565162951535312, 1.000000000000000000, 0.9510565162951535312, 1.000000000000000000, 0.9510565162951535312, 1.000000000000000000, 0.9510565162951535312, 1.000000000000000000, 0.9510565162951535312, 1.000000000000000000, 0.9510565162951535312, 1.000000000000000000, 0.9510565162951535312, 1.000000000000000000, 0.9510565162951535312, 1.000000000000000000, 0.9510565162951535312, 1.000000000000000000, 0.9510565162951535312, 1.000000000000000000, 0.9510565162951535312, 1.000000000000000000, 0.9510565162951535312, 1.000000000000000000, 0.9510565162951535312, 1.000000000000000000, 0.9510565162951535312, 1.000000000000000000, 0.9510565162951535312, 1.000000000000000000, 0.9510565162951535312, 1.000000000000000000, 0.9510565162951535312, 1.000000000000000000, 0.9510565162951535312, 1.000000000000000000 ) ) 
 REPRESENTATION_ITEM ( '' )  );
#9874 = CARTESIAN_POINT ( 'NONE',  ( 20.75514604977248467, 28.42500000273118133, -28.56700777964554305 ) ) ;
#9875 = CARTESIAN_POINT ( 'NONE',  ( 2.688165632520823219E-15, 71.37500000273119838, 14.63369212191046387 ) ) ;
#9876 = CARTESIAN_POINT ( 'NONE',  ( 10.37757302488624767, 41.97500000273117138, 31.93888565452638417 ) ) ;
#9877 = CARTESIAN_POINT ( 'NONE',  ( 27.16883889988623935, 22.57500000273118701, -19.73931689729374384 ) ) ;
#9878 = CARTESIAN_POINT ( 'NONE',  ( -26.29305231718579350, 12.30000000546238681, -19.10302069950537884 ) ) ;
#9879 = CARTESIAN_POINT ( 'NONE',  ( 27.16883889988624290, 73.92500000273119554, 19.73931689729373673 ) ) ;
#9880 = EDGE_CURVE ( 'NONE', #25888, #14943, #27167, .T. ) ;
#9881 = CARTESIAN_POINT ( 'NONE',  ( -5.147494310547423346, 66.44874571845315359, 32.50000000000000000 ) ) ;
#9882 = CARTESIAN_POINT ( 'NONE',  ( 26.29305231718579350, 62.80000000000001137, 19.10302069950537529 ) ) ;
#9883 = CARTESIAN_POINT ( 'NONE',  ( 0.000000000000000000, 52.00000000000000711, 0.000000000000000000 ) ) ;
#9884 = CARTESIAN_POINT ( 'NONE',  ( 10.37757302488624056, 62.52500000273120406, -31.93888565452638417 ) ) ;
#9885 = PRODUCT_DEFINITION_FORMATION_WITH_SPECIFIED_SOURCE ( 'ANY', '', #27642, .NOT_KNOWN. ) ;
#9886 = EDGE_CURVE ( 'NONE', #26574, #33508, #11712, .T. ) ;
#9887 = CARTESIAN_POINT ( 'NONE',  ( -7.236395654485757944, 1.724999997268800156, -22.27133577429736988 ) ) ;
#9888 = CARTESIAN_POINT ( 'NONE',  ( 19.11951029504797006, 39.78086833240934794, 19.06425588902558133 ) ) ;
#9889 = CARTESIAN_POINT ( 'NONE',  ( 27.16883889988623935, 76.57500000273120122, -19.73931689729374384 ) ) ;
#9890 = CARTESIAN_POINT ( 'NONE',  ( 20.75514604977248467, 4.425000002731183990, -28.56700777964554305 ) ) ;
#9891 = CARTESIAN_POINT ( 'NONE',  ( -18.94512977948576093, 12.32499999726882578, 13.76444248337722698 ) ) ;
#9892 = CARTESIAN_POINT ( 'NONE',  ( -6.988114217768288228, 63.84895833333332860, -26.07999730980477437 ) ) ;
#9893 = VERTEX_POINT ( 'NONE', #32642 ) ;
#9894 = CARTESIAN_POINT ( 'NONE',  ( 33.58253175000000113, 48.12500000273119127, -4.112674001490185761E-15 ) ) ;
#9895 = CARTESIAN_POINT ( 'NONE',  ( -20.75514604977248112, 21.67500000273119554, 28.56700777964554661 ) ) ;
#9896 = ORIENTED_EDGE ( 'NONE', *, *, #23857, .T. ) ;
#9897 = CARTESIAN_POINT ( 'NONE',  ( 26.00068869287367335, 34.20052083333332860, 15.01150461594596308 ) ) ;
#9898 = CARTESIAN_POINT ( 'NONE',  ( 15.04653450569292872, 31.34152750092398421, -25.98046417659857710 ) ) ;
#9899 = DIRECTION ( 'NONE',  ( -0.000000000000000000, -1.000000000000000000, -0.000000000000000000 ) ) ;
#9900 = CARTESIAN_POINT ( 'NONE',  ( -32.50000000000000000, 72.40000000546238823, -10.55989012756945300 ) ) ;
#9901 = CARTESIAN_POINT ( 'NONE',  ( 14.47279130897151589, 4.824999997268814234, 19.92008829642072953 ) ) ;
#9902 = CARTESIAN_POINT ( 'NONE',  ( 23.41746825000000243, 12.52499999726880375, 7.608796670333735079 ) ) ;
#9903 = CARTESIAN_POINT ( 'NONE',  ( 20.75514604977249178, 18.07500000273119056, 28.56700777964553950 ) ) ;
#9904 = CARTESIAN_POINT ( 'NONE',  ( -32.50000000000000000, 24.40000000546237047, -10.55989012756945478 ) ) ;
#9905 = CARTESIAN_POINT ( 'NONE',  ( 6.277390505771533514E-15, 66.49999999999998579, 34.17252228774368916 ) ) ;
#9906 = CARTESIAN_POINT ( 'NONE',  ( 19.82091636218621034, 11.54999999453762349, 14.40073868116559730 ) ) ;
#9907 = CARTESIAN_POINT ( 'NONE',  ( -12.90513655866680587, 66.99999999999998579, -31.00393344628902881 ) ) ;
#9908 = CARTESIAN_POINT ( 'NONE',  ( -28.01184896238304134, 15.15104166666666252, -7.505752307972844761 ) ) ;
#9909 = CARTESIAN_POINT ( 'NONE',  ( -20.75514604977248112, 29.67500000273119909, 28.56700777964554661 ) ) ;
#9910 = CARTESIAN_POINT ( 'NONE',  ( 20.08610463437158344, 43.20000000546236407, 27.64615127144129403 ) ) ;
#9911 = CARTESIAN_POINT ( 'NONE',  ( -30.02300923189239867, 35.63281249999999289, 2.654126918244514854E-13 ) ) ;
#9912 = CARTESIAN_POINT ( 'NONE',  ( 0.000000000000000000, 0.000000000000000000, 0.000000000000000000 ) ) ;
#9913 = CARTESIAN_POINT ( 'NONE',  ( -23.41746824999999887, 14.12499999726882294, -2.867812753649727150E-15 ) ) ;
#9914 =( BOUNDED_SURFACE ( )  B_SPLINE_SURFACE ( 1, 2, ( 
 ( #236, #10722, #31644, #18631, #5059, #15544, #5572, #31811, #33892, #31143, #2489, #12958, #26171, #2431, #30563, #28345, #7229, #15141, #33313, #23374, #18059, #20808, #30736, #20119, #4316, #4830, #7060, #20461, #15310, #12899, #25769, #17542, #23199, #33661, #10159, #30912, #17715, #2084, #28002, #25605, #1909, #33487, #25938, #33835, #12386, #5001, #28173, #4489, #23030, #28504, #4661, #20289, #31252, #31084, #7580, #9988, #14965, #12559, #2255, #22681, #15484, #12729, #25431, #10332, #7406, #20641, #22855, #9812, #17892, #17370, #27833, #14791, #25255, #1730, #12210, #33132, #9636, #23383, #9997, #10505, #2616, #20817, #28688, #18581, #17901, #31093, #13079, #7925, #28856, #15669, #31261, #28515, #23553, #10169, #20983, #5186, #26291, #7415, #31432, #20653, #2266, #5524, #23719, #5011, #21153, #5354, #185, #31594, #25947, #16, #15834, #26119, #8094, #18410, #2780, #7590, #13246, #29022, #18067, #15493, #10673, #2441, #20470, #16004, #26459, #2950, #13422, #25778, #33846, #23889, #30922, #28354, #4840, #15321, #12739, #23210, #12909, #33672, #10341, #7755, #18242, #27292, #8593, #10844, #24224, #8758, #31930, #24387, #27124, #19078, #19409, #29857, #19242, #13753, #26628, #11180, #11013, #694, #8926, #31762, #21483, #21817, #8422, #21651, #32266, #3451, #29680, #3122, #32097, #16172, #16837, #861, #6185, #3285, #26793, #6358, #11341, #13594, #526, #21981, #32430, #29517, #6021, #21322, #13922, #16497, #360, #5859, #16337, #16667, #18912, #26952, #1019, #3617, #14091, #14255, #24548, #11502, #3784, #24058, #8254, #18747, #5694, #29189, #29358, #1361, #7200, #14593, #20088, #11840, #24880, #22318, #27803, #12007, #22478, #32926, #1189, #9425, #24712, #30532, #11671, #32762, #17512, #3950, #27973, #30025, #9257, #22153, #4456, #9095, #14933, #32596, #9778, #20260, #30704, #27632, #12179, #1876, #25399, #7029, #4287, #19577, #1533, #4119, #19910, #30359, #6861, #14761, #17340, #6529, #17002, #12354, #25052, #14425, #17681, #22823, #30187, #27459, #28143, #19742, #1701, #25224, #22650, #6690, #4629, #33282, #17174, #33102, #9606, #2053, #26081, #4799, #18203, #2577, #10635, #13042, #15278, #20944, #31393, #7883, #28645, #15452, #33808, #25739, #12869, #33630, #31223, #23680, #145, #10129, #2740, #28479, #23513, #12528, #10302, #4975, #18373, #2219, #12698, #23347, #23168, #30878, #20779, #7716, #5142, #2401, #22996, #33455, #28818, #25907, #20611, #31557, #15796, #31056, #9954, #21113, #28311, #33972, #15630, #10466, #7548, #8054, #26252, #18540, #5314, #17859, #20429, #13203, #18033, #28985, #15108, #25573, #7375, #29147, #11304, #21782, #32230, #19041, #5821, #24182, #5652, #3248, #24017, #21612, #14050, #24511, #489, #27084, #18869, #13885, #26419, #654, #29318, #8719, #16134, #26589, #13716, #13554, #21285, #31889, #983, #5984, #18710, #3085, #3578, #11468, #16297, #11143, #2913, #29480, #26755, #5484, #10971, #21446, #823, #8385, #32057, #6144, #8557, #16461, #19372, #19202, #29641, #26914, #3412, #24351, #16629, #10805, #21942, #32392, #8887, #15963, #13381, #23853, #317, #31726, #8217, #32884, #17131, #27587, #4076, #6319, #14551, #29816, #25180, #16795, #3911, #22605, #9056, #33059, #1147, #16962, #27253, #9564, #14217, #20042, #3745, #14892, #25353, #1832, #32721, #17297, #6988, #30487, #12133, #9383, #24673, #6650, #9217, #25010, #6816, #19701, #1492, #11800, #12310, #17471, #33234, #30146, #32557, #11629, #27758, #19536, #19865, #4246, #22782, #14720, #29984, #1658, #27931, #4415, #30319, #11966, #22437, #6489, #9733, #14380, #22113, #27420, #24839, #1317, #22278, #33585, #29064, #7156, #5402, #10086, #26505, #20386, #7329, #28900, #28271, #2009, #12651, #16219, #21198, #33412, #30837, #8299, #18791, #20565, #15878, #17639, #233, #7507, #20219, #25697, #2178, #16051, #17813, #26335, #21365, #31010, #23121, #571, #405, #10892, #13293, #9909, #2824, #5569, #25532, #31808, #2998, #4757, #3169, #17991, #13471, #15234, #23766, #10719, #31641, #8139, #18628, #23936, #30659, #29235, #28100, #5740, #4588, #26674, #13639, #24103, #15064, #12485, #22954, #21527, #3825, #29403, #14299, #18958, #30063, #6569, #17043, #13964, #32470, #22195, #24756, #27339, #24591, #5905, #21861, #24426, #32308, #16712, #8801, #1064, #19283, #8473, #16382, #1233, #903, #737, #27504, #11711, #16543, #26835, #3994, #24270, #32641, #9136, #19618, #11544, #3331, #29726, #11385, #6232, #27166, #3659, #22026, #14135, #13801, #11223, #14466, #8971, #21697, #24923, #11062, #26996, #32143, #31975, #8637, #19454, #29899, #6402, #3494, #19122, #29559, #6060, #16876, #4164, #22357, #12400, #25097, #4502, #22870, #30928, #33328, #1574, #7241, #17730, #28187, #14977, #1744, #20133, #12051, #33149, #19958, #17558, #10004, #20477, #30406, #23043, #14806, #9825, #32804, #30578, #25271, #4675, #22521, #32972, #9653, #9476, #17216, #27850, #7421, #1923, #14637, #6904, #33501, #17907, #12224, #7074, #9297, #25447, #22697, #1408, #17385, #4333, #30752, #28015, #20302, #2099, #15154, #25619, #15328, #12572, #28360, #4847, #11886, #19781, #30231, #6734, #27675, #192, #2448, #8261, #15677, #21160, #12914, #25955, #23390, #28863, #13085, #23559, #23, #2272, #10512, #25783, #31602, #12745, #33852, #18587, #5017, #29027, #31099, #10347, #23219, #5530, #10177, #16011, #33678, #10852, #21327, #31768, #28695, #13252, #20989, #20824, #7596, #18248, #18753, #26297, #15499, #31268, #13427, #23895, #26125, #31439, #20659, #5360, #7931, #18073, #7762, #5193, #8100, #2622, #18419, #26465, #15840, #2786, #5701, #2958, #366, #23726, #10679, #29195, #28522, #21489, #6363, #24552, #26798, #32600, #6024, #11506, #3292, #16342, #13757, #19245, #3454, #13926, #24390, #26634, #864, #16179, #21986, #3128, #24228, #8932, #29364, #19413, #31936, #698, #13601, #29862, #532, #16841, #24066, #1194, #11675, #22158, #19081, #3622, #27297, #3789, #32434, #29684, #11019, #26955, #29521, #11345, #21822, #32269, #6189, #8763, #8429, #18918, #14260, #16502, #5864, #9100, #24717, #21655, #11185, #19581, #32100, #27128, #16671, #14096, #8598, #30029, #1025 ),
 ( #25578, #1538, #28148, #19916, #14938, #27465, #25231, #30364, #12359, #6695, #27636, #17344, #25056, #33108, #17178, #17516, #1705, #22827, #3955, #7033, #4124, #32768, #2057, #20264, #12013, #17688, #1881, #30710, #4634, #22482, #9611, #25403, #12184, #15113, #22654, #20092, #14599, #9784, #12533, #32931, #9430, #30537, #6865, #6534, #27977, #23002, #33459, #4462, #22323, #27807, #33287, #9958, #24884, #7204, #14429, #20434, #17007, #4291, #1367, #14766, #19746, #11844, #9262, #30192, #7380, #20784, #5320, #28483, #20949, #23685, #5147, #15968, #26424, #15800, #10306, #23173, #7721, #7553, #31229, #5489, #28316, #18038, #18377, #4979, #18208, #28822, #33977, #26256, #33635, #28651, #12702, #13385, #31398, #2744, #33813, #12874, #15634, #2918, #23858, #25743, #13208, #10810, #10471, #25913, #26086, #30884, #2582, #150, #323, #17864, #10639, #15283, #4804, #15457, #20616, #13046, #23518, #7888, #2406, #23351, #21118, #31561, #8059, #18544, #28990, #2225, #10134, #31060, #21786, #13890, #32062, #5988, #29823, #29151, #8389, #24357, #19210, #6149, #26920, #8562, #31730, #29485, #21290, #16634, #8221, #29323, #14056, #493, #24518, #26593, #18874, #18715, #988, #5657, #11473, #16139, #6327, #16804, #27260, #24187, #8726, #32398, #21947, #3584, #827, #3090, #19046, #659, #16465, #3416, #11308, #32234, #29647, #13561, #24024, #8893, #11147, #10976, #3751, #19377, #26760, #21450, #14225, #31893, #27090, #21618, #24681, #3252, #1155, #5825, #16304, #13722, #14391, #32564, #22614, #1327, #14728, #33067, #7165, #9573, #11808, #17478, #27940, #4423, #25189, #11976, #30327, #22286, #9390, #30154, #27768, #20227, #30667, #6658, #33243, #25019, #20049, #9063, #6823, #1499, #14898, #32731, #9224, #19874, #19708, #27427, #4085, #17647, #12141, #24847, #17141, #9741, #28108, #22444, #17305, #19544, #1666, #32891, #11637, #27594, #14559, #6996, #4253, #30495, #12320, #25362, #1840, #25539, #22790, #4595, #15072, #22121, #29992, #6496, #16969, #3918, #10433, #12660, #18509, #25872, #31359, #23129, #2186, #33595, #5110, #23311, #33776, #33942, #4936, #18000, #15418, #8023, #10603, #30846, #20908, #15932, #15594, #31017, #10267, #2018, #2364, #23480, #21081, #31530, #5282, #20395, #28955, #20574, #25705, #20749, #18168, #28610, #7515, #10095, #26048, #31192, #7851, #15765, #28445, #13008, #12837, #12493, #2541, #18339, #7682, #28784, #5451, #9918, #26219, #2711, #13172, #23650, #112, #22962, #33420, #7337, #17822, #28278, #4765, #15243, #23820, #26885, #26556, #18678, #21909, #6112, #10940, #3543, #21750, #16594, #14015, #8350, #19007, #11274, #21580, #24478, #8523, #29451, #3052, #29610, #952, #23986, #13523, #5953, #458, #26388, #3382, #11432, #32359, #24318, #8188, #5786, #13852, #8853, #10774, #27050, #286, #32026, #19334, #18840, #791, #26724, #5621, #29779, #6284, #622, #2880, #16267, #32195, #21415, #16433, #19173, #11110, #13347, #21251, #8689, #3219, #29118, #13687, #31858, #24151, #31695, #16105, #29286, #4214, #14349, #17096, #14688, #19831, #25147, #9022, #27554, #32522, #33199, #6785, #20182, #30113, #19504, #3712, #27726, #6455, #30283, #1623, #12275, #12101, #16929, #22572, #33022, #9528, #17263, #4042, #1458, #27387, #14516, #1284, #32853, #25322, #1796, #11763, #4381, #6617, #20009, #14182, #11936, #24975, #30456, #3876, #24806, #22405, #22245, #29951, #9184, #22748, #6953, #32689, #19668, #14856, #9702, #9348, #17437, #24638, #27899, #30626, #16760, #27219, #1112, #11597, #22077, #12796, #7810, #7477, #10052, #21040, #20870, #31318, #33731, #30801, #15377, #26005, #12452, #18299, #15552, #17779, #23606, #30976, #2497, #28237, #7294, #4723, #10229, #28407, #4897, #25832, #17604, #2322, #7123, #12966, #28066, #15203, #33901, #20352, #10392, #22922, #25667, #4553, #28744, #25497, #5241, #15032, #26179, #2674, #13132, #20533, #28571, #15724, #73, #23440, #20709, #1977, #17958, #23269, #31151, #7642, #18126, #5068, #10561, #33378, #9874, #2146, #12621, #23088, #33552, #32154, #3010, #26346, #16554, #10731, #8482, #21375, #29245, #13482, #3504, #8647, #5915, #11393, #11071, #26516, #5749, #31490, #31820, #18969, #6070, #27007, #747, #15890, #13974, #16061, #21208, #16230, #13649, #24114, #23947, #18639, #21537, #18801, #16392, #11232, #416, #29414, #10903, #7980, #31985, #581, #8310, #26684, #24437, #5411, #29076, #26845, #3341, #13811, #3180, #24279, #21708, #19132, #31653, #29569, #914, #18467, #28910, #2835, #8150, #23779, #13304, #246, #5580, #33465, #17694, #12539, #9965, #4297, #14944, #7211, #17522, #20440, #4470, #25410, #32481, #25583, #30891, #19464, #22037, #1887, #8982, #21870, #33293, #7386, #17870, #20269, #3671, #1712, #9793, #28321, #6242, #2063, #19294, #27983, #4810, #14772, #30716, #22661, #1075, #23010, #15289, #30544, #32320, #12190, #28154, #29913, #12365, #15119, #7040, #25749, #2233, #4640, #33114, #14145, #9616, #6415, #20098, #8811, #29738, #16887, #16723, #27350, #22833, #27178, #24601, #11555, #25237, #13051, #28487, #29157, #2749, #10646, #15639, #28658, #26090, #18721, #21296, #7558, #15465, #33642, #23690, #2413, #15805, #155, #8227, #21123, #12879, #18549, #28994, #5494, #26261, #23523, #31403, #23356, #10476, #31234, #28827, #31736, #5663, #7726, #330, #2587, #31566, #10139, #7897, #33982, #15973, #33817, #10311, #20954, #20789, #4984, #5154, #16146, #13213, #25918, #18214, #10816, #26599, #18381, #5325, #20621, #8064, #26429, #12708, #2922, #13391, #23863, #23179, #31063, #18043, #3420, #5993, #16973, #16808, #27264, #29651, #26766, #11311, #21952, #8394, #3755, #11477, #13727, #19548, #26924, #32401, #24192, #3257, #664, #6154, #24361, #831, #21790, #13567, #32238, #3096, #8897, #24030, #11152, #29827, #16310, #6331, #18880, #21623, #499, #14229, #21456, #24685, #10982, #22125, #32568, #9067, #16469, #24522, #1160, #11641, #19381, #16638, #31899, #13894, #8731, #19215, #27094, #3587, #14060, #992, #29329, #5831, #29996, #6500, #32066, #8566, #19050, #29489, #22290, #12499, #6663, #4428, #17310, #25193, #9394, #33426, #28113, #30851, #6828, #4258, #4089 ) ),
 .UNSPECIFIED., .F., .F., .T. ) 
 B_SPLINE_SURFACE_WITH_KNOTS ( ( 2, 2 ),
 ( 3, 2, 2, 2, 2, 2, 2, 2, 2, 2, 2, 2, 2, 2, 2, 2, 2, 2, 2, 2, 2, 2, 2, 2, 2, 2, 2, 2, 2, 2, 2, 2, 2, 2, 2, 2, 2, 2, 2, 2, 2, 2, 2, 2, 2, 2, 2, 2, 2, 2, 2, 2, 2, 2, 2, 2, 2, 2, 2, 2, 2, 2, 2, 2, 2, 2, 2, 2, 2, 2, 2, 2, 2, 2, 2, 2, 2, 2, 2, 2, 2, 2, 2, 2, 2, 2, 2, 2, 2, 2, 2, 2, 2, 2, 2, 2, 2, 2, 2, 2, 2, 2, 2, 2, 2, 2, 2, 2, 2, 2, 2, 2, 2, 2, 2, 2, 2, 2, 2, 2, 2, 2, 2, 2, 2, 2, 2, 2, 2, 2, 2, 2, 2, 2, 2, 2, 2, 2, 2, 2, 2, 2, 2, 2, 2, 2, 2, 2, 2, 2, 2, 2, 2, 2, 2, 2, 2, 2, 2, 2, 2, 2, 2, 2, 2, 2, 2, 2, 2, 2, 2, 2, 2, 2, 2, 2, 2, 2, 2, 2, 2, 2, 2, 2, 2, 2, 2, 2, 2, 2, 2, 2, 2, 2, 2, 2, 2, 2, 2, 2, 2, 2, 2, 2, 2, 2, 2, 2, 2, 2, 2, 2, 2, 2, 2, 2, 2, 2, 2, 2, 2, 2, 2, 2, 2, 2, 2, 2, 2, 2, 2, 2, 2, 2, 2, 2, 2, 2, 2, 2, 2, 2, 2, 2, 2, 2, 2, 2, 2, 2, 2, 2, 2, 2, 2, 2, 2, 2, 2, 2, 2, 2, 2, 2, 2, 2, 2, 2, 2, 2, 2, 2, 2, 2, 2, 2, 2, 2, 2, 2, 2, 2, 2, 2, 2, 2, 2, 2, 2, 2, 2, 2, 2, 2, 2, 2, 2, 2, 2, 2, 2, 2, 2, 2, 2, 2, 2, 2, 2, 2, 2, 2, 2, 2, 2, 2, 2, 2, 2, 2, 2, 2, 2, 2, 2, 2, 2, 2, 2, 2, 2, 2, 2, 2, 2, 2, 2, 2, 2, 2, 2, 2, 2, 2, 2, 2, 2, 2, 2, 2, 2, 2, 2, 2, 2, 2, 2, 2, 2, 2, 2, 2, 2, 2, 2, 2, 2, 2, 2, 2, 2, 2, 2, 2, 2, 2, 2, 2, 2, 2, 2, 2, 2, 2, 2, 2, 2, 2, 2, 2, 3 ),
 ( 0.000000000000000000, 1.000000000000000000 ),
 ( 0.000000000000000000, 0.002564102564102564100, 0.005128205128205128201, 0.007692307692307692735, 0.01025641025641025640, 0.01282051282051282007, 0.01538461538461538547, 0.01794871794871794740, 0.02051282051282051280, 0.02307692307692307820, 0.02564102564102564014, 0.02820512820512820554, 0.03076923076923077094, 0.03333333333333333287, 0.03589743589743589480, 0.03846153846153846367, 0.04102564102564102561, 0.04358974358974358754, 0.04615384615384615641, 0.04871794871794871834, 0.05128205128205128027, 0.05384615384615384914, 0.05641025641025641107, 0.05897435897435897301, 0.06153846153846154188, 0.06410256410256409687, 0.06666666666666666574, 0.06923076923076923461, 0.07179487179487178961, 0.07435897435897435848, 0.07692307692307692735, 0.07948717948717948234, 0.08205128205128205121, 0.08461538461538462008, 0.08717948717948717507, 0.08974358974358974395, 0.09230769230769231282, 0.09487179487179486781, 0.09743589743589743668, 0.1000000000000000056, 0.1025641025641025605, 0.1051282051282051294, 0.1076923076923076983, 0.1102564102564102533, 0.1128205128205128221, 0.1153846153846153910, 0.1179487179487179460, 0.1205128205128205149, 0.1230769230769230838, 0.1256410256410256387, 0.1282051282051281937, 0.1307692307692307765, 0.1333333333333333315, 0.1358974358974358865, 0.1384615384615384692, 0.1410256410256410242, 0.1435897435897435792, 0.1461538461538461620, 0.1487179487179487170, 0.1512820512820512719, 0.1538461538461538547, 0.1564102564102564097, 0.1589743589743589647, 0.1615384615384615474, 0.1641025641025641024, 0.1666666666666666574, 0.1692307692307692402, 0.1717948717948717952, 0.1743589743589743501, 0.1769230769230769329, 0.1794871794871794879, 0.1820512820512820429, 0.1846153846153846256, 0.1871794871794871806, 0.1897435897435897356, 0.1923076923076923184, 0.1948717948717948734, 0.1974358974358974284, 0.2000000000000000111, 0.2025641025641025661, 0.2051282051282051211, 0.2076923076923077038, 0.2102564102564102588, 0.2128205128205128138, 0.2153846153846153966, 0.2179487179487179516, 0.2205128205128205066, 0.2230769230769230893, 0.2256410256410256443, 0.2282051282051281993, 0.2307692307692307820, 0.2333333333333333370, 0.2358974358974358920, 0.2384615384615384748, 0.2410256410256410298, 0.2435897435897435848, 0.2461538461538461675, 0.2487179487179487225, 0.2512820512820512775, 0.2538461538461538325, 0.2564102564102563875, 0.2589743589743589980, 0.2615384615384615530, 0.2641025641025641080, 0.2666666666666666630, 0.2692307692307692180, 0.2717948717948717730, 0.2743589743589743835, 0.2769230769230769384, 0.2794871794871794934, 0.2820512820512820484, 0.2846153846153846034, 0.2871794871794871584, 0.2897435897435897689, 0.2923076923076923239, 0.2948717948717948789, 0.2974358974358974339, 0.2999999999999999889, 0.3025641025641025439, 0.3051282051282051544, 0.3076923076923077094, 0.3102564102564102644, 0.3128205128205128194, 0.3153846153846153744, 0.3179487179487179294, 0.3205128205128205399, 0.3230769230769230949, 0.3256410256410256499, 0.3282051282051282048, 0.3307692307692307598, 0.3333333333333333148, 0.3358974358974358698, 0.3384615384615384803, 0.3410256410256410353, 0.3435897435897435903, 0.3461538461538461453, 0.3487179487179487003, 0.3512820512820512553, 0.3538461538461538658, 0.3564102564102564208, 0.3589743589743589758, 0.3615384615384615308, 0.3641025641025640858, 0.3666666666666666408, 0.3692307692307692513, 0.3717948717948718063, 0.3743589743589743613, 0.3769230769230769162, 0.3794871794871794712, 0.3820512820512820262, 0.3846153846153846367, 0.3871794871794871917, 0.3897435897435897467, 0.3923076923076923017, 0.3948717948717948567, 0.3974358974358974117, 0.4000000000000000222, 0.4025641025641025772, 0.4051282051282051322, 0.4076923076923076872, 0.4102564102564102422, 0.4128205128205127972, 0.4153846153846154077, 0.4179487179487179627, 0.4205128205128205177, 0.4230769230769230727, 0.4256410256410256276, 0.4282051282051281826, 0.4307692307692307931, 0.4333333333333333481, 0.4358974358974359031, 0.4384615384615384581, 0.4410256410256410131, 0.4435897435897435681, 0.4461538461538461786, 0.4487179487179487336, 0.4512820512820512886, 0.4538461538461538436, 0.4564102564102563986, 0.4589743589743589536, 0.4615384615384615641, 0.4641025641025641191, 0.4666666666666666741, 0.4692307692307692291, 0.4717948717948717841, 0.4743589743589743390, 0.4769230769230769496, 0.4794871794871795045, 0.4820512820512820595, 0.4846153846153846145, 0.4871794871794871695, 0.4897435897435897245, 0.4923076923076923350, 0.4948717948717948900, 0.4974358974358974450, 0.5000000000000000000, 0.5025641025641025550, 0.5051282051282051100, 0.5076923076923076650, 0.5102564102564102200, 0.5128205128205127750, 0.5153846153846153300, 0.5179487179487179960, 0.5205128205128205510, 0.5230769230769231060, 0.5256410256410256610, 0.5282051282051282159, 0.5307692307692307709, 0.5333333333333333259, 0.5358974358974358809, 0.5384615384615384359, 0.5410256410256409909, 0.5435897435897435459, 0.5461538461538461009, 0.5487179487179487669, 0.5512820512820513219, 0.5538461538461538769, 0.5564102564102564319, 0.5589743589743589869, 0.5615384615384615419, 0.5641025641025640969, 0.5666666666666666519, 0.5692307692307692069, 0.5717948717948717618, 0.5743589743589743168, 0.5769230769230768718, 0.5794871794871795379, 0.5820512820512820928, 0.5846153846153846478, 0.5871794871794872028, 0.5897435897435897578, 0.5923076923076923128, 0.5948717948717948678, 0.5974358974358974228, 0.5999999999999999778, 0.6025641025641025328, 0.6051282051282050878, 0.6076923076923076428, 0.6102564102564103088, 0.6128205128205128638, 0.6153846153846154188, 0.6179487179487179738, 0.6205128205128205288, 0.6230769230769230838, 0.6256410256410256387, 0.6282051282051281937, 0.6307692307692307487, 0.6333333333333333037, 0.6358974358974358587, 0.6384615384615384137, 0.6410256410256410797, 0.6435897435897436347, 0.6461538461538461897, 0.6487179487179487447, 0.6512820512820512997, 0.6538461538461538547, 0.6564102564102564097, 0.6589743589743589647, 0.6615384615384615197, 0.6641025641025640747, 0.6666666666666666297, 0.6692307692307691847, 0.6717948717948717396, 0.6743589743589744057, 0.6769230769230769607, 0.6794871794871795156, 0.6820512820512820706, 0.6846153846153846256, 0.6871794871794871806, 0.6897435897435897356, 0.6923076923076922906, 0.6948717948717948456, 0.6974358974358974006, 0.6999999999999999556, 0.7025641025641025106, 0.7051282051282051766, 0.7076923076923077316, 0.7102564102564102866, 0.7128205128205128416, 0.7153846153846153966, 0.7179487179487179516, 0.7205128205128205066, 0.7230769230769230616, 0.7256410256410256165, 0.7282051282051281715, 0.7307692307692307265, 0.7333333333333332815, 0.7358974358974359475, 0.7384615384615385025, 0.7410256410256410575, 0.7435897435897436125, 0.7461538461538461675, 0.7487179487179487225, 0.7512820512820512775, 0.7538461538461538325, 0.7564102564102563875, 0.7589743589743589425, 0.7615384615384614975, 0.7641025641025640525, 0.7666666666666667185, 0.7692307692307692735, 0.7717948717948718285, 0.7743589743589743835, 0.7769230769230769384, 0.7794871794871794934, 0.7820512820512820484, 0.7846153846153846034, 0.7871794871794871584, 0.7897435897435897134, 0.7923076923076922684, 0.7948717948717948234, 0.7974358974358974894, 0.8000000000000000444, 0.8025641025641025994, 0.8051282051282051544, 0.8076923076923077094, 0.8102564102564102644, 0.8128205128205128194, 0.8153846153846153744, 0.8179487179487179294, 0.8205128205128204844, 0.8230769230769230393, 0.8256410256410255943, 0.8282051282051282604, 0.8307692307692308153, 0.8333333333333333703, 0.8358974358974359253, 0.8384615384615384803, 0.8410256410256410353, 0.8435897435897435903, 0.8461538461538461453, 0.8487179487179487003, 0.8512820512820512553, 0.8538461538461538103, 0.8564102564102563653, 0.8589743589743589203, 0.8615384615384615863, 0.8641025641025641413, 0.8666666666666666963, 0.8692307692307692513, 0.8717948717948718063, 0.8743589743589743613, 0.8769230769230769162, 0.8794871794871794712, 0.8820512820512820262, 0.8846153846153845812, 0.8871794871794871362, 0.8897435897435896912, 0.8923076923076923572, 0.8948717948717949122, 0.8974358974358974672, 0.9000000000000000222, 0.9025641025641025772, 0.9051282051282051322, 0.9076923076923076872, 0.9102564102564102422, 0.9128205128205127972, 0.9153846153846153522, 0.9179487179487179072, 0.9205128205128204621, 0.9230769230769231282, 0.9256410256410256832, 0.9282051282051282382, 0.9307692307692307931, 0.9333333333333333481, 0.9358974358974359031, 0.9384615384615384581, 0.9410256410256410131, 0.9435897435897435681, 0.9461538461538461231, 0.9487179487179486781, 0.9512820512820512331, 0.9538461538461538991, 0.9564102564102564541, 0.9589743589743590091, 0.9615384615384615641, 0.9641025641025641191, 0.9666666666666666741, 0.9692307692307692291, 0.9717948717948717841, 0.9743589743589743390, 0.9769230769230768940, 0.9794871794871794490, 0.9820512820512820040, 0.9846153846153846700, 0.9871794871794872250, 0.9897435897435897800, 0.9923076923076923350, 0.9948717948717948900, 0.9974358974358974450, 1.000000000000000000 ),
 .UNSPECIFIED. ) 
 GEOMETRIC_REPRESENTATION_ITEM ( )  RATIONAL_B_SPLINE_SURFACE ( (
 ( 1.000000000000000000, 0.9510565162951535312, 1.000000000000000000, 0.9510565162951535312, 1.000000000000000000, 0.9510565162951535312, 1.000000000000000000, 0.9510565162951535312, 1.000000000000000000, 0.9510565162951535312, 1.000000000000000000, 0.9510565162951535312, 1.000000000000000000, 0.9510565162951535312, 1.000000000000000000, 0.9510565162951535312, 1.000000000000000000, 0.9510565162951535312, 1.000000000000000000, 0.9510565162951535312, 1.000000000000000000, 0.9510565162951535312, 1.000000000000000000, 0.9510565162951535312, 1.000000000000000000, 0.9510565162951535312, 1.000000000000000000, 0.9510565162951535312, 1.000000000000000000, 0.9510565162951535312, 1.000000000000000000, 0.9510565162951535312, 1.000000000000000000, 0.9510565162951535312, 1.000000000000000000, 0.9510565162951535312, 1.000000000000000000, 0.9510565162951535312, 1.000000000000000000, 0.9510565162951535312, 1.000000000000000000, 0.9510565162951535312, 1.000000000000000000, 0.9510565162951535312, 1.000000000000000000, 0.9510565162951535312, 1.000000000000000000, 0.9510565162951535312, 1.000000000000000000, 0.9510565162951535312, 1.000000000000000000, 0.9510565162951535312, 1.000000000000000000, 0.9510565162951535312, 1.000000000000000000, 0.9510565162951535312, 1.000000000000000000, 0.9510565162951535312, 1.000000000000000000, 0.9510565162951535312, 1.000000000000000000, 0.9510565162951535312, 1.000000000000000000, 0.9510565162951535312, 1.000000000000000000, 0.9510565162951535312, 1.000000000000000000, 0.9510565162951535312, 1.000000000000000000, 0.9510565162951535312, 1.000000000000000000, 0.9510565162951535312, 1.000000000000000000, 0.9510565162951535312, 1.000000000000000000, 0.9510565162951535312, 1.000000000000000000, 0.9510565162951535312, 1.000000000000000000, 0.9510565162951535312, 1.000000000000000000, 0.9510565162951535312, 1.000000000000000000, 0.9510565162951535312, 1.000000000000000000, 0.9510565162951535312, 1.000000000000000000, 0.9510565162951535312, 1.000000000000000000, 0.9510565162951535312, 1.000000000000000000, 0.9510565162951535312, 1.000000000000000000, 0.9510565162951535312, 1.000000000000000000, 0.9510565162951535312, 1.000000000000000000, 0.9510565162951535312, 1.000000000000000000, 0.9510565162951535312, 1.000000000000000000, 0.9510565162951535312, 1.000000000000000000, 0.9510565162951535312, 1.000000000000000000, 0.9510565162951535312, 1.000000000000000000, 0.9510565162951535312, 1.000000000000000000, 0.9510565162951535312, 1.000000000000000000, 0.9510565162951535312, 1.000000000000000000, 0.9510565162951535312, 1.000000000000000000, 0.9510565162951535312, 1.000000000000000000, 0.9510565162951535312, 1.000000000000000000, 0.9510565162951535312, 1.000000000000000000, 0.9510565162951535312, 1.000000000000000000, 0.9510565162951535312, 1.000000000000000000, 0.9510565162951535312, 1.000000000000000000, 0.9510565162951535312, 1.000000000000000000, 0.9510565162951535312, 1.000000000000000000, 0.9510565162951535312, 1.000000000000000000, 0.9510565162951535312, 1.000000000000000000, 0.9510565162951535312, 1.000000000000000000, 0.9510565162951535312, 1.000000000000000000, 0.9510565162951535312, 1.000000000000000000, 0.9510565162951535312, 1.000000000000000000, 0.9510565162951535312, 1.000000000000000000, 0.9510565162951535312, 1.000000000000000000, 0.9510565162951535312, 1.000000000000000000, 0.9510565162951535312, 1.000000000000000000, 0.9510565162951535312, 1.000000000000000000, 0.9510565162951535312, 1.000000000000000000, 0.9510565162951535312, 1.000000000000000000, 0.9510565162951535312, 1.000000000000000000, 0.9510565162951535312, 1.000000000000000000, 0.9510565162951535312, 1.000000000000000000, 0.9510565162951535312, 1.000000000000000000, 0.9510565162951535312, 1.000000000000000000, 0.9510565162951535312, 1.000000000000000000, 0.9510565162951535312, 1.000000000000000000, 0.9510565162951535312, 1.000000000000000000, 0.9510565162951535312, 1.000000000000000000, 0.9510565162951535312, 1.000000000000000000, 0.9510565162951535312, 1.000000000000000000, 0.9510565162951535312, 1.000000000000000000, 0.9510565162951535312, 1.000000000000000000, 0.9510565162951535312, 1.000000000000000000, 0.9510565162951535312, 1.000000000000000000, 0.9510565162951535312, 1.000000000000000000, 0.9510565162951535312, 1.000000000000000000, 0.9510565162951535312, 1.000000000000000000, 0.9510565162951535312, 1.000000000000000000, 0.9510565162951535312, 1.000000000000000000, 0.9510565162951535312, 1.000000000000000000, 0.9510565162951535312, 1.000000000000000000, 0.9510565162951535312, 1.000000000000000000, 0.9510565162951535312, 1.000000000000000000, 0.9510565162951535312, 1.000000000000000000, 0.9510565162951535312, 1.000000000000000000, 0.9510565162951535312, 1.000000000000000000, 0.9510565162951535312, 1.000000000000000000, 0.9510565162951535312, 1.000000000000000000, 0.9510565162951535312, 1.000000000000000000, 0.9510565162951535312, 1.000000000000000000, 0.9510565162951535312, 1.000000000000000000, 0.9510565162951535312, 1.000000000000000000, 0.9510565162951535312, 1.000000000000000000, 0.9510565162951535312, 1.000000000000000000, 0.9510565162951535312, 1.000000000000000000, 0.9510565162951535312, 1.000000000000000000, 0.9510565162951535312, 1.000000000000000000, 0.9510565162951535312, 1.000000000000000000, 0.9510565162951535312, 1.000000000000000000, 0.9510565162951535312, 1.000000000000000000, 0.9510565162951535312, 1.000000000000000000, 0.9510565162951535312, 1.000000000000000000, 0.9510565162951535312, 1.000000000000000000, 0.9510565162951535312, 1.000000000000000000, 0.9510565162951535312, 1.000000000000000000, 0.9510565162951535312, 1.000000000000000000, 0.9510565162951535312, 1.000000000000000000, 0.9510565162951535312, 1.000000000000000000, 0.9510565162951535312, 1.000000000000000000, 0.9510565162951535312, 1.000000000000000000, 0.9510565162951535312, 1.000000000000000000, 0.9510565162951535312, 1.000000000000000000, 0.9510565162951535312, 1.000000000000000000, 0.9510565162951535312, 1.000000000000000000, 0.9510565162951535312, 1.000000000000000000, 0.9510565162951535312, 1.000000000000000000, 0.9510565162951535312, 1.000000000000000000, 0.9510565162951535312, 1.000000000000000000, 0.9510565162951535312, 1.000000000000000000, 0.9510565162951535312, 1.000000000000000000, 0.9510565162951535312, 1.000000000000000000, 0.9510565162951535312, 1.000000000000000000, 0.9510565162951535312, 1.000000000000000000, 0.9510565162951535312, 1.000000000000000000, 0.9510565162951535312, 1.000000000000000000, 0.9510565162951535312, 1.000000000000000000, 0.9510565162951535312, 1.000000000000000000, 0.9510565162951535312, 1.000000000000000000, 0.9510565162951535312, 1.000000000000000000, 0.9510565162951535312, 1.000000000000000000, 0.9510565162951535312, 1.000000000000000000, 0.9510565162951535312, 1.000000000000000000, 0.9510565162951535312, 1.000000000000000000, 0.9510565162951535312, 1.000000000000000000, 0.9510565162951535312, 1.000000000000000000, 0.9510565162951535312, 1.000000000000000000, 0.9510565162951535312, 1.000000000000000000, 0.9510565162951535312, 1.000000000000000000, 0.9510565162951535312, 1.000000000000000000, 0.9510565162951535312, 1.000000000000000000, 0.9510565162951535312, 1.000000000000000000, 0.9510565162951535312, 1.000000000000000000, 0.9510565162951535312, 1.000000000000000000, 0.9510565162951535312, 1.000000000000000000, 0.9510565162951535312, 1.000000000000000000, 0.9510565162951535312, 1.000000000000000000, 0.9510565162951535312, 1.000000000000000000, 0.9510565162951535312, 1.000000000000000000, 0.9510565162951535312, 1.000000000000000000, 0.9510565162951535312, 1.000000000000000000, 0.9510565162951535312, 1.000000000000000000, 0.9510565162951535312, 1.000000000000000000, 0.9510565162951535312, 1.000000000000000000, 0.9510565162951535312, 1.000000000000000000, 0.9510565162951535312, 1.000000000000000000, 0.9510565162951535312, 1.000000000000000000, 0.9510565162951535312, 1.000000000000000000, 0.9510565162951535312, 1.000000000000000000, 0.9510565162951535312, 1.000000000000000000, 0.9510565162951535312, 1.000000000000000000, 0.9510565162951535312, 1.000000000000000000, 0.9510565162951535312, 1.000000000000000000, 0.9510565162951535312, 1.000000000000000000, 0.9510565162951535312, 1.000000000000000000, 0.9510565162951535312, 1.000000000000000000, 0.9510565162951535312, 1.000000000000000000, 0.9510565162951535312, 1.000000000000000000, 0.9510565162951535312, 1.000000000000000000, 0.9510565162951535312, 1.000000000000000000, 0.9510565162951535312, 1.000000000000000000, 0.9510565162951535312, 1.000000000000000000, 0.9510565162951535312, 1.000000000000000000, 0.9510565162951535312, 1.000000000000000000, 0.9510565162951535312, 1.000000000000000000, 0.9510565162951535312, 1.000000000000000000, 0.9510565162951535312, 1.000000000000000000, 0.9510565162951535312, 1.000000000000000000, 0.9510565162951535312, 1.000000000000000000, 0.9510565162951535312, 1.000000000000000000, 0.9510565162951535312, 1.000000000000000000, 0.9510565162951535312, 1.000000000000000000, 0.9510565162951535312, 1.000000000000000000, 0.9510565162951535312, 1.000000000000000000, 0.9510565162951535312, 1.000000000000000000, 0.9510565162951535312, 1.000000000000000000, 0.9510565162951535312, 1.000000000000000000, 0.9510565162951535312, 1.000000000000000000, 0.9510565162951535312, 1.000000000000000000, 0.9510565162951535312, 1.000000000000000000, 0.9510565162951535312, 1.000000000000000000, 0.9510565162951535312, 1.000000000000000000, 0.9510565162951535312, 1.000000000000000000, 0.9510565162951535312, 1.000000000000000000, 0.9510565162951535312, 1.000000000000000000, 0.9510565162951535312, 1.000000000000000000, 0.9510565162951535312, 1.000000000000000000, 0.9510565162951535312, 1.000000000000000000, 0.9510565162951535312, 1.000000000000000000, 0.9510565162951535312, 1.000000000000000000, 0.9510565162951535312, 1.000000000000000000, 0.9510565162951535312, 1.000000000000000000, 0.9510565162951535312, 1.000000000000000000, 0.9510565162951535312, 1.000000000000000000, 0.9510565162951535312, 1.000000000000000000, 0.9510565162951535312, 1.000000000000000000, 0.9510565162951535312, 1.000000000000000000, 0.9510565162951535312, 1.000000000000000000, 0.9510565162951535312, 1.000000000000000000, 0.9510565162951535312, 1.000000000000000000, 0.9510565162951535312, 1.000000000000000000, 0.9510565162951535312, 1.000000000000000000, 0.9510565162951535312, 1.000000000000000000, 0.9510565162951535312, 1.000000000000000000, 0.9510565162951535312, 1.000000000000000000, 0.9510565162951535312, 1.000000000000000000, 0.9510565162951535312, 1.000000000000000000, 0.9510565162951535312, 1.000000000000000000, 0.9510565162951535312, 1.000000000000000000, 0.9510565162951535312, 1.000000000000000000, 0.9510565162951535312, 1.000000000000000000, 0.9510565162951535312, 1.000000000000000000, 0.9510565162951535312, 1.000000000000000000, 0.9510565162951535312, 1.000000000000000000, 0.9510565162951535312, 1.000000000000000000, 0.9510565162951535312, 1.000000000000000000, 0.9510565162951535312, 1.000000000000000000, 0.9510565162951535312, 1.000000000000000000, 0.9510565162951535312, 1.000000000000000000, 0.9510565162951535312, 1.000000000000000000, 0.9510565162951535312, 1.000000000000000000, 0.9510565162951535312, 1.000000000000000000, 0.9510565162951535312, 1.000000000000000000, 0.9510565162951535312, 1.000000000000000000, 0.9510565162951535312, 1.000000000000000000, 0.9510565162951535312, 1.000000000000000000, 0.9510565162951535312, 1.000000000000000000, 0.9510565162951535312, 1.000000000000000000, 0.9510565162951535312, 1.000000000000000000, 0.9510565162951535312, 1.000000000000000000, 0.9510565162951535312, 1.000000000000000000, 0.9510565162951535312, 1.000000000000000000, 0.9510565162951535312, 1.000000000000000000, 0.9510565162951535312, 1.000000000000000000, 0.9510565162951535312, 1.000000000000000000, 0.9510565162951535312, 1.000000000000000000, 0.9510565162951535312, 1.000000000000000000, 0.9510565162951535312, 1.000000000000000000, 0.9510565162951535312, 1.000000000000000000, 0.9510565162951535312, 1.000000000000000000, 0.9510565162951535312, 1.000000000000000000, 0.9510565162951535312, 1.000000000000000000, 0.9510565162951535312, 1.000000000000000000, 0.9510565162951535312, 1.000000000000000000, 0.9510565162951535312, 1.000000000000000000, 0.9510565162951535312, 1.000000000000000000, 0.9510565162951535312, 1.000000000000000000, 0.9510565162951535312, 1.000000000000000000, 0.9510565162951535312, 1.000000000000000000, 0.9510565162951535312, 1.000000000000000000, 0.9510565162951535312, 1.000000000000000000, 0.9510565162951535312, 1.000000000000000000, 0.9510565162951535312, 1.000000000000000000, 0.9510565162951535312, 1.000000000000000000, 0.9510565162951535312, 1.000000000000000000, 0.9510565162951535312, 1.000000000000000000, 0.9510565162951535312, 1.000000000000000000, 0.9510565162951535312, 1.000000000000000000, 0.9510565162951535312, 1.000000000000000000, 0.9510565162951535312, 1.000000000000000000, 0.9510565162951535312, 1.000000000000000000, 0.9510565162951535312, 1.000000000000000000, 0.9510565162951535312, 1.000000000000000000, 0.9510565162951535312, 1.000000000000000000, 0.9510565162951535312, 1.000000000000000000, 0.9510565162951535312, 1.000000000000000000, 0.9510565162951535312, 1.000000000000000000, 0.9510565162951535312, 1.000000000000000000, 0.9510565162951535312, 1.000000000000000000, 0.9510565162951535312, 1.000000000000000000, 0.9510565162951535312, 1.000000000000000000, 0.9510565162951535312, 1.000000000000000000, 0.9510565162951535312, 1.000000000000000000, 0.9510565162951535312, 1.000000000000000000, 0.9510565162951535312, 1.000000000000000000, 0.9510565162951535312, 1.000000000000000000, 0.9510565162951535312, 1.000000000000000000, 0.9510565162951535312, 1.000000000000000000, 0.9510565162951535312, 1.000000000000000000, 0.9510565162951535312, 1.000000000000000000, 0.9510565162951535312, 1.000000000000000000, 0.9510565162951535312, 1.000000000000000000, 0.9510565162951535312, 1.000000000000000000, 0.9510565162951535312, 1.000000000000000000, 0.9510565162951535312, 1.000000000000000000, 0.9510565162951535312, 1.000000000000000000, 0.9510565162951535312, 1.000000000000000000, 0.9510565162951535312, 1.000000000000000000, 0.9510565162951535312, 1.000000000000000000, 0.9510565162951535312, 1.000000000000000000, 0.9510565162951535312, 1.000000000000000000, 0.9510565162951535312, 1.000000000000000000, 0.9510565162951535312, 1.000000000000000000, 0.9510565162951535312, 1.000000000000000000, 0.9510565162951535312, 1.000000000000000000, 0.9510565162951535312, 1.000000000000000000, 0.9510565162951535312, 1.000000000000000000, 0.9510565162951535312, 1.000000000000000000, 0.9510565162951535312, 1.000000000000000000, 0.9510565162951535312, 1.000000000000000000, 0.9510565162951535312, 1.000000000000000000, 0.9510565162951535312, 1.000000000000000000, 0.9510565162951535312, 1.000000000000000000, 0.9510565162951535312, 1.000000000000000000, 0.9510565162951535312, 1.000000000000000000, 0.9510565162951535312, 1.000000000000000000, 0.9510565162951535312, 1.000000000000000000, 0.9510565162951535312, 1.000000000000000000, 0.9510565162951535312, 1.000000000000000000, 0.9510565162951535312, 1.000000000000000000, 0.9510565162951535312, 1.000000000000000000, 0.9510565162951535312, 1.000000000000000000, 0.9510565162951535312, 1.000000000000000000, 0.9510565162951535312, 1.000000000000000000, 0.9510565162951535312, 1.000000000000000000, 0.9510565162951535312, 1.000000000000000000, 0.9510565162951535312, 1.000000000000000000, 0.9510565162951535312, 1.000000000000000000, 0.9510565162951535312, 1.000000000000000000, 0.9510565162951535312, 1.000000000000000000, 0.9510565162951535312, 1.000000000000000000, 0.9510565162951535312, 1.000000000000000000, 0.9510565162951535312, 1.000000000000000000, 0.9510565162951535312, 1.000000000000000000, 0.9510565162951535312, 1.000000000000000000, 0.9510565162951535312, 1.000000000000000000, 0.9510565162951535312, 1.000000000000000000, 0.9510565162951535312, 1.000000000000000000, 0.9510565162951535312, 1.000000000000000000, 0.9510565162951535312, 1.000000000000000000, 0.9510565162951535312, 1.000000000000000000, 0.9510565162951535312, 1.000000000000000000, 0.9510565162951535312, 1.000000000000000000, 0.9510565162951535312, 1.000000000000000000, 0.9510565162951535312, 1.000000000000000000, 0.9510565162951535312, 1.000000000000000000, 0.9510565162951535312, 1.000000000000000000, 0.9510565162951535312, 1.000000000000000000, 0.9510565162951535312, 1.000000000000000000, 0.9510565162951535312, 1.000000000000000000, 0.9510565162951535312, 1.000000000000000000, 0.9510565162951535312, 1.000000000000000000, 0.9510565162951535312, 1.000000000000000000, 0.9510565162951535312, 1.000000000000000000, 0.9510565162951535312, 1.000000000000000000, 0.9510565162951535312, 1.000000000000000000, 0.9510565162951535312, 1.000000000000000000, 0.9510565162951535312, 1.000000000000000000, 0.9510565162951535312, 1.000000000000000000, 0.9510565162951535312, 1.000000000000000000, 0.9510565162951535312, 1.000000000000000000, 0.9510565162951535312, 1.000000000000000000, 0.9510565162951535312, 1.000000000000000000, 0.9510565162951535312, 1.000000000000000000, 0.9510565162951535312, 1.000000000000000000, 0.9510565162951535312, 1.000000000000000000, 0.9510565162951535312, 1.000000000000000000, 0.9510565162951535312, 1.000000000000000000, 0.9510565162951535312, 1.000000000000000000, 0.9510565162951535312, 1.000000000000000000, 0.9510565162951535312, 1.000000000000000000, 0.9510565162951535312, 1.000000000000000000),
 ( 1.000000000000000000, 0.9510565162951535312, 1.000000000000000000, 0.9510565162951535312, 1.000000000000000000, 0.9510565162951535312, 1.000000000000000000, 0.9510565162951535312, 1.000000000000000000, 0.9510565162951535312, 1.000000000000000000, 0.9510565162951535312, 1.000000000000000000, 0.9510565162951535312, 1.000000000000000000, 0.9510565162951535312, 1.000000000000000000, 0.9510565162951535312, 1.000000000000000000, 0.9510565162951535312, 1.000000000000000000, 0.9510565162951535312, 1.000000000000000000, 0.9510565162951535312, 1.000000000000000000, 0.9510565162951535312, 1.000000000000000000, 0.9510565162951535312, 1.000000000000000000, 0.9510565162951535312, 1.000000000000000000, 0.9510565162951535312, 1.000000000000000000, 0.9510565162951535312, 1.000000000000000000, 0.9510565162951535312, 1.000000000000000000, 0.9510565162951535312, 1.000000000000000000, 0.9510565162951535312, 1.000000000000000000, 0.9510565162951535312, 1.000000000000000000, 0.9510565162951535312, 1.000000000000000000, 0.9510565162951535312, 1.000000000000000000, 0.9510565162951535312, 1.000000000000000000, 0.9510565162951535312, 1.000000000000000000, 0.9510565162951535312, 1.000000000000000000, 0.9510565162951535312, 1.000000000000000000, 0.9510565162951535312, 1.000000000000000000, 0.9510565162951535312, 1.000000000000000000, 0.9510565162951535312, 1.000000000000000000, 0.9510565162951535312, 1.000000000000000000, 0.9510565162951535312, 1.000000000000000000, 0.9510565162951535312, 1.000000000000000000, 0.9510565162951535312, 1.000000000000000000, 0.9510565162951535312, 1.000000000000000000, 0.9510565162951535312, 1.000000000000000000, 0.9510565162951535312, 1.000000000000000000, 0.9510565162951535312, 1.000000000000000000, 0.9510565162951535312, 1.000000000000000000, 0.9510565162951535312, 1.000000000000000000, 0.9510565162951535312, 1.000000000000000000, 0.9510565162951535312, 1.000000000000000000, 0.9510565162951535312, 1.000000000000000000, 0.9510565162951535312, 1.000000000000000000, 0.9510565162951535312, 1.000000000000000000, 0.9510565162951535312, 1.000000000000000000, 0.9510565162951535312, 1.000000000000000000, 0.9510565162951535312, 1.000000000000000000, 0.9510565162951535312, 1.000000000000000000, 0.9510565162951535312, 1.000000000000000000, 0.9510565162951535312, 1.000000000000000000, 0.9510565162951535312, 1.000000000000000000, 0.9510565162951535312, 1.000000000000000000, 0.9510565162951535312, 1.000000000000000000, 0.9510565162951535312, 1.000000000000000000, 0.9510565162951535312, 1.000000000000000000, 0.9510565162951535312, 1.000000000000000000, 0.9510565162951535312, 1.000000000000000000, 0.9510565162951535312, 1.000000000000000000, 0.9510565162951535312, 1.000000000000000000, 0.9510565162951535312, 1.000000000000000000, 0.9510565162951535312, 1.000000000000000000, 0.9510565162951535312, 1.000000000000000000, 0.9510565162951535312, 1.000000000000000000, 0.9510565162951535312, 1.000000000000000000, 0.9510565162951535312, 1.000000000000000000, 0.9510565162951535312, 1.000000000000000000, 0.9510565162951535312, 1.000000000000000000, 0.9510565162951535312, 1.000000000000000000, 0.9510565162951535312, 1.000000000000000000, 0.9510565162951535312, 1.000000000000000000, 0.9510565162951535312, 1.000000000000000000, 0.9510565162951535312, 1.000000000000000000, 0.9510565162951535312, 1.000000000000000000, 0.9510565162951535312, 1.000000000000000000, 0.9510565162951535312, 1.000000000000000000, 0.9510565162951535312, 1.000000000000000000, 0.9510565162951535312, 1.000000000000000000, 0.9510565162951535312, 1.000000000000000000, 0.9510565162951535312, 1.000000000000000000, 0.9510565162951535312, 1.000000000000000000, 0.9510565162951535312, 1.000000000000000000, 0.9510565162951535312, 1.000000000000000000, 0.9510565162951535312, 1.000000000000000000, 0.9510565162951535312, 1.000000000000000000, 0.9510565162951535312, 1.000000000000000000, 0.9510565162951535312, 1.000000000000000000, 0.9510565162951535312, 1.000000000000000000, 0.9510565162951535312, 1.000000000000000000, 0.9510565162951535312, 1.000000000000000000, 0.9510565162951535312, 1.000000000000000000, 0.9510565162951535312, 1.000000000000000000, 0.9510565162951535312, 1.000000000000000000, 0.9510565162951535312, 1.000000000000000000, 0.9510565162951535312, 1.000000000000000000, 0.9510565162951535312, 1.000000000000000000, 0.9510565162951535312, 1.000000000000000000, 0.9510565162951535312, 1.000000000000000000, 0.9510565162951535312, 1.000000000000000000, 0.9510565162951535312, 1.000000000000000000, 0.9510565162951535312, 1.000000000000000000, 0.9510565162951535312, 1.000000000000000000, 0.9510565162951535312, 1.000000000000000000, 0.9510565162951535312, 1.000000000000000000, 0.9510565162951535312, 1.000000000000000000, 0.9510565162951535312, 1.000000000000000000, 0.9510565162951535312, 1.000000000000000000, 0.9510565162951535312, 1.000000000000000000, 0.9510565162951535312, 1.000000000000000000, 0.9510565162951535312, 1.000000000000000000, 0.9510565162951535312, 1.000000000000000000, 0.9510565162951535312, 1.000000000000000000, 0.9510565162951535312, 1.000000000000000000, 0.9510565162951535312, 1.000000000000000000, 0.9510565162951535312, 1.000000000000000000, 0.9510565162951535312, 1.000000000000000000, 0.9510565162951535312, 1.000000000000000000, 0.9510565162951535312, 1.000000000000000000, 0.9510565162951535312, 1.000000000000000000, 0.9510565162951535312, 1.000000000000000000, 0.9510565162951535312, 1.000000000000000000, 0.9510565162951535312, 1.000000000000000000, 0.9510565162951535312, 1.000000000000000000, 0.9510565162951535312, 1.000000000000000000, 0.9510565162951535312, 1.000000000000000000, 0.9510565162951535312, 1.000000000000000000, 0.9510565162951535312, 1.000000000000000000, 0.9510565162951535312, 1.000000000000000000, 0.9510565162951535312, 1.000000000000000000, 0.9510565162951535312, 1.000000000000000000, 0.9510565162951535312, 1.000000000000000000, 0.9510565162951535312, 1.000000000000000000, 0.9510565162951535312, 1.000000000000000000, 0.9510565162951535312, 1.000000000000000000, 0.9510565162951535312, 1.000000000000000000, 0.9510565162951535312, 1.000000000000000000, 0.9510565162951535312, 1.000000000000000000, 0.9510565162951535312, 1.000000000000000000, 0.9510565162951535312, 1.000000000000000000, 0.9510565162951535312, 1.000000000000000000, 0.9510565162951535312, 1.000000000000000000, 0.9510565162951535312, 1.000000000000000000, 0.9510565162951535312, 1.000000000000000000, 0.9510565162951535312, 1.000000000000000000, 0.9510565162951535312, 1.000000000000000000, 0.9510565162951535312, 1.000000000000000000, 0.9510565162951535312, 1.000000000000000000, 0.9510565162951535312, 1.000000000000000000, 0.9510565162951535312, 1.000000000000000000, 0.9510565162951535312, 1.000000000000000000, 0.9510565162951535312, 1.000000000000000000, 0.9510565162951535312, 1.000000000000000000, 0.9510565162951535312, 1.000000000000000000, 0.9510565162951535312, 1.000000000000000000, 0.9510565162951535312, 1.000000000000000000, 0.9510565162951535312, 1.000000000000000000, 0.9510565162951535312, 1.000000000000000000, 0.9510565162951535312, 1.000000000000000000, 0.9510565162951535312, 1.000000000000000000, 0.9510565162951535312, 1.000000000000000000, 0.9510565162951535312, 1.000000000000000000, 0.9510565162951535312, 1.000000000000000000, 0.9510565162951535312, 1.000000000000000000, 0.9510565162951535312, 1.000000000000000000, 0.9510565162951535312, 1.000000000000000000, 0.9510565162951535312, 1.000000000000000000, 0.9510565162951535312, 1.000000000000000000, 0.9510565162951535312, 1.000000000000000000, 0.9510565162951535312, 1.000000000000000000, 0.9510565162951535312, 1.000000000000000000, 0.9510565162951535312, 1.000000000000000000, 0.9510565162951535312, 1.000000000000000000, 0.9510565162951535312, 1.000000000000000000, 0.9510565162951535312, 1.000000000000000000, 0.9510565162951535312, 1.000000000000000000, 0.9510565162951535312, 1.000000000000000000, 0.9510565162951535312, 1.000000000000000000, 0.9510565162951535312, 1.000000000000000000, 0.9510565162951535312, 1.000000000000000000, 0.9510565162951535312, 1.000000000000000000, 0.9510565162951535312, 1.000000000000000000, 0.9510565162951535312, 1.000000000000000000, 0.9510565162951535312, 1.000000000000000000, 0.9510565162951535312, 1.000000000000000000, 0.9510565162951535312, 1.000000000000000000, 0.9510565162951535312, 1.000000000000000000, 0.9510565162951535312, 1.000000000000000000, 0.9510565162951535312, 1.000000000000000000, 0.9510565162951535312, 1.000000000000000000, 0.9510565162951535312, 1.000000000000000000, 0.9510565162951535312, 1.000000000000000000, 0.9510565162951535312, 1.000000000000000000, 0.9510565162951535312, 1.000000000000000000, 0.9510565162951535312, 1.000000000000000000, 0.9510565162951535312, 1.000000000000000000, 0.9510565162951535312, 1.000000000000000000, 0.9510565162951535312, 1.000000000000000000, 0.9510565162951535312, 1.000000000000000000, 0.9510565162951535312, 1.000000000000000000, 0.9510565162951535312, 1.000000000000000000, 0.9510565162951535312, 1.000000000000000000, 0.9510565162951535312, 1.000000000000000000, 0.9510565162951535312, 1.000000000000000000, 0.9510565162951535312, 1.000000000000000000, 0.9510565162951535312, 1.000000000000000000, 0.9510565162951535312, 1.000000000000000000, 0.9510565162951535312, 1.000000000000000000, 0.9510565162951535312, 1.000000000000000000, 0.9510565162951535312, 1.000000000000000000, 0.9510565162951535312, 1.000000000000000000, 0.9510565162951535312, 1.000000000000000000, 0.9510565162951535312, 1.000000000000000000, 0.9510565162951535312, 1.000000000000000000, 0.9510565162951535312, 1.000000000000000000, 0.9510565162951535312, 1.000000000000000000, 0.9510565162951535312, 1.000000000000000000, 0.9510565162951535312, 1.000000000000000000, 0.9510565162951535312, 1.000000000000000000, 0.9510565162951535312, 1.000000000000000000, 0.9510565162951535312, 1.000000000000000000, 0.9510565162951535312, 1.000000000000000000, 0.9510565162951535312, 1.000000000000000000, 0.9510565162951535312, 1.000000000000000000, 0.9510565162951535312, 1.000000000000000000, 0.9510565162951535312, 1.000000000000000000, 0.9510565162951535312, 1.000000000000000000, 0.9510565162951535312, 1.000000000000000000, 0.9510565162951535312, 1.000000000000000000, 0.9510565162951535312, 1.000000000000000000, 0.9510565162951535312, 1.000000000000000000, 0.9510565162951535312, 1.000000000000000000, 0.9510565162951535312, 1.000000000000000000, 0.9510565162951535312, 1.000000000000000000, 0.9510565162951535312, 1.000000000000000000, 0.9510565162951535312, 1.000000000000000000, 0.9510565162951535312, 1.000000000000000000, 0.9510565162951535312, 1.000000000000000000, 0.9510565162951535312, 1.000000000000000000, 0.9510565162951535312, 1.000000000000000000, 0.9510565162951535312, 1.000000000000000000, 0.9510565162951535312, 1.000000000000000000, 0.9510565162951535312, 1.000000000000000000, 0.9510565162951535312, 1.000000000000000000, 0.9510565162951535312, 1.000000000000000000, 0.9510565162951535312, 1.000000000000000000, 0.9510565162951535312, 1.000000000000000000, 0.9510565162951535312, 1.000000000000000000, 0.9510565162951535312, 1.000000000000000000, 0.9510565162951535312, 1.000000000000000000, 0.9510565162951535312, 1.000000000000000000, 0.9510565162951535312, 1.000000000000000000, 0.9510565162951535312, 1.000000000000000000, 0.9510565162951535312, 1.000000000000000000, 0.9510565162951535312, 1.000000000000000000, 0.9510565162951535312, 1.000000000000000000, 0.9510565162951535312, 1.000000000000000000, 0.9510565162951535312, 1.000000000000000000, 0.9510565162951535312, 1.000000000000000000, 0.9510565162951535312, 1.000000000000000000, 0.9510565162951535312, 1.000000000000000000, 0.9510565162951535312, 1.000000000000000000, 0.9510565162951535312, 1.000000000000000000, 0.9510565162951535312, 1.000000000000000000, 0.9510565162951535312, 1.000000000000000000, 0.9510565162951535312, 1.000000000000000000, 0.9510565162951535312, 1.000000000000000000, 0.9510565162951535312, 1.000000000000000000, 0.9510565162951535312, 1.000000000000000000, 0.9510565162951535312, 1.000000000000000000, 0.9510565162951535312, 1.000000000000000000, 0.9510565162951535312, 1.000000000000000000, 0.9510565162951535312, 1.000000000000000000, 0.9510565162951535312, 1.000000000000000000, 0.9510565162951535312, 1.000000000000000000, 0.9510565162951535312, 1.000000000000000000, 0.9510565162951535312, 1.000000000000000000, 0.9510565162951535312, 1.000000000000000000, 0.9510565162951535312, 1.000000000000000000, 0.9510565162951535312, 1.000000000000000000, 0.9510565162951535312, 1.000000000000000000, 0.9510565162951535312, 1.000000000000000000, 0.9510565162951535312, 1.000000000000000000, 0.9510565162951535312, 1.000000000000000000, 0.9510565162951535312, 1.000000000000000000, 0.9510565162951535312, 1.000000000000000000, 0.9510565162951535312, 1.000000000000000000, 0.9510565162951535312, 1.000000000000000000, 0.9510565162951535312, 1.000000000000000000, 0.9510565162951535312, 1.000000000000000000, 0.9510565162951535312, 1.000000000000000000, 0.9510565162951535312, 1.000000000000000000, 0.9510565162951535312, 1.000000000000000000, 0.9510565162951535312, 1.000000000000000000, 0.9510565162951535312, 1.000000000000000000, 0.9510565162951535312, 1.000000000000000000, 0.9510565162951535312, 1.000000000000000000, 0.9510565162951535312, 1.000000000000000000, 0.9510565162951535312, 1.000000000000000000, 0.9510565162951535312, 1.000000000000000000, 0.9510565162951535312, 1.000000000000000000, 0.9510565162951535312, 1.000000000000000000, 0.9510565162951535312, 1.000000000000000000, 0.9510565162951535312, 1.000000000000000000, 0.9510565162951535312, 1.000000000000000000, 0.9510565162951535312, 1.000000000000000000, 0.9510565162951535312, 1.000000000000000000, 0.9510565162951535312, 1.000000000000000000, 0.9510565162951535312, 1.000000000000000000, 0.9510565162951535312, 1.000000000000000000, 0.9510565162951535312, 1.000000000000000000, 0.9510565162951535312, 1.000000000000000000, 0.9510565162951535312, 1.000000000000000000, 0.9510565162951535312, 1.000000000000000000, 0.9510565162951535312, 1.000000000000000000, 0.9510565162951535312, 1.000000000000000000, 0.9510565162951535312, 1.000000000000000000, 0.9510565162951535312, 1.000000000000000000, 0.9510565162951535312, 1.000000000000000000, 0.9510565162951535312, 1.000000000000000000, 0.9510565162951535312, 1.000000000000000000, 0.9510565162951535312, 1.000000000000000000, 0.9510565162951535312, 1.000000000000000000, 0.9510565162951535312, 1.000000000000000000, 0.9510565162951535312, 1.000000000000000000, 0.9510565162951535312, 1.000000000000000000, 0.9510565162951535312, 1.000000000000000000, 0.9510565162951535312, 1.000000000000000000, 0.9510565162951535312, 1.000000000000000000, 0.9510565162951535312, 1.000000000000000000, 0.9510565162951535312, 1.000000000000000000, 0.9510565162951535312, 1.000000000000000000, 0.9510565162951535312, 1.000000000000000000, 0.9510565162951535312, 1.000000000000000000, 0.9510565162951535312, 1.000000000000000000, 0.9510565162951535312, 1.000000000000000000, 0.9510565162951535312, 1.000000000000000000, 0.9510565162951535312, 1.000000000000000000, 0.9510565162951535312, 1.000000000000000000, 0.9510565162951535312, 1.000000000000000000, 0.9510565162951535312, 1.000000000000000000, 0.9510565162951535312, 1.000000000000000000, 0.9510565162951535312, 1.000000000000000000, 0.9510565162951535312, 1.000000000000000000, 0.9510565162951535312, 1.000000000000000000, 0.9510565162951535312, 1.000000000000000000, 0.9510565162951535312, 1.000000000000000000, 0.9510565162951535312, 1.000000000000000000, 0.9510565162951535312, 1.000000000000000000, 0.9510565162951535312, 1.000000000000000000, 0.9510565162951535312, 1.000000000000000000, 0.9510565162951535312, 1.000000000000000000, 0.9510565162951535312, 1.000000000000000000, 0.9510565162951535312, 1.000000000000000000, 0.9510565162951535312, 1.000000000000000000, 0.9510565162951535312, 1.000000000000000000, 0.9510565162951535312, 1.000000000000000000, 0.9510565162951535312, 1.000000000000000000, 0.9510565162951535312, 1.000000000000000000, 0.9510565162951535312, 1.000000000000000000, 0.9510565162951535312, 1.000000000000000000, 0.9510565162951535312, 1.000000000000000000, 0.9510565162951535312, 1.000000000000000000, 0.9510565162951535312, 1.000000000000000000, 0.9510565162951535312, 1.000000000000000000, 0.9510565162951535312, 1.000000000000000000, 0.9510565162951535312, 1.000000000000000000, 0.9510565162951535312, 1.000000000000000000, 0.9510565162951535312, 1.000000000000000000, 0.9510565162951535312, 1.000000000000000000, 0.9510565162951535312, 1.000000000000000000, 0.9510565162951535312, 1.000000000000000000, 0.9510565162951535312, 1.000000000000000000, 0.9510565162951535312, 1.000000000000000000, 0.9510565162951535312, 1.000000000000000000, 0.9510565162951535312, 1.000000000000000000, 0.9510565162951535312, 1.000000000000000000, 0.9510565162951535312, 1.000000000000000000, 0.9510565162951535312, 1.000000000000000000, 0.9510565162951535312, 1.000000000000000000, 0.9510565162951535312, 1.000000000000000000, 0.9510565162951535312, 1.000000000000000000, 0.9510565162951535312, 1.000000000000000000, 0.9510565162951535312, 1.000000000000000000, 0.9510565162951535312, 1.000000000000000000, 0.9510565162951535312, 1.000000000000000000, 0.9510565162951535312, 1.000000000000000000, 0.9510565162951535312, 1.000000000000000000, 0.9510565162951535312, 1.000000000000000000, 0.9510565162951535312, 1.000000000000000000, 0.9510565162951535312, 1.000000000000000000) ) ) 
 REPRESENTATION_ITEM ( '' )  SURFACE ( )  );
#9915 = CARTESIAN_POINT ( 'NONE',  ( 26.29305231718578995, 9.199999999999985079, -19.10302069950538240 ) ) ;
#9916 = CARTESIAN_POINT ( 'NONE',  ( -10.04305231718578462, 52.40000000000000568, 30.90933677959249337 ) ) ;
#9917 = CARTESIAN_POINT ( 'NONE',  ( 26.09010956794244507, 53.24440999907603356, 6.950374756619249084 ) ) ;
#9918 = CARTESIAN_POINT ( 'NONE',  ( 20.75514604977248467, 48.42500000273119554, -28.56700777964554305 ) ) ;
#9919 = CARTESIAN_POINT ( 'NONE',  ( 10.37757302488624767, 63.97500000273119269, 31.93888565452638417 ) ) ;
#9920 = CARTESIAN_POINT ( 'NONE',  ( -10.37757302488623701, 39.77500000273118275, 31.93888565452638417 ) ) ;
#9921 = CARTESIAN_POINT ( 'NONE',  ( -23.41746824999999887, 15.62499999726882294, -2.867812753649727150E-15 ) ) ;
#9922 = CARTESIAN_POINT ( 'NONE',  ( 2.584737979205442066E-13, 14.14843749999999467, 27.95245687107223276 ) ) ;
#9923 = CARTESIAN_POINT ( 'NONE',  ( 3.980102097228898626E-15, 80.00000000000001421, 32.50000000000000000 ) ) ;
#9924 = CARTESIAN_POINT ( 'NONE',  ( -24.38179134483146981, 16.99999999999998934, -1.972686091485069459 ) ) ;
#9925 = CARTESIAN_POINT ( 'NONE',  ( 26.29305231718578995, 77.20000000000000284, -19.10302069950538240 ) ) ;
#9926 = CARTESIAN_POINT ( 'NONE',  ( -10.37757302488624411, 22.72500000273118559, -31.93888565452638417 ) ) ;
#9927 = CARTESIAN_POINT ( 'NONE',  ( 0.000000000000000000, 0.000000000000000000, 0.000000000000000000 ) ) ;
#9928 = DIRECTION ( 'NONE',  ( 0.000000000000000000, -1.000000000000000000, 0.000000000000000000 ) ) ;
#9929 = CARTESIAN_POINT ( 'NONE',  ( 0.000000000000000000, 52.00000000000000711, 32.50000000000000000 ) ) ;
#9930 = CARTESIAN_POINT ( 'NONE',  ( 28.00173670424535644, 66.70795166574268364, -7.543491769121920321 ) ) ;
#9931 = CARTESIAN_POINT ( 'NONE',  ( -32.50000000000000000, 38.60000000546239818, 10.55989012756946366 ) ) ;
#9932 = CARTESIAN_POINT ( 'NONE',  ( 2.375766604868046361, 70.80125428700921475, 14.99999999999999822 ) ) ;
#9933 = CARTESIAN_POINT ( 'NONE',  ( -10.37757302488624411, 24.72500000273119980, -31.93888565452638417 ) ) ;
#9934 = VECTOR ( 'NONE', #23299, 1000.000000000000114 ) ;
#9935 = CIRCLE ( 'NONE', #615, 15.00000000000000000 ) ;
#9936 = CARTESIAN_POINT ( 'NONE',  ( -13.97622843553588901, 31.62239583333332860, 24.20753774853756823 ) ) ;
#9937 = ORIENTED_EDGE ( 'NONE', *, *, #32022, .F. ) ;
#9938 = CARTESIAN_POINT ( 'NONE',  ( 27.16883889988624290, 71.92500000273120975, 19.73931689729373673 ) ) ;
#9939 = CARTESIAN_POINT ( 'NONE',  ( 28.01184896238290278, 40.64583333333332860, -7.505752307973347470 ) ) ;
#9940 = CARTESIAN_POINT ( 'NONE',  ( 0.000000000000000000, 16.99999999999998579, 0.000000000000000000 ) ) ;
#9941 = ORIENTED_EDGE ( 'NONE', *, *, #31376, .F. ) ;
#9942 = CARTESIAN_POINT ( 'NONE',  ( 7.543491769121427382, 62.13579833425730925, -28.00173670424548433 ) ) ;
#9943 = CARTESIAN_POINT ( 'NONE',  ( 13.94119854578937812, 56.54986083425731636, 24.22776226481240514 ) ) ;
#9944 = EDGE_LOOP ( 'NONE', ( #26661, #20370, #11655, #31715 ) ) ;
#9945 = CARTESIAN_POINT ( 'NONE',  ( 27.16883889988624290, 9.925000002731207971, 19.73931689729373673 ) ) ;
#9946 = CARTESIAN_POINT ( 'NONE',  ( -26.02091320914878025, 20.73138916574268720, -14.97647472619899389 ) ) ;
#9947 = CARTESIAN_POINT ( 'NONE',  ( -5.147494310547430452, 46.05125428700922896, -32.49999999999999289 ) ) ;
#9948 = CARTESIAN_POINT ( 'NONE',  ( -10.37757302488623701, 31.77500000273120051, 31.93888565452638417 ) ) ;
#9949 = CARTESIAN_POINT ( 'NONE',  ( -32.50000000000000000, 46.40000000546238113, -10.55989012756945478 ) ) ;
#9950 = EDGE_CURVE ( 'NONE', #33526, #16018, #8865, .T. ) ;
#9951 = CARTESIAN_POINT ( 'NONE',  ( 9.270509831248423538, 77.30000000000001137, -12.75976212528059861 ) ) ;
#9952 = CARTESIAN_POINT ( 'NONE',  ( 33.58253175000000113, 24.22500000273119625, -10.91162601494193751 ) ) ;
#9953 = CARTESIAN_POINT ( 'NONE',  ( 20.08610463437157279, 31.80000000546236905, -27.64615127144129758 ) ) ;
#9954 = CARTESIAN_POINT ( 'NONE',  ( 10.37757302488624767, 47.97500000273119269, 31.93888565452638417 ) ) ;
#9955 = CARTESIAN_POINT ( 'NONE',  ( 26.29305231718579350, 28.80000000000000782, 19.10302069950537529 ) ) ;
#9956 = CARTESIAN_POINT ( 'NONE',  ( -2.092463501923844636E-15, 27.50000000000000355, -34.17252228774368916 ) ) ;
#9957 = CARTESIAN_POINT ( 'NONE',  ( 7.236395654485760609, 17.02499999726880731, -22.27133577429736633 ) ) ;
#9958 = CARTESIAN_POINT ( 'NONE',  ( 33.58253175000000823, 74.02500000273120406, 10.91162601494192863 ) ) ;
#9959 = CARTESIAN_POINT ( 'NONE',  ( 10.04305231718579705, 62.60000000000000142, 30.90933677959248982 ) ) ;
#9960 = AXIS2_PLACEMENT_3D ( 'NONE', #12482, #5271, #17988 ) ;
#9961 = CARTESIAN_POINT ( 'NONE',  ( 5.348221797398307942, 74.00000000000001421, 12.84883053416113974 ) ) ;
#9962 = CARTESIAN_POINT ( 'NONE',  ( 10.37757302488624056, 58.77500000273119696, -31.93888565452638417 ) ) ;
#9963 = CARTESIAN_POINT ( 'NONE',  ( -15.00000000000000000, 74.15000000546240244, -4.873795443493594171 ) ) ;
#9964 = CARTESIAN_POINT ( 'NONE',  ( 0.000000000000000000, 16.99999999999998579, 0.000000000000000000 ) ) ;
#9965 = CARTESIAN_POINT ( 'NONE',  ( -33.58253175000000113, 21.22500000273117848, 10.91162601494193929 ) ) ;
#9966 = CARTESIAN_POINT ( 'NONE',  ( 7.570916362186207671, 9.349999994537617098, 23.30088464923126779 ) ) ;
#9967 = CARTESIAN_POINT ( 'NONE',  ( 14.01125832528286352, 24.46652750092397355, -24.18731323226246843 ) ) ;
#9968 = CARTESIAN_POINT ( 'NONE',  ( -32.50000000000000000, 25.99999999999999645, 0.000000000000000000 ) ) ;
#9969 = CARTESIAN_POINT ( 'NONE',  ( 10.37757302488624767, 43.72500000273120691, 31.93888565452638417 ) ) ;
#9970 = DIRECTION ( 'NONE',  ( -0.000000000000000000, -1.000000000000000000, -0.000000000000000000 ) ) ;
#9971 = CARTESIAN_POINT ( 'NONE',  ( -10.37757302488624411, 56.97500000273118559, -31.93888565452638417 ) ) ;
#9972 = CARTESIAN_POINT ( 'NONE',  ( 30.02300923189239867, 45.66444416759065916, 0.04044903254992252006 ) ) ;
#9973 = CARTESIAN_POINT ( 'NONE',  ( 15.14183272437242067, 5.699999999999993960, 20.84094480462498211 ) ) ;
#9974 = CARTESIAN_POINT ( 'NONE',  ( 20.47846945139867003, 35.48399333240935505, -20.53372385742107653 ) ) ;
#9975 = CARTESIAN_POINT ( 'NONE',  ( -10.04305231718578462, 60.90000000546237402, 30.90933677959249337 ) ) ;
#9976 = CARTESIAN_POINT ( 'NONE',  ( -11.25946833292375793, 74.67500000273119554, -8.180482586598733619 ) ) ;
#9977 = CARTESIAN_POINT ( 'NONE',  ( -1.778240108872766143E-15, 58.00000000546237544, -32.49999999999999289 ) ) ;
#9978 = CARTESIAN_POINT ( 'NONE',  ( 24.18731323226221974, 66.56472249907604066, -14.01125832528328985 ) ) ;
#9979 =( BOUNDED_CURVE ( )  B_SPLINE_CURVE ( 2, ( #1539, #23174, #33636, #4805, #30365, #18039, #33109, #4292, #12360, #33460, #9959, #9612, #1706 ),
 .UNSPECIFIED., .F., .T. ) 
 B_SPLINE_CURVE_WITH_KNOTS ( ( 3, 2, 2, 2, 2, 2, 3 ),
 ( 0.2115384615384615363, 0.2128205128205128138, 0.2153846153846153966, 0.2179487179487179516, 0.2205128205128205066, 0.2230769230769230893, 0.2243589743589743668 ),
 .UNSPECIFIED. ) 
 CURVE ( )  GEOMETRIC_REPRESENTATION_ITEM ( )  RATIONAL_B_SPLINE_CURVE ( ( 0.9755282581475768211, 0.9755282581475768211, 1.000000000000000000, 0.9510565162951535312, 1.000000000000000000, 0.9510565162951535312, 1.000000000000000000, 0.9510565162951535312, 1.000000000000000000, 0.9510565162951535312, 1.000000000000000000, 0.9755282581475768211, 0.9755282581475768211 ) ) 
 REPRESENTATION_ITEM ( '' )  );
#9980 = CARTESIAN_POINT ( 'NONE',  ( 32.50000000000000711, 63.40000000546236691, 10.55989012756945122 ) ) ;
#9981 = EDGE_CURVE ( 'NONE', #8583, #27363, #26420, .T. ) ;
#9982 = CARTESIAN_POINT ( 'NONE',  ( 26.29305231718578995, 77.70000000546239960, -19.10302069950538240 ) ) ;
#9983 = CARTESIAN_POINT ( 'NONE',  ( -2.584737979205441561E-13, 12.42968749999999289, -30.02300923189239512 ) ) ;
#9984 = CARTESIAN_POINT ( 'NONE',  ( 27.16883889988623935, 36.57500000273118701, -19.73931689729374384 ) ) ;
#9985 =( BOUNDED_CURVE ( )  B_SPLINE_CURVE ( 2, ( #17690, #23175, #2059, #28653, #12361, #20094, #28150, #30539, #12535, #25915, #7035, #9787, #12876 ),
 .UNSPECIFIED., .F., .T. ) 
 B_SPLINE_CURVE_WITH_KNOTS ( ( 3, 2, 2, 2, 2, 2, 3 ),
 ( 0.7371794871794872250, 0.7384615384615385025, 0.7410256410256410575, 0.7435897435897436125, 0.7461538461538461675, 0.7487179487179487225, 0.7500000000000000000 ),
 .UNSPECIFIED. ) 
 CURVE ( )  GEOMETRIC_REPRESENTATION_ITEM ( )  RATIONAL_B_SPLINE_CURVE ( ( 0.9755282581475768211, 0.9755282581475768211, 1.000000000000000000, 0.9510565162951535312, 1.000000000000000000, 0.9510565162951535312, 1.000000000000000000, 0.9510565162951535312, 1.000000000000000000, 0.9510565162951535312, 1.000000000000000000, 0.9755282581475768211, 0.9755282581475768211 ) ) 
 REPRESENTATION_ITEM ( '' )  );
#9986 = CARTESIAN_POINT ( 'NONE',  ( -18.94512977948576093, 6.324999997268820451, 13.76444248337722698 ) ) ;
#9987 = ORIENTED_EDGE ( 'NONE', *, *, #8784, .T. ) ;
#9988 = CARTESIAN_POINT ( 'NONE',  ( 6.486482029760649416E-15, 73.87500000273119838, 35.31076352940723240 ) ) ;
#9989 = CARTESIAN_POINT ( 'NONE',  ( 10.04305231718578817, 21.90000000546237047, -30.90933677959249337 ) ) ;
#9990 = EDGE_CURVE ( 'NONE', #1219, #684, #4504, .T. ) ;
#9991 = CARTESIAN_POINT ( 'NONE',  ( 28.01184896238290278, 44.08333333333332860, -7.505752307973347470 ) ) ;
#9992 = CARTESIAN_POINT ( 'NONE',  ( 10.04305231718579705, 61.10000000546239818, 30.90933677959248982 ) ) ;
#9993 = ORIENTED_EDGE ( 'NONE', *, *, #19722, .T. ) ;
#9994 = CARTESIAN_POINT ( 'NONE',  ( 19.82091636218621389, 5.949999994537630066, -14.40073868116559197 ) ) ;
#9995 = CARTESIAN_POINT ( 'NONE',  ( -33.58253175000000113, 39.12500000273119838, 0.000000000000000000 ) ) ;
#9996 = CARTESIAN_POINT ( 'NONE',  ( 7.236395654485760609, 15.02499999726880731, -22.27133577429736633 ) ) ;
#9997 = CARTESIAN_POINT ( 'NONE',  ( -27.16883889988623935, 71.57500000273120122, 19.73931689729374739 ) ) ;
#9998 = CARTESIAN_POINT ( 'NONE',  ( -10.04305231718579172, 4.100000005462373309, -30.90933677959248982 ) ) ;
#9999 = EDGE_CURVE ( 'NONE', #23029, #5175, #2762, .T. ) ;
#10000 = CARTESIAN_POINT ( 'NONE',  ( -27.16883889988624290, 58.92500000273119554, -19.73931689729374028 ) ) ;
#10001 = CARTESIAN_POINT ( 'NONE',  ( -26.00068869287340334, 14.72135416666666607, 15.01150461594643559 ) ) ;
#10002 = CARTESIAN_POINT ( 'NONE',  ( 10.04305231718579705, 48.60000000000000142, 30.90933677959248982 ) ) ;
#10003 = CARTESIAN_POINT ( 'NONE',  ( -26.29305231718579350, 13.79999999999997939, -19.10302069950537884 ) ) ;
#10004 = CARTESIAN_POINT ( 'NONE',  ( 27.16883889988623935, 18.57500000273118346, -19.73931689729374384 ) ) ;
#10005 = AXIS2_PLACEMENT_3D ( 'NONE', #22133, #33081, #12672 ) ;
#10006 = CARTESIAN_POINT ( 'NONE',  ( 3.445340210940985210E-14, 7.499999999999994671, 24.50000000000000000 ) ) ;
#10007 = CARTESIAN_POINT ( 'NONE',  ( -24.22776226481266448, 27.60638916574269075, -13.94119854578892514 ) ) ;
#10008 = CARTESIAN_POINT ( 'NONE',  ( -11.25946833292375793, 81.17500000273119554, -8.180482586598733619 ) ) ;
#10009 = CARTESIAN_POINT ( 'NONE',  ( -1.778240108872766143E-15, 42.00000000546236834, -32.49999999999999289 ) ) ;
#10010 = CARTESIAN_POINT ( 'NONE',  ( -1.778240108872766143E-15, 43.50000000000000000, -32.49999999999999289 ) ) ;
#10011 = CIRCLE ( 'NONE', #2333, 15.00000000000000000 ) ;
#10012 = CARTESIAN_POINT ( 'NONE',  ( 33.58253175000000113, 76.47500000273117848, -10.91162601494193751 ) ) ;
#10013 = ORIENTED_EDGE ( 'NONE', *, *, #13215, .T. ) ;
#10014 = CARTESIAN_POINT ( 'NONE',  ( -4.523095164977116484E-15, 10.62499999726880695, 24.62258325217400312 ) ) ;
#10015 = CARTESIAN_POINT ( 'NONE',  ( -7.236395654485763274, 2.024999997268822405, 22.27133577429736633 ) ) ;
#10016 = CARTESIAN_POINT ( 'NONE',  ( -13.97622843553632421, 53.39322916666665009, -24.20753774853731599 ) ) ;
#10017 = CARTESIAN_POINT ( 'NONE',  ( -20.75514604977248823, 60.82500000273121543, -28.56700777964554305 ) ) ;
#10018 = CARTESIAN_POINT ( 'NONE',  ( 10.37757302488624056, 20.77500000273117919, -31.93888565452638417 ) ) ;
#10019 = CARTESIAN_POINT ( 'NONE',  ( 33.58253175000000823, 12.27500000273118452, 10.91162601494192863 ) ) ;
#10020 = CARTESIAN_POINT ( 'NONE',  ( 13.97622843553633842, 27.61197916666666430, 24.20753774853730889 ) ) ;
#10021 = CARTESIAN_POINT ( 'NONE',  ( 25.98046417659858420, 18.45090250092397355, 15.04653450569292872 ) ) ;
#10022 = CARTESIAN_POINT ( 'NONE',  ( -20.53372385742107653, 13.99961833240935327, -20.47846945139867003 ) ) ;
#10023 = CARTESIAN_POINT ( 'NONE',  ( 33.58253175000000113, 2.225000002731181592, -10.91162601494193751 ) ) ;
#10024 = CARTESIAN_POINT ( 'NONE',  ( -4.300734207923755825, 73.77500000273118985, 13.23629886949340673 ) ) ;
#10025 = CARTESIAN_POINT ( 'NONE',  ( -32.50000000000000000, 42.09999999999997300, 10.55989012756946366 ) ) ;
#10026 = CARTESIAN_POINT ( 'NONE',  ( -20.75514604977248112, 47.42500000273119554, 28.56700777964554661 ) ) ;
#10027 = CARTESIAN_POINT ( 'NONE',  ( 14.47279130897151767, 6.924999997268805885, -19.92008829642072598 ) ) ;
#10028 = PLANE ( 'NONE',  #10641 ) ;
#10029 = ORIENTED_EDGE ( 'NONE', *, *, #21089, .F. ) ;
#10030 = CARTESIAN_POINT ( 'NONE',  ( -27.16883889988623935, 53.57500000273117280, 19.73931689729374739 ) ) ;
#10031 = DIRECTION ( 'NONE',  ( -0.000000000000000000, 1.000000000000000000, -0.000000000000000000 ) ) ;
#10032 = AXIS2_PLACEMENT_3D ( 'NONE', #28619, #7173, #28453 ) ;
#10033 = CARTESIAN_POINT ( 'NONE',  ( 26.09010956794232428, 45.52121500092397355, -6.950374756619718042 ) ) ;
#10034 = CARTESIAN_POINT ( 'NONE',  ( -33.58253175000000113, 73.47500000273117848, 10.91162601494193929 ) ) ;
#10035 = ORIENTED_EDGE ( 'NONE', *, *, #32348, .T. ) ;
#10036 = CARTESIAN_POINT ( 'NONE',  ( 20.75514604977248467, 24.42500000273119554, -28.56700777964554305 ) ) ;
#10037 = AXIS2_PLACEMENT_3D ( 'NONE', #26116, #18239, #20294 ) ;
#10038 = CARTESIAN_POINT ( 'NONE',  ( -15.01150461594642138, 15.58072916666666607, -26.00068869287340334 ) ) ;
#10039 = VERTEX_POINT ( 'NONE', #20660 ) ;
#10040 = CARTESIAN_POINT ( 'NONE',  ( -33.58253175000000113, 65.12500000273119838, 0.000000000000000000 ) ) ;
#10041 = CARTESIAN_POINT ( 'NONE',  ( -28.01184896238304134, 35.77604166666666430, -7.505752307972844761 ) ) ;
#10042 = CARTESIAN_POINT ( 'NONE',  ( 15.14183272437241889, 11.70000000000000995, 20.84094480462498211 ) ) ;
#10043 = CARTESIAN_POINT ( 'NONE',  ( 23.41746824999999887, 1.224999997268811480, -7.608796670333727974 ) ) ;
#10044 = CARTESIAN_POINT ( 'NONE',  ( 27.16883889988624290, 9.925000002731193760, 19.73931689729373673 ) ) ;
#10045 = CARTESIAN_POINT ( 'NONE',  ( -20.47846945139866648, 50.95274333240935505, 20.53372385742108008 ) ) ;
#10046 = CARTESIAN_POINT ( 'NONE',  ( -15.00000000000000000, 75.90000000000000568, -4.873795443493594171 ) ) ;
#10047 = CARTESIAN_POINT ( 'NONE',  ( 5.147494310547426899, 19.94874572391552547, -32.50000000000000000 ) ) ;
#10048 = CARTESIAN_POINT ( 'NONE',  ( -2.375766604868041476, 74.69874572391552192, 14.99999999999999822 ) ) ;
#10049 = CARTESIAN_POINT ( 'NONE',  ( -24.50000000000000000, 14.74999999453763166, -3.000384657911015469E-15 ) ) ;
#10050 = CARTESIAN_POINT ( 'NONE',  ( 2.897257156509938333E-15, 72.75000000546236834, 15.77193336357400710 ) ) ;
#10051 = CARTESIAN_POINT ( 'NONE',  ( -6.988114217767819270, 21.16666666666666430, 26.07999730980490583 ) ) ;
#10052 = CARTESIAN_POINT ( 'NONE',  ( 33.58253175000000823, 34.02500000273118275, 10.91162601494192863 ) ) ;
#10053 = CARTESIAN_POINT ( 'NONE',  ( -20.75514604977248112, 77.42500000273119554, 28.56700777964554661 ) ) ;
#10054 = CARTESIAN_POINT ( 'NONE',  ( -10.37757302488623701, 43.77500000273119696, 31.93888565452638417 ) ) ;
#10055 = CARTESIAN_POINT ( 'NONE',  ( 33.58253175000000113, 24.47500000273118914, -10.91162601494193574 ) ) ;
#10056 = CARTESIAN_POINT ( 'NONE',  ( -32.50000000000000000, 12.40000000546237402, -10.55989012756945300 ) ) ;
#10057 = AXIS2_PLACEMENT_3D ( 'NONE', #2445, #30925, #25781 ) ;
#10058 = CARTESIAN_POINT ( 'NONE',  ( 33.58253175000000113, 78.12500000273119838, -4.112674001490185761E-15 ) ) ;
#10059 = CARTESIAN_POINT ( 'NONE',  ( 10.04305231718578817, 59.90000000546235981, -30.90933677959249337 ) ) ;
#10060 = CARTESIAN_POINT ( 'NONE',  ( 20.08610463437158344, 58.70000000000000995, 27.64615127144129403 ) ) ;
#10061 = CARTESIAN_POINT ( 'NONE',  ( -23.41746825000000243, 17.72499999726881370, 7.608796670333725309 ) ) ;
#10062 = CARTESIAN_POINT ( 'NONE',  ( 33.58253175000000113, 64.22500000273117848, -10.91162601494193574 ) ) ;
#10063 = CARTESIAN_POINT ( 'NONE',  ( 7.236395654485755280, 8.724999997268806595, 22.27133577429736988 ) ) ;
#10064 = CARTESIAN_POINT ( 'NONE',  ( -10.37757302488623701, 73.77500000273120406, 31.93888565452638417 ) ) ;
#10065 = CARTESIAN_POINT ( 'NONE',  ( -33.58253175000000113, 7.225000002731182924, 10.91162601494193929 ) ) ;
#10066 = CARTESIAN_POINT ( 'NONE',  ( -23.41746824999999887, 14.12499999726882294, -2.867812753649727150E-15 ) ) ;
#10067 = CARTESIAN_POINT ( 'NONE',  ( 19.11951029504763611, 14.29725666759064318, -19.06425588902591173 ) ) ;
#10068 = EDGE_LOOP ( 'NONE', ( #18616, #17669, #31630, #5559 ) ) ;
#10069 = CARTESIAN_POINT ( 'NONE',  ( 20.75514604977248467, 44.42500000273120264, -28.56700777964554305 ) ) ;
#10070 = ORIENTED_EDGE ( 'NONE', *, *, #6408, .T. ) ;
#10071 = CARTESIAN_POINT ( 'NONE',  ( 26.00068869287367335, 30.76302083333332504, 15.01150461594596308 ) ) ;
#10072 = DIRECTION ( 'NONE',  ( 0.000000000000000000, 0.000000000000000000, 1.000000000000000000 ) ) ;
#10073 = CARTESIAN_POINT ( 'NONE',  ( 10.04305231718579705, 5.100000005462374197, 30.90933677959248982 ) ) ;
#10074 = CARTESIAN_POINT ( 'NONE',  ( -4.223320258572819786E-15, 9.499999999999992895, 24.50000000000000000 ) ) ;
#10075 = CARTESIAN_POINT ( 'NONE',  ( 23.41746824999999887, 1.124999997268810725, 0.000000000000000000 ) ) ;
#10076 = VECTOR ( 'NONE', #12847, 1000.000000000000000 ) ;
#10077 = CARTESIAN_POINT ( 'NONE',  ( -4.523095164977116484E-15, 14.12499999726881050, 24.62258325217400312 ) ) ;
#10078 = CARTESIAN_POINT ( 'NONE',  ( -20.75514604977248823, 13.07500000273120300, -28.56700777964554305 ) ) ;
#10079 = CARTESIAN_POINT ( 'NONE',  ( 10.04305231718579705, 19.10000000546238752, 30.90933677959248982 ) ) ;
#10080 = EDGE_CURVE ( 'NONE', #564, #25987, #25784, .T. ) ;
#10081 =( BOUNDED_CURVE ( )  B_SPLINE_CURVE ( 2, ( #33195, #10048, #20178, #6613, #30622, #7118, #22918, #4549, #17091, #17600, #12448, #27550, #4038 ),
 .UNSPECIFIED., .F., .T. ) 
 B_SPLINE_CURVE_WITH_KNOTS ( ( 3, 2, 2, 2, 2, 2, 3 ),
 ( 0.5500000000000000444, 0.5600000000000000533, 0.5799999999999999600, 0.5999999999999999778, 0.6199999999999999956, 0.6400000000000000133, 0.6500000000000000222 ),
 .UNSPECIFIED. ) 
 CURVE ( )  GEOMETRIC_REPRESENTATION_ITEM ( )  RATIONAL_B_SPLINE_CURVE ( ( 0.9755282581475768211, 0.9755282581475768211, 1.000000000000000000, 0.9510565162951535312, 1.000000000000000000, 0.9510565162951535312, 1.000000000000000000, 0.9510565162951535312, 1.000000000000000000, 0.9510565162951535312, 1.000000000000000000, 0.9755282581475768211, 0.9755282581475768211 ) ) 
 REPRESENTATION_ITEM ( '' )  );
#10082 = CARTESIAN_POINT ( 'NONE',  ( 20.08610463437157279, 65.29999999999999716, -27.64615127144129758 ) ) ;
#10083 = CARTESIAN_POINT ( 'NONE',  ( 24.50000000000000000, 11.74999999453762989, 0.000000000000000000 ) ) ;
#10084 = CARTESIAN_POINT ( 'NONE',  ( -10.04305231718579172, 29.60000000000001563, -30.90933677959248982 ) ) ;
#10085 = CARTESIAN_POINT ( 'NONE',  ( -0.04044903254990864921, 63.71131916759064495, 30.02300923189239867 ) ) ;
#10086 = CARTESIAN_POINT ( 'NONE',  ( -2.162160676586881955E-15, 32.87500000273118417, -35.31076352940723240 ) ) ;
#10087 = FACE_OUTER_BOUND ( 'NONE', #25979, .T. ) ;
#10088 = CARTESIAN_POINT ( 'NONE',  ( -7.505752307972844761, 38.35416666666666430, 28.01184896238304134 ) ) ;
#10089 = DIRECTION ( 'NONE',  ( 0.000000000000000000, 0.000000000000000000, 1.000000000000000000 ) ) ;
#10090 = EDGE_CURVE ( 'NONE', #11746, #25891, #7243, .T. ) ;
#10091 = CARTESIAN_POINT ( 'NONE',  ( -18.94512977948576093, 16.32499999726880091, 13.76444248337722698 ) ) ;
#10092 = CARTESIAN_POINT ( 'NONE',  ( 20.08610463437157279, 9.299999999999998934, -27.64615127144129758 ) ) ;
#10093 = DIRECTION ( 'NONE',  ( -1.224646799147353454E-16, 1.000000000000000000, -0.000000000000000000 ) ) ;
#10094 = CARTESIAN_POINT ( 'NONE',  ( 26.09010956794244507, 49.80690999907602645, 6.950374756619249084 ) ) ;
#10095 = CARTESIAN_POINT ( 'NONE',  ( 20.75514604977249178, 49.82500000273117990, 28.56700777964553950 ) ) ;
#10096 = CARTESIAN_POINT ( 'NONE',  ( -10.37757302488624411, 62.97500000273119269, -31.93888565452638417 ) ) ;
#10097 = CARTESIAN_POINT ( 'NONE',  ( -20.75514604977248823, 43.07500000273118701, -28.56700777964554305 ) ) ;
#10098 = CARTESIAN_POINT ( 'NONE',  ( 7.236395654485755280, 14.22499999726881192, 22.27133577429736988 ) ) ;
#10099 = FACE_OUTER_BOUND ( 'NONE', #30173, .T. ) ;
#10100 = DIRECTION ( 'NONE',  ( -0.000000000000000000, -1.000000000000000000, -0.000000000000000000 ) ) ;
#10101 = CARTESIAN_POINT ( 'NONE',  ( 32.50000000000000000, 77.00000000000000000, -3.980102097228898626E-15 ) ) ;
#10102 = CARTESIAN_POINT ( 'NONE',  ( 20.75514604977248467, 14.42500000273119021, -28.56700777964554305 ) ) ;
#10103 = CARTESIAN_POINT ( 'NONE',  ( 26.29305231718579350, 6.800000000000000711, 19.10302069950537529 ) ) ;
#10104 = FACE_OUTER_BOUND ( 'NONE', #17117, .T. ) ;
#10105 = CLOSED_SHELL ( 'NONE', ( #25625, #6835, #20931, #10408, #7750, #3421, #21827, #13530, #23304, #28199, #19493, #5189, #12156, #29681, #29828, #31587, #27193, #4853, #13262, #25709, #26367, #16701, #4459, #7122, #33155, #13221, #26664 ) ) ;
#10106 = CARTESIAN_POINT ( 'NONE',  ( 24.50000000000000000, 9.649999994537628467, 7.960532557706212486 ) ) ;
#10107 = CARTESIAN_POINT ( 'NONE',  ( -26.09010956794245217, 20.58815999907601935, -6.950374756619243755 ) ) ;
#10108 = CARTESIAN_POINT ( 'NONE',  ( -32.50000000000000000, 44.50000000546237544, 0.000000000000000000 ) ) ;
#10109 = CARTESIAN_POINT ( 'NONE',  ( -15.14183272437242067, 10.44999999453763095, -20.84094480462497856 ) ) ;
#10110 = CARTESIAN_POINT ( 'NONE',  ( -2.162160676586882350E-15, 24.62500000273118772, -35.31076352940722529 ) ) ;
#10111 = CARTESIAN_POINT ( 'NONE',  ( 10.37757302488624767, 65.97500000273120691, 31.93888565452638417 ) ) ;
#10112 = CARTESIAN_POINT ( 'NONE',  ( -24.20753774853730889, 35.34635416666666430, 13.97622843553633842 ) ) ;
#10113 = ORIENTED_EDGE ( 'NONE', *, *, #21593, .F. ) ;
#10114 = CARTESIAN_POINT ( 'NONE',  ( -27.16883889988624290, 70.92500000273120975, -19.73931689729374028 ) ) ;
#10115 = CARTESIAN_POINT ( 'NONE',  ( -30.02300923189239512, 49.38281249999997868, 2.654126918244515359E-13 ) ) ;
#10116 = CARTESIAN_POINT ( 'NONE',  ( 3.000384657911015469E-15, 16.99999999999998579, 24.50000000000000000 ) ) ;
#10117 = ORIENTED_EDGE ( 'NONE', *, *, #11873, .F. ) ;
#10118 = CARTESIAN_POINT ( 'NONE',  ( 7.468012846824777284, 56.69309000092396644, 28.02196122052045268 ) ) ;
#10119 = CARTESIAN_POINT ( 'NONE',  ( -24.22776226481240514, 64.28423583425730214, 13.94119854578937812 ) ) ;
#10120 = CARTESIAN_POINT ( 'NONE',  ( 33.58253175000000113, 10.12500000273118594, -4.112674001490185761E-15 ) ) ;
#10121 = CARTESIAN_POINT ( 'NONE',  ( -28.02196122052058413, 17.15065999907602290, -7.468012846824272799 ) ) ;
#10122 = CARTESIAN_POINT ( 'NONE',  ( 2.375766604868043697, 78.80125428700924317, 15.00000000000000178 ) ) ;
#10123 = CARTESIAN_POINT ( 'NONE',  ( -33.58253175000000113, 35.27500000273120406, -10.91162601494193218 ) ) ;
#10124 = CARTESIAN_POINT ( 'NONE',  ( 10.04305231718579705, 35.10000000546236976, 30.90933677959248982 ) ) ;
#10125 = CARTESIAN_POINT ( 'NONE',  ( -15.00000000000000000, 80.00000000000001421, 0.000000000000000000 ) ) ;
#10126 = CARTESIAN_POINT ( 'NONE',  ( 26.00068869287367335, 65.13802083333334281, 15.01150461594596308 ) ) ;
#10127 = CARTESIAN_POINT ( 'NONE',  ( 10.37757302488624767, 25.72500000273120335, 31.93888565452638417 ) ) ;
#10128 = CARTESIAN_POINT ( 'NONE',  ( -15.00000000000000000, 81.90000000000000568, -4.873795443493594171 ) ) ;
#10129 = CARTESIAN_POINT ( 'NONE',  ( 33.58253175000000113, 50.47500000273117848, -10.91162601494193751 ) ) ;
#10130 = SURFACE_STYLE_FILL_AREA ( #20612 ) ;
#10131 = CARTESIAN_POINT ( 'NONE',  ( -32.50000000000000000, 30.00000000000001421, 0.000000000000000000 ) ) ;
#10132 = CARTESIAN_POINT ( 'NONE',  ( 10.04305231718579705, 24.60000000000001208, 30.90933677959248982 ) ) ;
#10133 = CARTESIAN_POINT ( 'NONE',  ( 14.47279130897151767, 16.92499999726880944, -19.92008829642072598 ) ) ;
#10134 = CARTESIAN_POINT ( 'NONE',  ( 10.37757302488624056, 66.52500000273120406, -31.93888565452638417 ) ) ;
#10135 = DIRECTION ( 'NONE',  ( -1.224646799147353454E-16, 1.000000000000000000, -0.000000000000000000 ) ) ;
#10136 = CARTESIAN_POINT ( 'NONE',  ( -3.880418787951136483, 14.55125428154684997, -24.50000000000000000 ) ) ;
#10137 = CARTESIAN_POINT ( 'NONE',  ( -33.58253175000000113, 59.37500000273118417, 0.000000000000000000 ) ) ;
#10138 = CARTESIAN_POINT ( 'NONE',  ( 10.04305231718579705, 72.59999999999999432, 30.90933677959248982 ) ) ;
#10139 = CARTESIAN_POINT ( 'NONE',  ( -10.37757302488623701, 11.52500000273118452, 31.93888565452638417 ) ) ;
#10140 = CARTESIAN_POINT ( 'NONE',  ( -19.82091636218621389, 8.949999994537632730, 14.40073868116558842 ) ) ;
#10141 = CARTESIAN_POINT ( 'NONE',  ( -6.950374756619716266, 34.34934000092397355, -26.09010956794232428 ) ) ;
#10142 = CARTESIAN_POINT ( 'NONE',  ( 25.10896554811106540, 66.99999999999997158, -21.28139962774331906 ) ) ;
#10143 = CARTESIAN_POINT ( 'NONE',  ( -20.75514604977248112, 33.42500000273120264, 28.56700777964554661 ) ) ;
#10144 = FACE_OUTER_BOUND ( 'NONE', #7915, .T. ) ;
#10145 = CARTESIAN_POINT ( 'NONE',  ( 32.50000000000000711, 18.90000000000001279, 10.55989012756945122 ) ) ;
#10146 = CARTESIAN_POINT ( 'NONE',  ( -4.635254915624211769, 81.60000000000000853, -14.26584774442730286 ) ) ;
#10147 = CARTESIAN_POINT ( 'NONE',  ( 7.543491769121922985, 46.94232666574269075, 28.00173670424535644 ) ) ;
#10148 = CARTESIAN_POINT ( 'NONE',  ( 10.04305231718579705, 61.10000000546238397, 30.90933677959248982 ) ) ;
#10149 = AXIS2_PLACEMENT_3D ( 'NONE', #8702, #21766, #32209 ) ;
#10150 = CARTESIAN_POINT ( 'NONE',  ( 11.25946833292375793, 78.17500000273119554, 8.180482586598731842 ) ) ;
#10151 = CARTESIAN_POINT ( 'NONE',  ( 20.08610463437157279, 63.30000000000001137, -27.64615127144129758 ) ) ;
#10152 = CARTESIAN_POINT ( 'NONE',  ( -27.95245687107223986, 68.56993083240934084, 0.04044903255043252877 ) ) ;
#10153 = CARTESIAN_POINT ( 'NONE',  ( 5.147494310547426899, 63.94874572391551482, -32.50000000000000000 ) ) ;
#10154 = CARTESIAN_POINT ( 'NONE',  ( 32.50000000000000000, 73.50000000546236834, -3.980102097228898626E-15 ) ) ;
#10155 = CARTESIAN_POINT ( 'NONE',  ( 26.00068869287340334, 16.44010416666666430, -15.01150461594642316 ) ) ;
#10156 = CARTESIAN_POINT ( 'NONE',  ( -33.58253175000000113, 37.37500000273118417, 0.000000000000000000 ) ) ;
#10157 = CARTESIAN_POINT ( 'NONE',  ( 7.236395654485755280, 8.724999997268806595, 22.27133577429736988 ) ) ;
#10158 = EDGE_LOOP ( 'NONE', ( #20245, #7059, #24658, #22589 ) ) ;
#10159 = CARTESIAN_POINT ( 'NONE',  ( 10.37757302488624767, 75.97500000273119269, 31.93888565452638417 ) ) ;
#10160 = CARTESIAN_POINT ( 'NONE',  ( -10.04305231718579172, 22.10000000546237686, -30.90933677959248982 ) ) ;
#10161 = CARTESIAN_POINT ( 'NONE',  ( 26.00068869287367335, 44.51302083333331439, 15.01150461594596308 ) ) ;
#10162 = CARTESIAN_POINT ( 'NONE',  ( 26.00068869287340334, 64.56510416666667140, -15.01150461594642316 ) ) ;
#10163 = CARTESIAN_POINT ( 'NONE',  ( -20.75514604977248823, 55.07500000273117990, -28.56700777964554305 ) ) ;
#10164 = CARTESIAN_POINT ( 'NONE',  ( 20.08610463437158344, 63.20000000546237118, 27.64615127144129403 ) ) ;
#10165 = ORIENTED_EDGE ( 'NONE', *, *, #32350, .T. ) ;
#10166 = CARTESIAN_POINT ( 'NONE',  ( -1.778240108872766143E-15, 10.00000000546236834, -32.49999999999999289 ) ) ;
#10167 = CARTESIAN_POINT ( 'NONE',  ( -33.58253175000000113, 43.12500000273116996, 0.000000000000000000 ) ) ;
#10168 = CARTESIAN_POINT ( 'NONE',  ( -23.41746824999999887, 17.62499999726882649, -2.867812753649727150E-15 ) ) ;
#10169 = CARTESIAN_POINT ( 'NONE',  ( 20.75514604977249178, 70.07500000273120122, 28.56700777964553950 ) ) ;
#10170 = PRODUCT_RELATED_PRODUCT_CATEGORY ( 'part', '', ( #20871 ) ) ;
#10171 = CARTESIAN_POINT ( 'NONE',  ( -2.092463501923844636E-15, 4.000000005462377217, -34.17252228774368916 ) ) ;
#10172 = CARTESIAN_POINT ( 'NONE',  ( 27.16883889988624290, 63.92500000273120264, 19.73931689729373673 ) ) ;
#10173 = CARTESIAN_POINT ( 'NONE',  ( 15.01150461594643382, 13.86197916666666252, 26.00068869287340334 ) ) ;
#10174 =( GEOMETRIC_REPRESENTATION_CONTEXT ( 3 ) GLOBAL_UNCERTAINTY_ASSIGNED_CONTEXT ( ( #29833 ) ) GLOBAL_UNIT_ASSIGNED_CONTEXT ( ( #30188, #3785, #8759 ) ) REPRESENTATION_CONTEXT ( 'NONE', 'WORKASPACE' ) );
#10175 = CARTESIAN_POINT ( 'NONE',  ( 26.29305231718579350, 48.80000000000001137, 19.10302069950537529 ) ) ;
#10176 = CARTESIAN_POINT ( 'NONE',  ( 3.000384657911015469E-15, 0.000000000000000000, -24.50000000000000000 ) ) ;
#10177 = CARTESIAN_POINT ( 'NONE',  ( -27.16883889988623935, 11.57500000273120655, 19.73931689729374739 ) ) ;
#10178 = CARTESIAN_POINT ( 'NONE',  ( -26.29305231718579350, 73.80000000000001137, -19.10302069950537884 ) ) ;
#10179 = CARTESIAN_POINT ( 'NONE',  ( -6.950374756619247307, 30.04128499907601224, 26.09010956794245217 ) ) ;
#10180 = CARTESIAN_POINT ( 'NONE',  ( -13.91746824999999532, 79.27500000273118985, -4.522059556121115875 ) ) ;
#10181 = CARTESIAN_POINT ( 'NONE',  ( 4.635254915624212657, 74.85000000546237686, 14.26584774442730286 ) ) ;
#10182 = DIRECTION ( 'NONE',  ( -0.000000000000000000, 1.000000000000000000, -0.000000000000000000 ) ) ;
#10183 = CARTESIAN_POINT ( 'NONE',  ( 20.75514604977248467, 72.67500000273118133, -28.56700777964554305 ) ) ;
#10184 = ORIENTED_EDGE ( 'NONE', *, *, #23725, .F. ) ;
#10185 = CARTESIAN_POINT ( 'NONE',  ( -7.236395654485757944, 13.72499999726881015, -22.27133577429736988 ) ) ;
#10186 = CARTESIAN_POINT ( 'NONE',  ( -7.236395654485757944, 1.224999997268799712, -22.27133577429736988 ) ) ;
#10187 = CARTESIAN_POINT ( 'NONE',  ( 19.09188309203694800, 48.09375000000000000, 19.09188309203660694 ) ) ;
#10188 = VECTOR ( 'NONE', #22027, 1000.000000000000000 ) ;
#10189 = CARTESIAN_POINT ( 'NONE',  ( -33.58253175000000113, 57.22500000273117848, 10.91162601494193929 ) ) ;
#10190 = CARTESIAN_POINT ( 'NONE',  ( 33.58253175000000113, 16.47500000273118204, -10.91162601494193751 ) ) ;
#10191 = CARTESIAN_POINT ( 'NONE',  ( -20.75514604977248112, 7.675000002731199089, 28.56700777964554661 ) ) ;
#10192 = CARTESIAN_POINT ( 'NONE',  ( -6.988114217768288228, 29.47395833333332860, -26.07999730980477437 ) ) ;
#10193 = UNCERTAINTY_MEASURE_WITH_UNIT (LENGTH_MEASURE( 1.000000000000000082E-05 ), #10720, 'distance_accuracy_value', 'NONE');
#10194 = VECTOR ( 'NONE', #24325, 1000.000000000000000 ) ;
#10195 =( BOUNDED_CURVE ( )  B_SPLINE_CURVE ( 2, ( #26977, #1392, #32788, #17027, #21844, #11206, #9281, #11865, #19765, #8955, #24410, #32623, #24250 ),
 .UNSPECIFIED., .F., .T. ) 
 B_SPLINE_CURVE_WITH_KNOTS ( ( 3, 2, 2, 2, 2, 2, 3 ),
 ( 0.1388888888888888673, 0.1444444444444444309, 0.1555555555555555580, 0.1666666666666666574, 0.1777777777777777846, 0.1888888888888888840, 0.1944444444444444475 ),
 .UNSPECIFIED. ) 
 CURVE ( )  GEOMETRIC_REPRESENTATION_ITEM ( )  RATIONAL_B_SPLINE_CURVE ( ( 0.9755282581475768211, 0.9755282581475768211, 1.000000000000000000, 0.9510565162951535312, 1.000000000000000000, 0.9510565162951535312, 1.000000000000000000, 0.9510565162951535312, 1.000000000000000000, 0.9510565162951535312, 1.000000000000000000, 0.9755282581475768211, 0.9755282581475768211 ) ) 
 REPRESENTATION_ITEM ( '' )  );
#10196 = CARTESIAN_POINT ( 'NONE',  ( -7.468012846824771955, 24.03684000092397000, -28.02196122052045624 ) ) ;
#10197 = CARTESIAN_POINT ( 'NONE',  ( 7.505752307973351023, 65.56770833333332860, 28.01184896238290278 ) ) ;
#10198 = CARTESIAN_POINT ( 'NONE',  ( -26.29305231718579350, 78.30000000546237970, -19.10302069950537884 ) ) ;
#10199 = CARTESIAN_POINT ( 'NONE',  ( 30.28308157046064153, 52.00000000000001421, -13.46430247876119601 ) ) ;
#10200 = CARTESIAN_POINT ( 'NONE',  ( -20.08610463437156923, 42.30000000000000426, 27.64615127144130113 ) ) ;
#10201 = CARTESIAN_POINT ( 'NONE',  ( -33.58253175000000113, 45.02500000273117564, -10.91162601494193041 ) ) ;
#10202 = CARTESIAN_POINT ( 'NONE',  ( 7.236395654485755280, 8.224999997268806595, 22.27133577429736988 ) ) ;
#10203 = CARTESIAN_POINT ( 'NONE',  ( 15.00000000000000000, 79.00000000000001421, -1.836970198721029589E-15 ) ) ;
#10204 = ORIENTED_EDGE ( 'NONE', *, *, #28242, .F. ) ;
#10205 = CARTESIAN_POINT ( 'NONE',  ( -20.75514604977248823, 51.07500000273116569, -28.56700777964554305 ) ) ;
#10206 = CARTESIAN_POINT ( 'NONE',  ( 6.950374756619721595, 46.38059000092397355, 26.09010956794232428 ) ) ;
#10207 = CARTESIAN_POINT ( 'NONE',  ( -2.162160676586881955E-15, 72.87500000273115575, -35.31076352940723240 ) ) ;
#10208 = ORIENTED_EDGE ( 'NONE', *, *, #31652, .T. ) ;
#10209 = CARTESIAN_POINT ( 'NONE',  ( -27.16883889988624290, 24.92500000273119198, -19.73931689729374028 ) ) ;
#10210 = CARTESIAN_POINT ( 'NONE',  ( 20.50609665440969565, 12.85937500000000000, -20.50609665441004736 ) ) ;
#10211 = ORIENTED_EDGE ( 'NONE', *, *, #30533, .F. ) ;
#10212 = VECTOR ( 'NONE', #9829, 1000.000000000000114 ) ;
#10213 = CARTESIAN_POINT ( 'NONE',  ( -10.04305231718578462, 14.90000000546237757, 30.90933677959249337 ) ) ;
#10214 = CARTESIAN_POINT ( 'NONE',  ( 27.16883889988624290, 59.92500000273118133, 19.73931689729373673 ) ) ;
#10215 = CARTESIAN_POINT ( 'NONE',  ( 15.01150461594596308, 40.21614583333332860, -26.00068869287367335 ) ) ;
#10216 = CARTESIAN_POINT ( 'NONE',  ( -24.50000000000000000, 17.00000000000001421, -3.000384657911015469E-15 ) ) ;
#10217 = CARTESIAN_POINT ( 'NONE',  ( 18.94512977948575738, 4.924999997268808549, 13.76444248337723408 ) ) ;
#10218 = EDGE_CURVE ( 'NONE', #1559, #28004, #13288, .T. ) ;
#10219 = CARTESIAN_POINT ( 'NONE',  ( 6.486482029760649416E-15, 3.625000002731181059, 35.31076352940723240 ) ) ;
#10220 = CARTESIAN_POINT ( 'NONE',  ( 1.469576158976824144E-15, 102.0000000000000284, 12.00000000000000178 ) ) ;
#10221 = CARTESIAN_POINT ( 'NONE',  ( 20.53372385742108008, 56.96836833240936215, 20.47846945139866648 ) ) ;
#10222 = CARTESIAN_POINT ( 'NONE',  ( -15.00000000000000000, 72.09999999999999432, 4.873795443493597723 ) ) ;
#10223 = CARTESIAN_POINT ( 'NONE',  ( -20.50609665440969209, 66.14062500000000000, 20.50609665441005092 ) ) ;
#10224 = CARTESIAN_POINT ( 'NONE',  ( -3.880418787951136483, 14.30125427608446920, -24.50000000000000000 ) ) ;
#10225 = CARTESIAN_POINT ( 'NONE',  ( 32.50000000000000711, 14.89999999999999680, 10.55989012756945122 ) ) ;
#10226 = CARTESIAN_POINT ( 'NONE',  ( 7.570916362186207671, 11.34999999453761887, 23.30088464923126779 ) ) ;
#10227 = CARTESIAN_POINT ( 'NONE',  ( 4.635254915624212657, 72.85000000546237686, 14.26584774442730286 ) ) ;
#10228 = CARTESIAN_POINT ( 'NONE',  ( 13.97622843553589966, 19.59114583333332149, -24.20753774853756113 ) ) ;
#10229 = CARTESIAN_POINT ( 'NONE',  ( 33.58253175000000113, 32.22500000273117848, -10.91162601494193751 ) ) ;
#10230 = CARTESIAN_POINT ( 'NONE',  ( 2.445080149700053643E-15, 74.49999999999998579, 15.00000000000000000 ) ) ;
#10231 = CARTESIAN_POINT ( 'NONE',  ( 27.16883889988624290, 34.17500000273120264, 19.73931689729373673 ) ) ;
#10232 = CARTESIAN_POINT ( 'NONE',  ( -27.16883889988623935, 23.57500000273119056, 19.73931689729374739 ) ) ;
#10233 = CARTESIAN_POINT ( 'NONE',  ( 1.093617666956751375E-13, 67.50000000000001421, -32.50000000000000711 ) ) ;
#10234 = CARTESIAN_POINT ( 'NONE',  ( 10.37757302488624767, 77.72500000273119269, 31.93888565452638417 ) ) ;
#10235 = CARTESIAN_POINT ( 'NONE',  ( -32.50000000000000000, 66.10000000000000853, 10.55989012756946366 ) ) ;
#10236 = CARTESIAN_POINT ( 'NONE',  ( 32.50000000000000000, 58.99999999999998579, -3.980102097228898626E-15 ) ) ;
#10237 = CARTESIAN_POINT ( 'NONE',  ( 14.47279130897151767, 18.32499999726882578, 19.92008829642072953 ) ) ;
#10238 = CARTESIAN_POINT ( 'NONE',  ( -10.37757302488624411, 64.72500000273117848, -31.93888565452638417 ) ) ;
#10239 = CARTESIAN_POINT ( 'NONE',  ( 23.41746824999999887, 9.124999997268817609, 0.000000000000000000 ) ) ;
#10240 = AXIS2_PLACEMENT_3D ( 'NONE', #8569, #27266, #501 ) ;
#10241 = CARTESIAN_POINT ( 'NONE',  ( 27.16883889988623935, 72.57500000273118701, -19.73931689729374384 ) ) ;
#10242 = CARTESIAN_POINT ( 'NONE',  ( 33.58253175000000823, 10.02500000273118275, 10.91162601494192685 ) ) ;
#10243 = CARTESIAN_POINT ( 'NONE',  ( 1.507698388325705758E-15, 15.62499999726882116, -24.62258325217400312 ) ) ;
#10244 = CARTESIAN_POINT ( 'NONE',  ( 7.025853678916403666, 10.57329833425730747, -26.06988505166735237 ) ) ;
#10245 = ORIENTED_EDGE ( 'NONE', *, *, #18742, .T. ) ;
#10246 = CARTESIAN_POINT ( 'NONE',  ( -33.58253175000000113, 45.12500000273119127, 0.000000000000000000 ) ) ;
#10247 = ORIENTED_EDGE ( 'NONE', *, *, #5383, .F. ) ;
#10248 = CARTESIAN_POINT ( 'NONE',  ( 2.740863092043355209E-13, 41.64843750000000000, 30.02300923189239512 ) ) ;
#10249 = LINE ( 'NONE', #12816, #4558 ) ;
#10250 = CARTESIAN_POINT ( 'NONE',  ( 26.29305231718579350, 1.300000005462376151, 19.10302069950537529 ) ) ;
#10251 = CARTESIAN_POINT ( 'NONE',  ( 20.75514604977248467, 78.42500000273116711, -28.56700777964554305 ) ) ;
#10252 = CARTESIAN_POINT ( 'NONE',  ( 23.41746825000000243, 3.024999997268812635, 7.608796670333735079 ) ) ;
#10253 = CARTESIAN_POINT ( 'NONE',  ( 23.41746825000000243, 16.52499999726882152, 7.608796670333735079 ) ) ;
#10254 = CARTESIAN_POINT ( 'NONE',  ( 10.37757302488624767, 17.97500000273119625, 31.93888565452638417 ) ) ;
#10255 = CARTESIAN_POINT ( 'NONE',  ( -10.04305231718579172, 18.10000000546238397, -30.90933677959248982 ) ) ;
#10256 = CARTESIAN_POINT ( 'NONE',  ( 32.50000000000000711, 66.90000000000001990, 10.55989012756945122 ) ) ;
#10257 = CARTESIAN_POINT ( 'NONE',  ( -10.04305231718578462, 30.39999999999998437, 30.90933677959249337 ) ) ;
#10258 = CARTESIAN_POINT ( 'NONE',  ( -2.584737979205441561E-13, 12.42968749999999289, -30.02300923189239512 ) ) ;
#10259 = CARTESIAN_POINT ( 'NONE',  ( 10.11607355459420710, -70.99969134886156041, 1.238861709857297692E-15 ) ) ;
#10260 = CARTESIAN_POINT ( 'NONE',  ( 30.02300923189239867, 37.35156249999999289, -2.619432448724978208E-13 ) ) ;
#10261 = SHAPE_DEFINITION_REPRESENTATION ( #20558, #31529 ) ;
#10262 = DIRECTION ( 'NONE',  ( -0.000000000000000000, -1.000000000000000000, -0.000000000000000000 ) ) ;
#10263 = CARTESIAN_POINT ( 'NONE',  ( -7.236395654485757944, 17.72499999726881370, -22.27133577429736988 ) ) ;
#10264 = CARTESIAN_POINT ( 'NONE',  ( -10.04305231718578462, 6.400000000000016342, 30.90933677959249337 ) ) ;
#10265 = CYLINDRICAL_SURFACE ( 'NONE', #2837, 32.50000000000000000 ) ;
#10266 = CARTESIAN_POINT ( 'NONE',  ( 7.025853678916867295, 53.81732666574268364, 26.06988505166722803 ) ) ;
#10267 = CARTESIAN_POINT ( 'NONE',  ( -27.16883889988623935, 51.32500000273118701, 19.73931689729374739 ) ) ;
#10268 = CARTESIAN_POINT ( 'NONE',  ( -27.16883889988624290, 63.17500000273117422, -19.73931689729374028 ) ) ;
#10269 = CARTESIAN_POINT ( 'NONE',  ( 10.37757302488624767, 37.97500000273118559, 31.93888565452638417 ) ) ;
#10270 = DIRECTION ( 'NONE',  ( -0.000000000000000000, 1.000000000000000000, -0.000000000000000000 ) ) ;
#10271 = AXIS2_PLACEMENT_3D ( 'NONE', #25040, #24537, #6174 ) ;
#10272 = DIRECTION ( 'NONE',  ( -0.7071067811865526798, 0.000000000000000000, -0.7071067811865423547 ) ) ;
#10273 = LINE ( 'NONE', #15938, #9763 ) ;
#10274 = CARTESIAN_POINT ( 'NONE',  ( 10.04305231718579705, 51.10000000546238397, 30.90933677959248982 ) ) ;
#10275 = DIRECTION ( 'NONE',  ( 0.000000000000000000, 0.000000000000000000, 1.000000000000000000 ) ) ;
#10276 = CARTESIAN_POINT ( 'NONE',  ( -2.162160676586881955E-15, 18.62500000273117351, -35.31076352940723240 ) ) ;
#10277 = CARTESIAN_POINT ( 'NONE',  ( -20.08610463437156923, 62.80000000546237260, 27.64615127144130113 ) ) ;
#10278 = CARTESIAN_POINT ( 'NONE',  ( 1.836970198721029589E-15, 82.00000000000001421, 15.00000000000000000 ) ) ;
#10279 = CARTESIAN_POINT ( 'NONE',  ( -20.08610463437156923, 40.30000000000001137, 27.64615127144130113 ) ) ;
#10280 = CARTESIAN_POINT ( 'NONE',  ( -0.04044903255042732459, 17.86680583240935860, -27.95245687107223986 ) ) ;
#10281 = CARTESIAN_POINT ( 'NONE',  ( 32.50000000000000711, 33.40000000546238113, 10.55989012756945122 ) ) ;
#10282 = ADVANCED_FACE ( 'NONE', ( #27851 ), #25620, .F. ) ;
#10283 = CARTESIAN_POINT ( 'NONE',  ( 7.570916362186207671, 17.34999999453762243, 23.30088464923126779 ) ) ;
#10284 = CARTESIAN_POINT ( 'NONE',  ( -27.16883889988623935, 27.32500000273119412, 19.73931689729374739 ) ) ;
#10285 = CARTESIAN_POINT ( 'NONE',  ( -19.09188309203660694, 42.07812499999999289, 19.09188309203694800 ) ) ;
#10286 = EDGE_CURVE ( 'NONE', #10883, #14665, #15501, .T. ) ;
#10287 = ORIENTED_EDGE ( 'NONE', *, *, #31033, .T. ) ;
#10288 = CARTESIAN_POINT ( 'NONE',  ( -20.75514604977248112, 59.42500000273118843, 28.56700777964554661 ) ) ;
#10289 = CARTESIAN_POINT ( 'NONE',  ( -7.505752307972844761, 48.66666666666666430, 28.01184896238304134 ) ) ;
#10290 = SHAPE_REPRESENTATION ( 'plain washer hardened_iso_Washer ISO 7415 - 30', ( #1376 ), #23828 ) ;
#10291 = ORIENTED_EDGE ( 'NONE', *, *, #33593, .T. ) ;
#10292 = CARTESIAN_POINT ( 'NONE',  ( -2.584737979205441561E-13, 15.86718749999999645, -30.02300923189239512 ) ) ;
#10293 = CARTESIAN_POINT ( 'NONE',  ( -26.02091320914849959, 16.15923583425731636, 14.97647472619947528 ) ) ;
#10294 = CARTESIAN_POINT ( 'NONE',  ( 20.75514604977249178, 1.825000002731179460, 28.56700777964553950 ) ) ;
#10295 = CARTESIAN_POINT ( 'NONE',  ( -1.778240108872766143E-15, 46.00000000546238255, -32.49999999999999289 ) ) ;
#10296 = CARTESIAN_POINT ( 'NONE',  ( 33.58253175000000823, 32.27500000273117564, 10.91162601494192863 ) ) ;
#10297 = CARTESIAN_POINT ( 'NONE',  ( -32.50000000000000000, 40.50000000546238965, 0.000000000000000000 ) ) ;
#10298 = CARTESIAN_POINT ( 'NONE',  ( -9.657523855033125146E-16, 75.50000000000001421, -15.77193336357400710 ) ) ;
#10299 = CARTESIAN_POINT ( 'NONE',  ( -5.147494310547423346, 48.44874571845315359, 32.50000000000000000 ) ) ;
#10300 = CARTESIAN_POINT ( 'NONE',  ( -27.16883889988623935, 25.32500000273119056, 19.73931689729374739 ) ) ;
#10301 = DIRECTION ( 'NONE',  ( -0.000000000000000000, -1.000000000000000000, -0.000000000000000000 ) ) ;
#10302 = CARTESIAN_POINT ( 'NONE',  ( 10.37757302488624767, 49.97500000273119269, 31.93888565452638417 ) ) ;
#10303 = CARTESIAN_POINT ( 'NONE',  ( -10.04305231718578462, 28.39999999999999503, 30.90933677959249337 ) ) ;
#10304 = CARTESIAN_POINT ( 'NONE',  ( -2.092463501923844636E-15, 25.50000000000001066, -34.17252228774368916 ) ) ;
#10305 = CARTESIAN_POINT ( 'NONE',  ( 19.82091636218621034, 3.799999999999998046, 14.40073868116559730 ) ) ;
#10306 = CARTESIAN_POINT ( 'NONE',  ( 10.37757302488624767, 71.72500000273119269, 31.93888565452638417 ) ) ;
#10307 = CARTESIAN_POINT ( 'NONE',  ( -10.04305231718579172, 77.60000000000000853, -30.90933677959248982 ) ) ;
#10308 = CARTESIAN_POINT ( 'NONE',  ( -7.570916362186210335, 14.60000000000000142, -23.30088464923126779 ) ) ;
#10309 = CARTESIAN_POINT ( 'NONE',  ( 20.75514604977249178, 58.07500000273117990, 28.56700777964553950 ) ) ;
#10310 = CARTESIAN_POINT ( 'NONE',  ( -1.778240108872766143E-15, 40.00000000546237544, -32.49999999999999289 ) ) ;
#10311 = CARTESIAN_POINT ( 'NONE',  ( -33.58253175000000113, 11.02500000273117919, -10.91162601494193218 ) ) ;
#10312 = CARTESIAN_POINT ( 'NONE',  ( -6.950374756619716266, 27.47434000092397000, -26.09010956794232428 ) ) ;
#10313 = DIRECTION ( 'NONE',  ( 0.000000000000000000, -1.000000000000000000, 0.000000000000000000 ) ) ;
#10314 = CARTESIAN_POINT ( 'NONE',  ( -33.58253175000000113, 33.22500000273117138, 10.91162601494193929 ) ) ;
#10315 = CARTESIAN_POINT ( 'NONE',  ( 5.147494310547535257, 57.44874571845314648, -32.49999999999996447 ) ) ;
#10316 = DIRECTION ( 'NONE',  ( 1.000000000000000000, 0.000000000000000000, 1.224646799147353700E-16 ) ) ;
#10317 = CARTESIAN_POINT ( 'NONE',  ( 4.300734207923757602, 74.27500000273118985, -13.23629886949340673 ) ) ;
#10318 = CARTESIAN_POINT ( 'NONE',  ( 7.543491769121922985, 50.37982666574269075, 28.00173670424535644 ) ) ;
#10319 = CARTESIAN_POINT ( 'NONE',  ( -32.50000000000000000, 52.60000000546235555, 10.55989012756946366 ) ) ;
#10320 = AXIS2_PLACEMENT_3D ( 'NONE', #1118, #21915, #11438 ) ;
#10321 = EDGE_CURVE ( 'NONE', #32300, #30131, #29906, .T. ) ;
#10322 = CARTESIAN_POINT ( 'NONE',  ( 13.91746824999999887, 76.37500000273116996, -1.704398294459741270E-15 ) ) ;
#10323 = SURFACE_STYLE_USAGE ( .BOTH. , #13579 ) ;
#10324 = CARTESIAN_POINT ( 'NONE',  ( 26.07999730980477437, 13.14583333333332860, -6.988114217768290004 ) ) ;
#10325 = CARTESIAN_POINT ( 'NONE',  ( -10.04305231718578462, 54.40000000000000568, 30.90933677959249337 ) ) ;
#10326 = EDGE_CURVE ( 'NONE', #12037, #17796, #13496, .T. ) ;
#10327 = CARTESIAN_POINT ( 'NONE',  ( -32.50000000000000000, 66.50000000546238255, 0.000000000000000000 ) ) ;
#10328 = CARTESIAN_POINT ( 'NONE',  ( -28.01184896238290278, 21.73958333333332860, 7.505752307973363457 ) ) ;
#10329 = CARTESIAN_POINT ( 'NONE',  ( 6.486482029760649416E-15, 37.87500000273117706, 35.31076352940723240 ) ) ;
#10330 = CARTESIAN_POINT ( 'NONE',  ( -14.47279130897152299, 6.424999997268821872, 19.92008829642072243 ) ) ;
#10331 = ORIENTED_EDGE ( 'NONE', *, *, #6211, .T. ) ;
#10332 = CARTESIAN_POINT ( 'NONE',  ( -20.75514604977248823, 73.07500000273115859, -28.56700777964554305 ) ) ;
#10333 = CARTESIAN_POINT ( 'NONE',  ( 26.29305231718579350, 23.30000000546238326, 19.10302069950537529 ) ) ;
#10334 = CARTESIAN_POINT ( 'NONE',  ( -7.505752307973343918, 39.78645833333332860, -28.01184896238290989 ) ) ;
#10335 = CARTESIAN_POINT ( 'NONE',  ( 7.505752307973351023, 58.69270833333332860, 28.01184896238290278 ) ) ;
#10336 = CARTESIAN_POINT ( 'NONE',  ( 20.75514604977249178, 52.07500000273119412, 28.56700777964553950 ) ) ;
#10337 = CARTESIAN_POINT ( 'NONE',  ( 20.08610463437158344, 57.20000000546237828, 27.64615127144129403 ) ) ;
#10338 = CARTESIAN_POINT ( 'NONE',  ( -5.147494310547430452, 10.05125428700921653, -32.49999999999999289 ) ) ;
#10339 = CARTESIAN_POINT ( 'NONE',  ( -27.16883889988624290, 44.92500000273119554, -19.73931689729374028 ) ) ;
#10340 = CARTESIAN_POINT ( 'NONE',  ( -30.16025403784430736, -22.00000000000000000, 0.000000000000000000 ) ) ;
#10341 = CARTESIAN_POINT ( 'NONE',  ( -27.16883889988623935, 65.57500000273120122, 19.73931689729374739 ) ) ;
#10342 = CARTESIAN_POINT ( 'NONE',  ( 20.08610463437158344, 7.200000005462393382, 27.64615127144129403 ) ) ;
#10343 = CARTESIAN_POINT ( 'NONE',  ( 20.75514604977249178, 59.82500000273117280, 28.56700777964553950 ) ) ;
#10344 = CARTESIAN_POINT ( 'NONE',  ( -30.02300923189239867, 15.00781249999999645, 2.654126918244514854E-13 ) ) ;
#10345 = CARTESIAN_POINT ( 'NONE',  ( 32.50000000000000000, 45.10000000000000853, -10.55989012756945833 ) ) ;
#10346 = CARTESIAN_POINT ( 'NONE',  ( 14.47279130897151589, 2.324999997268805796, 19.92008829642072953 ) ) ;
#10347 = CARTESIAN_POINT ( 'NONE',  ( 6.486482029760649416E-15, 11.87500000273118062, 35.31076352940723240 ) ) ;
#10348 = CARTESIAN_POINT ( 'NONE',  ( 24.22776226481265383, 32.76263916574268364, 13.94119854578893580 ) ) ;
#10349 = CARTESIAN_POINT ( 'NONE',  ( -8.601468415847518756, 77.07500000273117280, -11.83890561707634781 ) ) ;
#10350 = CARTESIAN_POINT ( 'NONE',  ( 0.000000000000000000, 0.000000000000000000, 0.000000000000000000 ) ) ;
#10351 = DIRECTION ( 'NONE',  ( -0.000000000000000000, -1.000000000000000000, -0.000000000000000000 ) ) ;
#10352 = CARTESIAN_POINT ( 'NONE',  ( -10.37757302488623701, 73.77500000273120406, 31.93888565452638417 ) ) ;
#10353 = ORIENTED_EDGE ( 'NONE', *, *, #20920, .T. ) ;
#10354 = CARTESIAN_POINT ( 'NONE',  ( 23.41746825000000243, 11.22499999726881548, -7.608796670333727974 ) ) ;
#10355 = CARTESIAN_POINT ( 'NONE',  ( -19.09188309203694445, 60.12500000000000000, -19.09188309203661049 ) ) ;
#10356 = CARTESIAN_POINT ( 'NONE',  ( 6.486482029760649416E-15, 53.62500000273119838, 35.31076352940723240 ) ) ;
#10357 = CARTESIAN_POINT ( 'NONE',  ( 20.75514604977249178, 20.07500000273118346, 28.56700777964553950 ) ) ;
#10358 = CARTESIAN_POINT ( 'NONE',  ( 27.16883889988623935, 2.575000002731184345, -19.73931689729374384 ) ) ;
#10359 = CARTESIAN_POINT ( 'NONE',  ( -26.07999730980490583, 42.65104166666666430, -6.988114217767815717 ) ) ;
#10360 = CARTESIAN_POINT ( 'NONE',  ( 20.53372385742072481, 24.60975666759063785, -20.47846945139902175 ) ) ;
#10361 = CARTESIAN_POINT ( 'NONE',  ( 15.04653450569339945, 19.29909749907602290, 25.98046417659831775 ) ) ;
#10362 = CARTESIAN_POINT ( 'NONE',  ( 33.58253175000000823, 4.025000002731196957, 10.91162601494192863 ) ) ;
#10363 = CARTESIAN_POINT ( 'NONE',  ( 12.54892211412375680, 52.00000000000002842, -30.22116052075408987 ) ) ;
#10364 = CARTESIAN_POINT ( 'NONE',  ( 33.58253175000000823, 44.02500000273118275, 10.91162601494192685 ) ) ;
#10365 = CARTESIAN_POINT ( 'NONE',  ( 14.47279130897151589, 8.324999997268818674, 19.92008829642072953 ) ) ;
#10366 = CARTESIAN_POINT ( 'NONE',  ( -1.778240108872766143E-15, 64.00000000546238255, -32.49999999999999289 ) ) ;
#10367 = EDGE_LOOP ( 'NONE', ( #16211, #11377 ) ) ;
#10368 = CARTESIAN_POINT ( 'NONE',  ( 27.16883889988624290, 52.17500000273118843, 19.73931689729373673 ) ) ;
#10369 = CARTESIAN_POINT ( 'NONE',  ( 5.147494310547434893, 59.05125428700922896, 32.49999999999999289 ) ) ;
#10370 = CARTESIAN_POINT ( 'NONE',  ( 13.94119854578937812, 39.36236083425731636, 24.22776226481240514 ) ) ;
#10371 = CARTESIAN_POINT ( 'NONE',  ( -10.37757302488624411, 78.97500000273119269, -31.93888565452638417 ) ) ;
#10372 = ORIENTED_EDGE ( 'NONE', *, *, #22463, .T. ) ;
#10373 = CARTESIAN_POINT ( 'NONE',  ( -20.75514604977248823, 22.82500000273118701, -28.56700777964554305 ) ) ;
#10374 = CARTESIAN_POINT ( 'NONE',  ( 28.01184896238304134, 13.43229166666666607, 7.505752307972846538 ) ) ;
#10375 = VERTEX_POINT ( 'NONE', #7075 ) ;
#10376 = CARTESIAN_POINT ( 'NONE',  ( 5.147494310547426899, 29.94874572391553258, -32.50000000000000000 ) ) ;
#10377 = CARTESIAN_POINT ( 'NONE',  ( -20.75514604977248823, 62.82500000273119412, -28.56700777964554305 ) ) ;
#10378 = CARTESIAN_POINT ( 'NONE',  ( -15.01150461594642138, 46.51822916666666430, -26.00068869287340334 ) ) ;
#10379 = CARTESIAN_POINT ( 'NONE',  ( -15.14183272437242778, 7.049999994537622605, 20.84094480462497856 ) ) ;
#10380 = CYLINDRICAL_SURFACE ( 'NONE', #33589, 33.00000000000000000 ) ;
#10381 = CARTESIAN_POINT ( 'NONE',  ( 20.75514604977248467, 6.425000002731179549, -28.56700777964554305 ) ) ;
#10382 = CARTESIAN_POINT ( 'NONE',  ( -24.50000000000000711, 6.849999994537629533, 7.960532557706201828 ) ) ;
#10383 = CARTESIAN_POINT ( 'NONE',  ( 20.53372385742108008, 63.84336833240935505, 20.47846945139866648 ) ) ;
#10384 = CARTESIAN_POINT ( 'NONE',  ( -24.50000000000000711, 15.09999999999998899, 7.960532557706201828 ) ) ;
#10385 = CARTESIAN_POINT ( 'NONE',  ( 28.01184896238290278, 64.70833333333334281, -7.505752307973347470 ) ) ;
#10386 = CARTESIAN_POINT ( 'NONE',  ( 20.08610463437157279, 9.299999999999995381, -27.64615127144129758 ) ) ;
#10387 = CARTESIAN_POINT ( 'NONE',  ( 10.04305231718579705, 14.59999999999998721, 30.90933677959248982 ) ) ;
#10388 = CARTESIAN_POINT ( 'NONE',  ( 19.09188309203661049, 64.42187499999998579, -19.09188309203694445 ) ) ;
#10389 = CARTESIAN_POINT ( 'NONE',  ( 7.570916362186213000, 12.14999999453761426, -23.30088464923126423 ) ) ;
#10390 = CARTESIAN_POINT ( 'NONE',  ( 8.601468415847516980, 80.17500000273116711, -11.83890561707634781 ) ) ;
#10391 = CARTESIAN_POINT ( 'NONE',  ( -13.97622843553588901, 31.62239583333332860, 24.20753774853756823 ) ) ;
#10392 = CARTESIAN_POINT ( 'NONE',  ( -33.58253175000000113, 31.02500000273118630, -10.91162601494193218 ) ) ;
#10393 = CARTESIAN_POINT ( 'NONE',  ( -27.16883889988623935, 71.32500000273118701, 19.73931689729374739 ) ) ;
#10394 = CARTESIAN_POINT ( 'NONE',  ( -10.37757302488623701, 33.77500000273118985, 31.93888565452638417 ) ) ;
#10395 = CARTESIAN_POINT ( 'NONE',  ( 27.16883889988624290, 18.17500000273120264, 19.73931689729373673 ) ) ;
#10396 = CARTESIAN_POINT ( 'NONE',  ( -5.147494310547377161, 67.55125428154684641, -32.50000000000002132 ) ) ;
#10397 = CARTESIAN_POINT ( 'NONE',  ( -26.06988505166735237, 47.52642333425731636, -7.025853678916388567 ) ) ;
#10398 = CARTESIAN_POINT ( 'NONE',  ( -27.16883889988624290, 76.92500000273119554, -19.73931689729374028 ) ) ;
#10399 = DIRECTION ( 'NONE',  ( -0.000000000000000000, -1.000000000000000000, -0.000000000000000000 ) ) ;
#10400 = CARTESIAN_POINT ( 'NONE',  ( 6.277390505771533514E-15, 62.50000000000000000, 34.17252228774368916 ) ) ;
#10401 = CARTESIAN_POINT ( 'NONE',  ( -23.41746824999999887, 17.52499999726881796, -7.608796670333730638 ) ) ;
#10402 = CARTESIAN_POINT ( 'NONE',  ( -33.58253175000000113, 65.12500000273119838, 0.000000000000000000 ) ) ;
#10403 = CARTESIAN_POINT ( 'NONE',  ( 7.236395654485755280, 6.724999997268804819, 22.27133577429736988 ) ) ;
#10404 = CARTESIAN_POINT ( 'NONE',  ( -33.58253175000000113, 75.27500000273118985, -10.91162601494193218 ) ) ;
#10405 = CARTESIAN_POINT ( 'NONE',  ( -10.37757302488624411, 4.725000002731183812, -31.93888565452638417 ) ) ;
#10406 = CARTESIAN_POINT ( 'NONE',  ( -23.41746825000000598, 18.22499999726879949, 7.608796670333726198 ) ) ;
#10407 = CARTESIAN_POINT ( 'NONE',  ( 0.04044903254993986036, 10.43006916759064495, -27.95245687107223986 ) ) ;
#10408 = ADVANCED_FACE ( 'NONE', ( #28016 ), #20825, .F. ) ;
#10409 = ORIENTED_EDGE ( 'NONE', *, *, #11255, .T. ) ;
#10410 = CARTESIAN_POINT ( 'NONE',  ( 20.75514604977249178, 45.82500000273118701, 28.56700777964553950 ) ) ;
#10411 = EDGE_LOOP ( 'NONE', ( #23839, #23627, #18896, #13145 ) ) ;
#10412 = CARTESIAN_POINT ( 'NONE',  ( 2.740863092043355209E-13, 45.08593750000000711, 30.02300923189239512 ) ) ;
#10413 = CARTESIAN_POINT ( 'NONE',  ( -20.08610463437157989, 79.70000000000000284, -27.64615127144129758 ) ) ;
#10414 = CARTESIAN_POINT ( 'NONE',  ( 20.08610463437157279, 3.800000005462383257, -27.64615127144129758 ) ) ;
#10415 = CARTESIAN_POINT ( 'NONE',  ( 6.486482029760649416E-15, 77.62500000273121259, 35.31076352940723240 ) ) ;
#10416 = CARTESIAN_POINT ( 'NONE',  ( -4.523095164977116484E-15, 6.624999997268815832, 24.62258325217400312 ) ) ;
#10417 = EDGE_CURVE ( 'NONE', #390, #23284, #33423, .T. ) ;
#10418 = CARTESIAN_POINT ( 'NONE',  ( -18.94512977948575738, 15.42499999726881832, -13.76444248337723231 ) ) ;
#10419 = CARTESIAN_POINT ( 'NONE',  ( 27.16883889988624290, 18.17500000273120264, 19.73931689729373673 ) ) ;
#10420 = CARTESIAN_POINT ( 'NONE',  ( -10.04305231718579172, 57.59999999999998721, -30.90933677959248982 ) ) ;
#10421 = CARTESIAN_POINT ( 'NONE',  ( -1.089172066684569321E-14, 76.75000000546238255, 15.00000000000000000 ) ) ;
#10422 = DIRECTION ( 'NONE',  ( 0.000000000000000000, 0.000000000000000000, -1.000000000000000000 ) ) ;
#10423 = CARTESIAN_POINT ( 'NONE',  ( -20.47846945139866648, 37.20274333240935505, 20.53372385742108008 ) ) ;
#10424 = CARTESIAN_POINT ( 'NONE',  ( -4.300734207923759378, 76.97500000273119269, -13.23629886949340495 ) ) ;
#10425 = CARTESIAN_POINT ( 'NONE',  ( -28.01184896238304134, 35.77604166666666430, -7.505752307972844761 ) ) ;
#10426 = APPLICATION_PROTOCOL_DEFINITION ( 'draft international standard', 'automotive_design', 1998, #19086 ) ;
#10427 = ADVANCED_FACE ( 'NONE', ( #26635 ), #7763, .T. ) ;
#10428 = DIRECTION ( 'NONE',  ( 0.000000000000000000, 1.000000000000000000, 0.000000000000000000 ) ) ;
#10429 = CARTESIAN_POINT ( 'NONE',  ( 5.779280353836490358E-15, 68.50000000000000000, 32.49999999999999289 ) ) ;
#10430 = CARTESIAN_POINT ( 'NONE',  ( 32.50000000000000711, 6.900000000000014566, 10.55989012756945122 ) ) ;
#10431 = DIRECTION ( 'NONE',  ( -1.224646799147353454E-16, 1.000000000000000000, -0.000000000000000000 ) ) ;
#10432 = CARTESIAN_POINT ( 'NONE',  ( 24.22776226481265383, 49.95013916574269786, 13.94119854578893580 ) ) ;
#10433 = CARTESIAN_POINT ( 'NONE',  ( -10.37757302488623701, 53.52500000273118985, 31.93888565452638417 ) ) ;
#10434 = CARTESIAN_POINT ( 'NONE',  ( -20.75514604977248823, 53.07500000273118701, -28.56700777964554305 ) ) ;
#10435 = CARTESIAN_POINT ( 'NONE',  ( 20.75514604977248467, 40.67500000273117422, -28.56700777964554305 ) ) ;
#10436 = CARTESIAN_POINT ( 'NONE',  ( 10.04305231718579705, 24.60000000000001208, 30.90933677959248982 ) ) ;
#10437 = CARTESIAN_POINT ( 'NONE',  ( -13.97622843553632777, 15.58072916666666430, -24.20753774853731599 ) ) ;
#10438 = CARTESIAN_POINT ( 'NONE',  ( 5.779280353836490358E-15, 15.00000000546237899, 32.49999999999999289 ) ) ;
#10439 = CARTESIAN_POINT ( 'NONE',  ( 8.998893468610761559, 16.99999999999998579, -21.61938333025141290 ) ) ;
#10440 = CARTESIAN_POINT ( 'NONE',  ( -26.29305231718579350, 27.79999999999999005, -19.10302069950537884 ) ) ;
#10441 = CARTESIAN_POINT ( 'NONE',  ( -33.58253175000000113, 17.22500000273118559, 10.91162601494193929 ) ) ;
#10442 = CARTESIAN_POINT ( 'NONE',  ( -11.25946833292375793, 81.17500000273119554, -8.180482586598733619 ) ) ;
#10443 = FACE_OUTER_BOUND ( 'NONE', #430, .T. ) ;
#10444 = CARTESIAN_POINT ( 'NONE',  ( 0.000000000000000000, 80.00000000000001421, 0.000000000000000000 ) ) ;
#10445 = CARTESIAN_POINT ( 'NONE',  ( 26.06988505166722803, 18.58295166574268364, -7.025853678916862854 ) ) ;
#10446 = CARTESIAN_POINT ( 'NONE',  ( -26.29305231718578995, 36.70000000546237828, 19.10302069950538595 ) ) ;
#10447 = CARTESIAN_POINT ( 'NONE',  ( -3.880418787951142701, 11.19874571299079058, 24.49999999999999645 ) ) ;
#10448 = PRODUCT_DEFINITION_SHAPE ( 'NONE', 'NONE',  #6163 ) ;
#10449 = CARTESIAN_POINT ( 'NONE',  ( 33.58253175000000113, 24.22500000273119625, -10.91162601494193574 ) ) ;
#10450 = CARTESIAN_POINT ( 'NONE',  ( 6.988114217767829928, 40.07291666666666430, -26.07999730980489872 ) ) ;
#10451 = ORIENTED_EDGE ( 'NONE', *, *, #20393, .T. ) ;
#10452 = CARTESIAN_POINT ( 'NONE',  ( -20.75514604977248823, 62.82500000273119412, -28.56700777964554305 ) ) ;
#10453 = CARTESIAN_POINT ( 'NONE',  ( 28.01184896238304134, 47.80729166666666430, 7.505752307972846538 ) ) ;
#10454 = ORIENTED_EDGE ( 'NONE', *, *, #9880, .F. ) ;
#10455 = CARTESIAN_POINT ( 'NONE',  ( 26.00068869287367335, 13.57552083333332682, 15.01150461594596308 ) ) ;
#10456 = CARTESIAN_POINT ( 'NONE',  ( -25.98046417659859486, 16.73215250092398065, -15.04653450569291628 ) ) ;
#10457 = VERTEX_POINT ( 'NONE', #29197 ) ;
#10458 = CARTESIAN_POINT ( 'NONE',  ( 33.58253175000000823, 2.025000002731187632, 10.91162601494192863 ) ) ;
#10459 = CARTESIAN_POINT ( 'NONE',  ( 5.779280353836490358E-15, 15.00000000546237899, 32.49999999999999289 ) ) ;
#10460 = CARTESIAN_POINT ( 'NONE',  ( 10.37757302488624056, 34.77500000273120406, -31.93888565452638417 ) ) ;
#10461 = CARTESIAN_POINT ( 'NONE',  ( 32.50000000000000000, 37.60000000546235555, -10.55989012756945833 ) ) ;
#10462 = CARTESIAN_POINT ( 'NONE',  ( -9.270509831248425314, 77.70000000000000284, -12.75976212528059861 ) ) ;
#10463 = CARTESIAN_POINT ( 'NONE',  ( -26.00068869287368756, 66.85677083333334281, -15.01150461594595775 ) ) ;
#10464 = CARTESIAN_POINT ( 'NONE',  ( 10.37757302488624056, 20.52500000273119340, -31.93888565452638417 ) ) ;
#10465 = CARTESIAN_POINT ( 'NONE',  ( 24.50000000000000000, 5.749999994537624559, 0.000000000000000000 ) ) ;
#10466 = CARTESIAN_POINT ( 'NONE',  ( -33.58253175000000113, 47.47500000273119269, 10.91162601494193929 ) ) ;
#10467 = CARTESIAN_POINT ( 'NONE',  ( -26.29305231718579350, 27.80000000000000426, -19.10302069950537884 ) ) ;
#10468 = CARTESIAN_POINT ( 'NONE',  ( 6.277390505771533514E-15, 26.50000000000000711, 34.17252228774368916 ) ) ;
#10469 = CARTESIAN_POINT ( 'NONE',  ( 24.50000000000000355, 3.899999999999992806, 7.960532557706212486 ) ) ;
#10470 = ADVANCED_FACE ( 'NONE', ( #33853 ), #31937, .T. ) ;
#10471 = CARTESIAN_POINT ( 'NONE',  ( -27.16883889988624290, 68.92500000273119554, -19.73931689729374028 ) ) ;
#10472 = CARTESIAN_POINT ( 'NONE',  ( -4.934616302121927505E-14, 71.00000000546238255, 32.50000000000000000 ) ) ;
#10473 = CARTESIAN_POINT ( 'NONE',  ( -26.29305231718578995, 76.70000000546239960, 19.10302069950538595 ) ) ;
#10474 = CARTESIAN_POINT ( 'NONE',  ( -27.16883889988624290, 59.17500000273118133, -19.73931689729374028 ) ) ;
#10475 = CARTESIAN_POINT ( 'NONE',  ( -10.04305231718579172, 40.10000000546237686, -30.90933677959248982 ) ) ;
#10476 = CARTESIAN_POINT ( 'NONE',  ( 20.75514604977248467, 12.42500000273119554, -28.56700777964554305 ) ) ;
#10477 = CARTESIAN_POINT ( 'NONE',  ( 0.04044903254993986036, 34.49256916759064495, -27.95245687107223986 ) ) ;
#10478 = CARTESIAN_POINT ( 'NONE',  ( 17.00271606754840903, 67.00000000000000000, -28.39578712880048528 ) ) ;
#10479 = CARTESIAN_POINT ( 'NONE',  ( 27.16883889988624290, 4.175000002731188431, 19.73931689729373673 ) ) ;
#10480 = CARTESIAN_POINT ( 'NONE',  ( -27.16883889988624290, 36.92500000273117422, -19.73931689729374028 ) ) ;
#10481 = CARTESIAN_POINT ( 'NONE',  ( 20.08610463437157279, 45.80000000546239391, -27.64615127144129758 ) ) ;
#10482 = CARTESIAN_POINT ( 'NONE',  ( 5.779280353836490358E-15, 18.50000000000000000, 32.49999999999999289 ) ) ;
#10483 = CARTESIAN_POINT ( 'NONE',  ( -13.91746824999999887, 78.87500000273118417, 0.000000000000000000 ) ) ;
#10484 = CARTESIAN_POINT ( 'NONE',  ( -20.53372385742107653, 44.93711833240935505, -20.47846945139867003 ) ) ;
#10485 = CARTESIAN_POINT ( 'NONE',  ( 32.50000000000000711, 55.40000000546238113, 10.55989012756945122 ) ) ;
#10486 = CARTESIAN_POINT ( 'NONE',  ( 4.300734207923757602, 74.77500000273118985, -13.23629886949340673 ) ) ;
#10487 = SURFACE_SIDE_STYLE ('',( #5678 ) ) ;
#10488 = CARTESIAN_POINT ( 'NONE',  ( 2.584737979205441561E-13, 21.02343749999999645, 27.95245687107222921 ) ) ;
#10489 = CARTESIAN_POINT ( 'NONE',  ( 20.08610463437157279, 63.80000000546237970, -27.64615127144129758 ) ) ;
#10490 = CARTESIAN_POINT ( 'NONE',  ( 26.29305231718579350, 67.30000000546237970, 19.10302069950537529 ) ) ;
#10491 = CARTESIAN_POINT ( 'NONE',  ( -20.50609665441004736, 18.87499999999999645, -20.50609665440969565 ) ) ;
#10492 = CARTESIAN_POINT ( 'NONE',  ( 10.37757302488624767, 31.97500000273119269, 31.93888565452638417 ) ) ;
#10493 = CARTESIAN_POINT ( 'NONE',  ( -4.523095164977117273E-15, 12.62499999726879807, 24.62258325217400312 ) ) ;
#10494 = VERTEX_POINT ( 'NONE', #8262 ) ;
#10495 = CARTESIAN_POINT ( 'NONE',  ( -28.00173670424549499, 44.08892333425729504, -7.543491769121417612 ) ) ;
#10496 = CARTESIAN_POINT ( 'NONE',  ( -10.04305231718578462, 22.90000000546237047, 30.90933677959249337 ) ) ;
#10497 = CARTESIAN_POINT ( 'NONE',  ( 15.01150461594596308, 47.09114583333332860, -26.00068869287367335 ) ) ;
#10498 = CARTESIAN_POINT ( 'NONE',  ( -1.778240108872766143E-15, 35.49999999999998579, -32.49999999999999289 ) ) ;
#10499 = CARTESIAN_POINT ( 'NONE',  ( -10.37757302488623701, 53.77500000273119696, 31.93888565452638417 ) ) ;
#10500 = CARTESIAN_POINT ( 'NONE',  ( -2.092463501923844636E-15, 54.00000000546236834, -34.17252228774368916 ) ) ;
#10501 = CARTESIAN_POINT ( 'NONE',  ( 24.50000000000000000, 5.649999994537638237, 7.960532557706212486 ) ) ;
#10502 = CARTESIAN_POINT ( 'NONE',  ( 33.58253175000000113, 40.22500000273119269, -10.91162601494193751 ) ) ;
#10503 = CARTESIAN_POINT ( 'NONE',  ( 0.000000000000000000, -22.99999999999999289, 0.000000000000000000 ) ) ;
#10504 = VECTOR ( 'NONE', #1829, 1000.000000000000000 ) ;
#10505 = CARTESIAN_POINT ( 'NONE',  ( -33.58253175000000113, 71.47500000273119269, 10.91162601494193929 ) ) ;
#10506 = CARTESIAN_POINT ( 'NONE',  ( 12.07957071404696592, 74.00000000000001421, 6.971801377361973806 ) ) ;
#10507 = CARTESIAN_POINT ( 'NONE',  ( -10.37757302488624411, 62.72500000273119269, -31.93888565452638417 ) ) ;
#10508 = CARTESIAN_POINT ( 'NONE',  ( 2.740863092043355209E-13, 24.46093749999999645, 30.02300923189239867 ) ) ;
#10509 = CARTESIAN_POINT ( 'NONE',  ( -26.29305231718578995, 44.20000000000001705, 19.10302069950538595 ) ) ;
#10510 = CARTESIAN_POINT ( 'NONE',  ( 23.41746825000000243, 6.524999997268818852, 7.608796670333735079 ) ) ;
#10511 = EDGE_CURVE ( 'NONE', #26665, #29691, #2973, .T. ) ;
#10512 = CARTESIAN_POINT ( 'NONE',  ( 10.37757302488624056, 12.77500000273118452, -31.93888565452638417 ) ) ;
#10513 = CARTESIAN_POINT ( 'NONE',  ( 1.093617666956751375E-13, 66.00000000546238255, -32.50000000000000711 ) ) ;
#10514 = CARTESIAN_POINT ( 'NONE',  ( 27.95245687107223276, 32.47618083240936215, -0.04044903255042905932 ) ) ;
#10515 = LINE ( 'NONE', #28866, #5104 ) ;
#10516 = CARTESIAN_POINT ( 'NONE',  ( 2.489536152421872915E-14, 77.50000000000000000, -32.49999999999999289 ) ) ;
#10517 = CARTESIAN_POINT ( 'NONE',  ( 0.000000000000000000, 80.00000000000001421, 0.000000000000000000 ) ) ;
#10518 = EDGE_CURVE ( 'NONE', #19648, #1729, #21419, .T. ) ;
#10519 = CARTESIAN_POINT ( 'NONE',  ( 6.486482029760649416E-15, 75.87500000273119838, 35.31076352940723240 ) ) ;
#10520 = ORIENTED_EDGE ( 'NONE', *, *, #30533, .T. ) ;
#10521 = CARTESIAN_POINT ( 'NONE',  ( 14.47279130897151589, 16.82499999726881512, 19.92008829642072953 ) ) ;
#10522 = CARTESIAN_POINT ( 'NONE',  ( -27.95245687107222921, 59.69531250000000711, 2.498001805406602216E-13 ) ) ;
#10523 = CARTESIAN_POINT ( 'NONE',  ( 10.37757302488624767, 55.72500000273118559, 31.93888565452638417 ) ) ;
#10524 = CARTESIAN_POINT ( 'NONE',  ( 33.58253175000000823, 14.27500000273119340, 10.91162601494192863 ) ) ;
#10525 = CARTESIAN_POINT ( 'NONE',  ( -33.58253175000000113, 3.475000002731185589, 10.91162601494193929 ) ) ;
#10526 = CARTESIAN_POINT ( 'NONE',  ( -6.988114217768288228, 36.34895833333333570, -26.07999730980477437 ) ) ;
#10527 = CARTESIAN_POINT ( 'NONE',  ( 20.53372385742072481, 28.04725666759063429, -20.47846945139902175 ) ) ;
#10528 = CARTESIAN_POINT ( 'NONE',  ( -25.98046417659831420, 20.15847249907602290, 15.04653450569339945 ) ) ;
#10529 = CARTESIAN_POINT ( 'NONE',  ( 26.29305231718579350, 71.30000000546236549, 19.10302069950537529 ) ) ;
#10530 = CARTESIAN_POINT ( 'NONE',  ( 16.81447360525979917, 52.00000000000001421, -28.18961368868568229 ) ) ;
#10531 = CARTESIAN_POINT ( 'NONE',  ( -10.37757302488624411, 38.72500000273118559, -31.93888565452638417 ) ) ;
#10532 = CARTESIAN_POINT ( 'NONE',  ( 6.950374756619257965, 48.94753499907601935, -26.09010956794244507 ) ) ;
#10533 = CARTESIAN_POINT ( 'NONE',  ( 7.236395654485760609, 9.024999997268828622, -22.27133577429736633 ) ) ;
#10534 = CARTESIAN_POINT ( 'NONE',  ( 2.445080149700053643E-15, 74.75000000546236834, 15.00000000000000000 ) ) ;
#10535 = ORIENTED_EDGE ( 'NONE', *, *, #21696, .F. ) ;
#10536 = CARTESIAN_POINT ( 'NONE',  ( -33.58253175000000113, 55.27500000273120406, -10.91162601494193218 ) ) ;
#10537 = CARTESIAN_POINT ( 'NONE',  ( 23.41746824999999887, 0.8749999972688105032, 0.000000000000000000 ) ) ;
#10538 = CARTESIAN_POINT ( 'NONE',  ( -14.01125832528285109, 39.93527750092397355, 24.18731323226248264 ) ) ;
#10539 = CARTESIAN_POINT ( 'NONE',  ( -33.58253175000000113, 77.47500000273120691, 10.91162601494193929 ) ) ;
#10540 = VERTEX_POINT ( 'NONE', #2787 ) ;
#10541 = CARTESIAN_POINT ( 'NONE',  ( 33.58253175000000113, 22.22500000273117493, -10.91162601494193751 ) ) ;
#10542 = CARTESIAN_POINT ( 'NONE',  ( 20.50609665440969565, 19.73437500000000000, -20.50609665441004736 ) ) ;
#10543 = ORIENTED_EDGE ( 'NONE', *, *, #5807, .F. ) ;
#10544 = CARTESIAN_POINT ( 'NONE',  ( 10.04305231718578817, 29.90000000546239178, -30.90933677959249337 ) ) ;
#10545 = CARTESIAN_POINT ( 'NONE',  ( -20.75514604977248823, 58.82500000273117990, -28.56700777964554305 ) ) ;
#10546 = CARTESIAN_POINT ( 'NONE',  ( 26.00068869287367335, 47.95052083333331439, 15.01150461594596308 ) ) ;
#10547 = CARTESIAN_POINT ( 'NONE',  ( -18.94512977948576093, 10.32499999726882400, 13.76444248337722698 ) ) ;
#10548 = CARTESIAN_POINT ( 'NONE',  ( 20.75514604977248467, 4.425000002731183990, -28.56700777964554305 ) ) ;
#10549 = CARTESIAN_POINT ( 'NONE',  ( 5.779280353836490358E-15, 59.00000000546238255, 32.49999999999999289 ) ) ;
#10550 = CARTESIAN_POINT ( 'NONE',  ( 0.04044903255045854962, 64.27305583240934084, 30.02300923189239867 ) ) ;
#10551 = CARTESIAN_POINT ( 'NONE',  ( -15.00000000000000000, 80.15000000546234560, -4.873795443493594171 ) ) ;
#10552 = CARTESIAN_POINT ( 'NONE',  ( 5.147494310547481966, 65.94874572391553613, -32.49999999999998579 ) ) ;
#10553 = CARTESIAN_POINT ( 'NONE',  ( 20.08610463437158344, 8.699999999999986855, 27.64615127144129403 ) ) ;
#10554 = CARTESIAN_POINT ( 'NONE',  ( 32.50000000000000711, 16.89999999999998437, 10.55989012756945122 ) ) ;
#10555 = CARTESIAN_POINT ( 'NONE',  ( -13.97622843553588901, 62.55989583333332149, 24.20753774853756823 ) ) ;
#10556 = EDGE_CURVE ( 'NONE', #32671, #29627, #20991, .T. ) ;
#10557 = EDGE_CURVE ( 'NONE', #11416, #11025, #7932, .T. ) ;
#10558 = CARTESIAN_POINT ( 'NONE',  ( -14.47279130897152122, 2.424999997268802332, 19.92008829642072243 ) ) ;
#10559 = CARTESIAN_POINT ( 'NONE',  ( -4.635254915624211769, 73.85000000546237686, -14.26584774442730286 ) ) ;
#10560 = CARTESIAN_POINT ( 'NONE',  ( 2.584737979205441561E-13, 34.77343750000000000, 27.95245687107222921 ) ) ;
#10561 = CARTESIAN_POINT ( 'NONE',  ( -2.162160676586881955E-15, 28.62500000273118062, -35.31076352940723240 ) ) ;
#10562 = CARTESIAN_POINT ( 'NONE',  ( -33.58253175000000113, 71.22500000273117848, 10.91162601494193929 ) ) ;
#10563 = CARTESIAN_POINT ( 'NONE',  ( -20.75514604977248112, 39.67500000273118133, 28.56700777964554661 ) ) ;
#10564 = CARTESIAN_POINT ( 'NONE',  ( 33.58253175000000113, 16.47500000273118204, -10.91162601494193574 ) ) ;
#10565 = CARTESIAN_POINT ( 'NONE',  ( -1.053607264507113999E-13, 64.50000000000000000, 32.50000000000000711 ) ) ;
#10567 = CARTESIAN_POINT ( 'NONE',  ( 6.950374756619721595, 56.69309000092396644, 26.09010956794232428 ) ) ;
#10566 =( REPRESENTATION_RELATIONSHIP ('NONE','NONE', #5873, #10290 ) REPRESENTATION_RELATIONSHIP_WITH_TRANSFORMATION ( #23981 )SHAPE_REPRESENTATION_RELATIONSHIP( ) );
#10568 = CARTESIAN_POINT ( 'NONE',  ( -10.37757302488624411, 74.72500000273119269, -31.93888565452638417 ) ) ;
#10569 = CARTESIAN_POINT ( 'NONE',  ( 24.50000000000000000, 8.100000000000006750, -7.960532557706203605 ) ) ;
#10570 = CARTESIAN_POINT ( 'NONE',  ( 26.29305231718579350, 54.80000000000000426, 19.10302069950537529 ) ) ;
#10571 = CARTESIAN_POINT ( 'NONE',  ( -18.94512977948575738, 17.42499999726882010, -13.76444248337723231 ) ) ;
#10572 = CARTESIAN_POINT ( 'NONE',  ( 10.37757302488624056, 56.52500000273119696, -31.93888565452638417 ) ) ;
#10573 = CIRCLE ( 'NONE', #33001, 2.000000000000000000 ) ;
#10574 = CARTESIAN_POINT ( 'NONE',  ( -18.94512977948576093, 6.324999997268820451, 13.76444248337722698 ) ) ;
#10575 = ORIENTED_EDGE ( 'NONE', *, *, #12841, .F. ) ;
#10576 = CARTESIAN_POINT ( 'NONE',  ( 33.58253175000000113, 74.47500000273116427, -10.91162601494193751 ) ) ;
#10577 = CARTESIAN_POINT ( 'NONE',  ( 33.58253175000000113, 8.125000002731198379, -4.112674001490185761E-15 ) ) ;
#10578 = CARTESIAN_POINT ( 'NONE',  ( 7.236395654485760609, 15.52499999726880731, -22.27133577429736633 ) ) ;
#10579 = CARTESIAN_POINT ( 'NONE',  ( -19.11951029504763611, 16.01600666759064140, 19.06425588902592239 ) ) ;
#10580 = VERTEX_POINT ( 'NONE', #15841 ) ;
#10581 = CARTESIAN_POINT ( 'NONE',  ( 20.75514604977248467, 46.42500000273119554, -28.56700777964554305 ) ) ;
#10582 =( BOUNDED_CURVE ( )  B_SPLINE_CURVE ( 2, ( #26378, #13162, #10257, #5441, #10763, #28943, #2530, #26208, #33931, #26036, #10084, #28269, #12998 ),
 .UNSPECIFIED., .F., .T. ) 
 B_SPLINE_CURVE_WITH_KNOTS ( ( 3, 2, 2, 2, 2, 2, 3 ),
 ( 0.6346153846153845812, 0.6358974358974358587, 0.6384615384615384137, 0.6410256410256410797, 0.6435897435897436347, 0.6461538461538461897, 0.6474358974358974672 ),
 .UNSPECIFIED. ) 
 CURVE ( )  GEOMETRIC_REPRESENTATION_ITEM ( )  RATIONAL_B_SPLINE_CURVE ( ( 0.9755282581475768211, 0.9755282581475768211, 1.000000000000000000, 0.9510565162951535312, 1.000000000000000000, 0.9510565162951535312, 1.000000000000000000, 0.9510565162951535312, 1.000000000000000000, 0.9510565162951535312, 1.000000000000000000, 0.9755282581475768211, 0.9755282581475768211 ) ) 
 REPRESENTATION_ITEM ( '' )  );
#10583 = ORIENTED_EDGE ( 'NONE', *, *, #25296, .T. ) ;
#10584 = CARTESIAN_POINT ( 'NONE',  ( 26.00068869287367335, 41.07552083333331439, 15.01150461594596308 ) ) ;
#10585 = CARTESIAN_POINT ( 'NONE',  ( 5.147494310547434893, 4.551254281546843750, 32.49999999999999289 ) ) ;
#10586 = CARTESIAN_POINT ( 'NONE',  ( 32.50000000000000000, 1.500000005462381880, -3.980102097228898626E-15 ) ) ;
#10587 = CARTESIAN_POINT ( 'NONE',  ( 26.29305231718578995, 27.70000000546238184, -19.10302069950538240 ) ) ;
#10588 = CARTESIAN_POINT ( 'NONE',  ( -15.01150461594595775, 17.87239583333332149, 26.00068869287368756 ) ) ;
#10589 = CARTESIAN_POINT ( 'NONE',  ( 24.50000000000000000, 0.000000000000000000, 0.000000000000000000 ) ) ;
#10590 = CARTESIAN_POINT ( 'NONE',  ( 6.486482029760649416E-15, 17.87500000273119838, 35.31076352940723240 ) ) ;
#10591 = AXIS2_PLACEMENT_3D ( 'NONE', #18177, #4775, #17656 ) ;
#10592 = CARTESIAN_POINT ( 'NONE',  ( 20.08610463437157279, 61.30000000000001847, -27.64615127144129758 ) ) ;
#10593 = CARTESIAN_POINT ( 'NONE',  ( 20.08610463437158344, 57.20000000546237828, 27.64615127144129403 ) ) ;
#10594 = CARTESIAN_POINT ( 'NONE',  ( 32.50000000000000000, 73.60000000546239107, -10.55989012756945833 ) ) ;
#10595 = CARTESIAN_POINT ( 'NONE',  ( -20.53372385742107653, 34.62461833240934794, -20.47846945139867003 ) ) ;
#10596 = CARTESIAN_POINT ( 'NONE',  ( 11.25946833292375793, 76.57500000273120122, -8.180482586598735395 ) ) ;
#10597 = CARTESIAN_POINT ( 'NONE',  ( -15.01150461594642316, 39.64322916666667140, -26.00068869287341045 ) ) ;
#10598 = CYLINDRICAL_SURFACE ( 'NONE', #7510, 15.00000000000000000 ) ;
#10599 = CARTESIAN_POINT ( 'NONE',  ( -24.50000000000000000, 13.00000000000001066, -3.000384657911015469E-15 ) ) ;
#10600 = CARTESIAN_POINT ( 'NONE',  ( 10.04305231718579705, 4.599999999999992539, 30.90933677959248982 ) ) ;
#10601 = CARTESIAN_POINT ( 'NONE',  ( -24.49999999999999645, -17.00000000000000000, 0.000000000000000000 ) ) ;
#10602 = CARTESIAN_POINT ( 'NONE',  ( -26.09010956794245217, 65.27565999907601224, -6.950374756619243755 ) ) ;
#10603 = CARTESIAN_POINT ( 'NONE',  ( 27.16883889988624290, 51.92500000273120264, 19.73931689729373673 ) ) ;
#10604 = CARTESIAN_POINT ( 'NONE',  ( 2.897257156509938333E-15, 70.75000000546238255, 15.77193336357400710 ) ) ;
#10605 = CARTESIAN_POINT ( 'NONE',  ( 20.75514604977249178, 56.07500000273117990, 28.56700777964553950 ) ) ;
#10606 = CARTESIAN_POINT ( 'NONE',  ( 20.75514604977248467, 32.67500000273119554, -28.56700777964554305 ) ) ;
#10607 = DIRECTION ( 'NONE',  ( -1.224646799147353454E-16, 1.000000000000000000, -0.000000000000000000 ) ) ;
#10608 = LINE ( 'NONE', #22966, #8447 ) ;
#10609 = DIRECTION ( 'NONE',  ( 0.000000000000000000, 0.000000000000000000, 1.000000000000000000 ) ) ;
#10610 = CARTESIAN_POINT ( 'NONE',  ( -20.08610463437156923, 22.80000000546236549, 27.64615127144130113 ) ) ;
#10611 = CARTESIAN_POINT ( 'NONE',  ( -32.50000000000000000, 70.10000000000000853, 10.55989012756946366 ) ) ;
#10612 = CARTESIAN_POINT ( 'NONE',  ( 33.58253175000000113, 14.22500000273119625, -10.91162601494193751 ) ) ;
#10613 = DIRECTION ( 'NONE',  ( 0.000000000000000000, 0.000000000000000000, 1.000000000000000000 ) ) ;
#10614 = DIRECTION ( 'NONE',  ( -1.224646799147353454E-16, 1.000000000000000000, -0.000000000000000000 ) ) ;
#10615 = CARTESIAN_POINT ( 'NONE',  ( 19.82091636218621389, 9.949999994537634507, -14.40073868116559197 ) ) ;
#10616 = CARTESIAN_POINT ( 'NONE',  ( 7.025853678916867295, 22.87982666574268720, 26.06988505166722803 ) ) ;
#10617 = CARTESIAN_POINT ( 'NONE',  ( -20.08610463437157989, 38.20000000546236407, -27.64615127144129758 ) ) ;
#10618 = CARTESIAN_POINT ( 'NONE',  ( 32.50000000000000711, 10.90000000000000568, 10.55989012756945122 ) ) ;
#10619 = CARTESIAN_POINT ( 'NONE',  ( -33.58253175000000113, 23.22500000273117493, 10.91162601494193929 ) ) ;
#10620 = CARTESIAN_POINT ( 'NONE',  ( -24.20753774853756823, 46.23177083333331439, -13.97622843553588723 ) ) ;
#10621 = AXIS2_PLACEMENT_3D ( 'NONE', #6337, #31906, #16815 ) ;
#10622 = ADVANCED_FACE ( 'NONE', ( #13253 ), #193, .T. ) ;
#10623 = ORIENTED_EDGE ( 'NONE', *, *, #14259, .T. ) ;
#10624 = CARTESIAN_POINT ( 'NONE',  ( 20.75514604977248467, 64.42500000273116711, -28.56700777964554305 ) ) ;
#10625 = EDGE_LOOP ( 'NONE', ( #24914, #32419, #20889, #18532 ) ) ;
#10626 = CARTESIAN_POINT ( 'NONE',  ( -20.53372385742071771, 64.14100666759063074, 20.47846945139902530 ) ) ;
#10627 = CARTESIAN_POINT ( 'NONE',  ( 28.00173670424549499, 14.87017333425730747, 7.543491769121417612 ) ) ;
#10628 = CARTESIAN_POINT ( 'NONE',  ( -33.58253175000000113, 3.125000002731193049, 0.000000000000000000 ) ) ;
#10629 = CARTESIAN_POINT ( 'NONE',  ( -23.41746824999999887, 1.624999997268811169, -2.867812753649727150E-15 ) ) ;
#10630 = CARTESIAN_POINT ( 'NONE',  ( -27.16883889988623935, 37.57500000273117280, 19.73931689729374739 ) ) ;
#10631 = CARTESIAN_POINT ( 'NONE',  ( 26.29305231718578995, 35.70000000546236407, -19.10302069950538240 ) ) ;
#10632 = CARTESIAN_POINT ( 'NONE',  ( 20.08610463437157279, 79.30000000000001137, -27.64615127144129758 ) ) ;
#10633 = CARTESIAN_POINT ( 'NONE',  ( -7.505752307972844761, 65.85416666666665719, 28.01184896238304134 ) ) ;
#10634 = CARTESIAN_POINT ( 'NONE',  ( 0.000000000000000000, 0.000000000000000000, 24.50000000000000000 ) ) ;
#10635 = CARTESIAN_POINT ( 'NONE',  ( 10.37757302488624767, 51.97500000273119980, 31.93888565452638417 ) ) ;
#10636 = CARTESIAN_POINT ( 'NONE',  ( -10.04305231718578462, 20.40000000000001634, 30.90933677959249337 ) ) ;
#10637 = CARTESIAN_POINT ( 'NONE',  ( -32.50000000000000000, 24.09999999999999787, 10.55989012756946366 ) ) ;
#10638 = CARTESIAN_POINT ( 'NONE',  ( 1.577395562988744260E-15, 8.499999999999992895, -25.76082449383753925 ) ) ;
#10639 = CARTESIAN_POINT ( 'NONE',  ( 33.58253175000000113, 68.12500000273119838, -4.112674001490185761E-15 ) ) ;
#10640 = CARTESIAN_POINT ( 'NONE',  ( -7.570916362186210335, 2.349999994537638415, -23.30088464923126779 ) ) ;
#10641 = AXIS2_PLACEMENT_3D ( 'NONE', #9500, #20326, #25471 ) ;
#10642 = CARTESIAN_POINT ( 'NONE',  ( 12.86449124955741041, 74.00000000000001421, -5.310441354522136947 ) ) ;
#10643 = CARTESIAN_POINT ( 'NONE',  ( 20.75514604977248467, 56.67500000273119554, -28.56700777964554305 ) ) ;
#10644 = CONICAL_SURFACE ( 'NONE', #22685, 24.49999999999999645, 1.047197551196593412 ) ;
#10645 = CARTESIAN_POINT ( 'NONE',  ( 20.08610463437157279, 7.800000005462373487, -27.64615127144129758 ) ) ;
#10646 = CARTESIAN_POINT ( 'NONE',  ( -10.37757302488624411, 14.72500000273119269, -31.93888565452638417 ) ) ;
#10647 = CARTESIAN_POINT ( 'NONE',  ( 26.09010956794232428, 31.77121500092397000, -6.950374756619718042 ) ) ;
#10648 = CARTESIAN_POINT ( 'NONE',  ( 1.683996601885203503, 67.00000000000000000, -33.30202823065786788 ) ) ;
#10649 = CARTESIAN_POINT ( 'NONE',  ( 10.37757302488624056, 2.775000002731176085, -31.93888565452638417 ) ) ;
#10650 = CARTESIAN_POINT ( 'NONE',  ( -2.162160676586881955E-15, 32.62500000273119838, -35.31076352940723240 ) ) ;
#10651 = CARTESIAN_POINT ( 'NONE',  ( -20.08610463437156923, 64.80000000546237970, 27.64615127144130113 ) ) ;
#10652 = DIRECTION ( 'NONE',  ( -0.000000000000000000, -1.000000000000000000, -0.000000000000000000 ) ) ;
#10653 = CARTESIAN_POINT ( 'NONE',  ( 2.688165632520823219E-15, 79.37500000273118417, 14.63369212191046209 ) ) ;
#10654 = CARTESIAN_POINT ( 'NONE',  ( -25.98046417659831420, 44.22097249907603356, 15.04653450569339945 ) ) ;
#10655 = CARTESIAN_POINT ( 'NONE',  ( -20.08610463437156923, 52.80000000546237260, 27.64615127144130113 ) ) ;
#10656 = CARTESIAN_POINT ( 'NONE',  ( -4.300734207923755825, 77.77500000273118985, 13.23629886949340673 ) ) ;
#10657 = PRESENTATION_STYLE_ASSIGNMENT (( #10323 ) ) ;
#10658 = CARTESIAN_POINT ( 'NONE',  ( 13.97622843553633665, 17.29947916666666430, 24.20753774853730889 ) ) ;
#10659 = CARTESIAN_POINT ( 'NONE',  ( 23.41746825000000243, 3.224999997268806151, -7.608796670333727974 ) ) ;
#10660 = CARTESIAN_POINT ( 'NONE',  ( -20.08610463437157989, 68.20000000546239960, -27.64615127144129758 ) ) ;
#10661 = CARTESIAN_POINT ( 'NONE',  ( 15.01150461594643204, 20.73697916666666075, 26.00068869287340334 ) ) ;
#10662 = CARTESIAN_POINT ( 'NONE',  ( 6.486482029760649416E-15, 29.87500000273119838, 35.31076352940723240 ) ) ;
#10663 = CARTESIAN_POINT ( 'NONE',  ( -7.236395654485763274, 14.52499999726880553, 22.27133577429736633 ) ) ;
#10664 = ORIENTED_EDGE ( 'NONE', *, *, #5900, .T. ) ;
#10665 = CARTESIAN_POINT ( 'NONE',  ( 15.04653450569292872, 45.09152750092398065, -25.98046417659857710 ) ) ;
#10666 = CARTESIAN_POINT ( 'NONE',  ( -32.50000000000000000, 14.40000000546236691, -10.55989012756945478 ) ) ;
#10667 = CARTESIAN_POINT ( 'NONE',  ( 26.00068869287367335, 54.82552083333331439, 15.01150461594596308 ) ) ;
#10668 = CARTESIAN_POINT ( 'NONE',  ( 2.489536152421872915E-14, 75.50000000000001421, -32.49999999999999289 ) ) ;
#10669 = CARTESIAN_POINT ( 'NONE',  ( -27.16883889988624290, 53.17500000273117422, -19.73931689729374028 ) ) ;
#10670 = CARTESIAN_POINT ( 'NONE',  ( 26.29305231718578995, 59.70000000546238539, -19.10302069950538240 ) ) ;
#10671 = CARTESIAN_POINT ( 'NONE',  ( -8.960552108402742093E-16, 76.87500000273118417, -14.63369212191046387 ) ) ;
#10672 = CARTESIAN_POINT ( 'NONE',  ( -27.16883889988624290, 40.92500000273119554, -19.73931689729374028 ) ) ;
#10673 = CARTESIAN_POINT ( 'NONE',  ( -33.58253175000000113, 67.37500000273119838, 0.000000000000000000 ) ) ;
#10674 = CARTESIAN_POINT ( 'NONE',  ( 6.189173980287828059, 74.00000000000002842, 12.49879098907252128 ) ) ;
#10675 = CARTESIAN_POINT ( 'NONE',  ( 20.75514604977248467, 60.42500000273118133, -28.56700777964554305 ) ) ;
#10676 = CARTESIAN_POINT ( 'NONE',  ( -20.50609665440969209, 21.45312499999999645, 20.50609665441005092 ) ) ;
#10677 = CARTESIAN_POINT ( 'NONE',  ( 26.29305231718579350, 44.80000000000000426, 19.10302069950537529 ) ) ;
#10678 = CARTESIAN_POINT ( 'NONE',  ( 18.94512977948575738, 6.424999997268809437, 13.76444248337723408 ) ) ;
#10679 = CARTESIAN_POINT ( 'NONE',  ( 10.37757302488624767, 7.975000002731186477, 31.93888565452638417 ) ) ;
#10680 = CARTESIAN_POINT ( 'NONE',  ( 0.000000000000000000, 80.00000000000001421, 0.000000000000000000 ) ) ;
#10681 = CARTESIAN_POINT ( 'NONE',  ( 0.04044903255044120238, 36.77305583240936215, 27.95245687107223276 ) ) ;
#10682 = CARTESIAN_POINT ( 'NONE',  ( 4.300734207923761154, 73.97500000273119269, 13.23629886949340495 ) ) ;
#10683 = CARTESIAN_POINT ( 'NONE',  ( 12.11000150615022264, -45.00000000000001421, 0.000000000000000000 ) ) ;
#10684 = CARTESIAN_POINT ( 'NONE',  ( -33.58253175000000113, 77.37500000273118417, 0.000000000000000000 ) ) ;
#10685 = ORIENTED_EDGE ( 'NONE', *, *, #23142, .T. ) ;
#10686 = CYLINDRICAL_SURFACE ( 'NONE', #14582, 32.50000000000000000 ) ;
#10687 = AXIS2_PLACEMENT_3D ( 'NONE', #25885, #15779, #301 ) ;
#10688 = CARTESIAN_POINT ( 'NONE',  ( -6.988114217767819270, 58.97916666666666430, 26.07999730980490583 ) ) ;
#10689 =( BOUNDED_SURFACE ( )  B_SPLINE_SURFACE ( 1, 2, ( 
 ( #25509, #20196, #17617, #22934, #25333, #1297, #14701, #24990, #19681, #28078, #17452, #30468, #1811, #25159, #27912, #7307, #20366, #30127, #30814, #27568, #4395, #4567, #1473, #27401, #14869, #1989, #17109, #11779, #9889, #15567, #4909, #7996, #20544, #7824, #28584, #18313, #26360, #5254, #5424, #2335, #2158, #10404, #30989, #7654, #23453, #23793, #2849, #15215, #15904, #10576, #21054, #13320, #15736, #25678, #31162, #15389, #10064, #13146, #31332, #2511, #26191, #26020, #33915, #31667, #10745, #12632, #21224, #17969, #10241, #7489, #28419, #28759, #2686, #23619, #88, #31504, #20883, #25845, #33745, #4734, #12979, #23280, #18481, #28925, #18141, #12808, #259, #20721, #17792, #23102, #5081, #28251, #33566, #3519, #3356, #593, #6258, #31832, #767, #29753, #13826, #1089, #13991, #3194, #24452, #18815, #27024, #16075, #16241, #24295, #11408, #8663, #5593, #928, #21724, #16737, #29258, #24127, #21884, #32334, #431, #11248, #11571, #16407, #8827, #18651, #13494, #6087, #26697, #29089, #19147, #10915, #26530, #26861, #3024, #29585, #3685, #11084, #32170, #23961, #27195, #18982, #19311, #13663, #21387, #21556, #31999, #8495, #5762, #16569, #14159, #29427, #24615, #8326, #22052, #5930, #8161, #27528, #29927, #4017, #17069, #14491, #9160, #33175, #30086, #32498, #24949, #32830, #27364, #8997, #6592, #30255, #19644, #22726, #1258, #22545, #9320, #32994, #7099, #19983, #20159, #1431, #16902, #25121, #11738, #22381, #4189, #4529, #17582, #6430, #30603, #25299, #1768, #28043, #30430, #3849, #11909, #19807, #24779, #27874, #12076, #17239, #6929, #6759, #14661, #12426, #25473, #14324, #1951, #32665, #27699, #22218, #1599, #9502, #17412, #4357, #14833, #12249, #9677, #15004, #19478, #9851, #7618, #28384, #31291, #28719, #2299, #30952, #18098, #25644, #13109, #17754, #23067, #31125, #31464, #18272, #28545, #15354, #21013, #12597, #15527, #10536, #5043, #15864, #5215, #17934, #15698, #33527, #7785, #30778, #7449, #25980, #26152, #23414, #20328, #2646, #2473, #7956, #10030, #4873, #23583, #48, #15179, #12940, #26320, #33875, #18443, #33354, #28212, #20846, #25808, #7270, #10368, #2122, #4699, #28886, #20506, #12771, #23245, #5386, #33706, #2809, #22896, #10205, #20685, #31960, #16034, #3478, #8124, #13452, #21511, #21846, #8623, #8455, #5725, #11370, #2984, #5889, #889, #18944, #6214, #19105, #8283, #29544, #23920, #32127, #21184, #21351, #29389, #16526, #13783, #10704, #6045, #26821, #32291, #391, #29219, #26979, #13949, #5553, #16367, #16694, #3317, #24412, #23751, #18612, #11208, #31793, #217, #24252, #26489, #31626, #722, #29050, #21681, #8785, #16203, #19268, #10876, #29710, #24089, #27151, #18775, #26657, #3153, #13624, #557, #11045, #13276, #1216, #3644, #9121, #3978, #32456, #14119, #11696, #1394, #24740, #27830, #6386, #27658, #14451, #4147, #12207, #25076, #25252, #22180, #22010, #30217, #16863, #27488, #9283, #9633, #22678, #1048, #1727, #30385, #6887, #33129, #1557, #11528, #17029, #32625, #29885, #32954, #17200, #22343, #12033, #11867, #19767, #17539, #30560, #8957, #7056, #3812, #30050, #27324, #14283, #14620, #22503, #9456, #19938, #17367, #6718, #19603, #32790, #6554, #20116, #24908, #4313, #24576, #14788, #19437, #23371, #23027, #10329, #4658, #12896, #1906, #2081, #10156, #31249, #28501, #25428, #33832, #7576, #15656, #15138, #9984, #20805, #7741, #20286, #20638, #20969, #2252, #18230, #4486, #33310, #25935, #12556, #14962, #4998, #30733, #12383, #12726, #22852, #15481, #23541, #20458, #23196, #9809, #13065, #4827, #28676, #33484, #7226, #30909, #7403, #17889, #25602, #5172, #28342, #27999, #15307, #25766, #17712, #28170, #33658, #31081, #18056, #26106, #2428, #2604, #2, #10492, #31420, #7913, #6477, #2938, #2767, #11454, #31582, #8242, #24498, #24825, #27407, #15823, #16949, #11617, #22099, #3897, #16780, #26277, #31751, #5510, #10662, #14204, #32378, #3563, #27240, #16160, #971, #32707, #11785, #13232, #22265, #18569, #10831, #8082, #29010, #29802, #19358, #8874, #3733, #6304, #21928, #15991, #347, #5342, #14036, #23877, #24660, #1132, #18735, #26447, #32544, #21141, #9043, #23706, #13409, #26614, #14368, #19522, #21310, #172, #29970, #29177, #1304, #18397, #5682, #28843, #9548, #24996, #17623, #27574, #22422, #33044, #25516, #33220, #20028, #4233, #1995, #11953, #6973, #4573, #30474, #33396, #9719, #6803, #20202, #32871, #22767, #6636, #19850, #17458, #30645, #14875, #30133, #7142, #27918, #15051, #9368, #27743, #28084, #12470, #1479, #4401, #9895, #25340, #22940, #19687, #4063, #1817, #30304, #17116, #12295, #14535, #9202, #20372, #1643, #17282, #14707, #25165, #12119, #22591, #24936, #16726, #6582, #917, #3345, #11396, #24440, #21873, #16557, #17057, #3507, #5918, #32323, #6246, #751, #16395, #13977, #3674, #27010, #30076, #8650, #29916, #27181, #6418, #14480, #27353, #27519, #8814, #24282, #32484, #19135, #29741, #11558, #11899, #1421, #13815, #4006, #32654, #9149, #22371, #3838, #11235, #19297, #14148, #32157, #1246, #19467, #24604, #14313, #1078, #22040, #19795, #32818, #21711, #9310, #6073, #8986, #29572, #16890, #24768, #11725, #22207, #19631, #26848, #1936, #27863, #22884, #9666, #25633, #25461, #4516, #6917, #15167, #33514, #2112, #20147, #10019, #12585, #14991, #14652, #12414, #25285, #30941, #1588, #2285, #32985, #12064, #1757, #9489, #33341, #17922, #9838, #30591, #4861, #4688, #12237, #4345, #12760, #20316, #23055, #30765, #28029, #7255, #22713, #7436, #25112, #14820, #33163, #23232, #7087, #33692, #17742, #17571, #25796, #28202, #19972, #20490, #30418, #17399, #22535, #28373, #15341, #10191, #30243, #6748, #17228, #27688, #4178, #15516, #18764, #18599, #25967, #21002, #2798, #204, #28876, #29208, #13265, #29039, #23571, #543, #26646, #5714, #5542, #31451, #26138, #10692, #23908, #26309, #23404, #3140, #36, #16192, #20836, #379, #16023, #2461, #13613, #7944, #8272, #24078, #23740, #33865, #26478, #10525, #15689, #2971, #18432, #21173, #12927, #13441, #2635, #10865, #10358, #7774, #5372, #31281, #13098, #7607, #18087, #20674, #31113, #31615, #28535, #31780, #5030 ),
 ( #15853, #18261, #28707, #8112, #21339, #5205, #19064, #19395, #22138, #16654, #27618, #19729, #11827, #32582, #24535, #19229, #3771, #16987, #29843, #16482, #30174, #27109, #22303, #13908, #27445, #11657, #29503, #32749, #1006, #1346, #6677, #16822, #26938, #9081, #3602, #8745, #19562, #14076, #6344, #8580, #30010, #29666, #6516, #6008, #847, #11489, #3438, #6172, #681, #11167, #13739, #9242, #27278, #17161, #24865, #24208, #3937, #14412, #21638, #24374, #32084, #11326, #21803, #32252, #14242, #21968, #32416, #8912, #24699, #1176, #22981, #7356, #9938, #17497, #17843, #33440, #22809, #22461, #12339, #33089, #4784, #9411, #10114, #6846, #19895, #9591, #17324, #30688, #25725, #20246, #27959, #12682, #12514, #20073, #12163, #20593, #17666, #20413, #28127, #1862, #33268, #30516, #15263, #32912, #1687, #22637, #31039, #14917, #7534, #4615, #7014, #33614, #15091, #27787, #9761, #25209, #28297, #4273, #25559, #25385, #2039, #23149, #30864, #2204, #4441, #30345, #7185, #14747, #18018, #4104, #14577, #25038, #1518, #11993, #21271, #31714, #13541, #26407, #25889, #7868, #15615, #20766, #23840, #8041, #13192, #2899, #26239, #10624, #8371, #21433, #23330, #31875, #28630, #20930, #7701, #18189, #5469, #16122, #28464, #31378, #26575, #131, #26067, #10452, #15437, #23669, #33958, #13368, #305, #18360, #2560, #21101, #31210, #18696, #33794, #5129, #2728, #3071, #10793, #31545, #28804, #24004, #13027, #18527, #475, #28973, #4957, #8206, #23501, #29136, #5301, #5638, #2385, #15783, #15951, #10958, #12855, #10288, #24659, #32377, #6476, #29468, #811, #3732, #11616, #11129, #970, #11784, #27070, #22098, #29305, #24169, #16779, #26902, #5806, #29801, #21600, #16285, #3562, #13704, #6303, #14367, #11292, #14035, #640, #3896, #29628, #19521, #13871, #26743, #24338, #3401, #21771, #5973, #29969, #16450, #18858, #32215, #19190, #32043, #3236, #8707, #32543, #24824, #27239, #8543, #6131, #16615, #19028, #14203, #8873, #24497, #1131, #11452, #21927, #32706, #22264, #19357, #9042, #16948, #27406, #1303, #32870, #20201, #30820, #9201, #12118, #7312, #14874, #6802, #25164, #30132, #27917, #14706, #17622, #15050, #22590, #17281, #4400, #11952, #33395, #4062, #9367, #17457, #17797, #4572, #25339, #1642, #28256, #19849, #1816, #4740, #12294, #2163, #25515, #4232, #1994, #30302, #28083, #17115, #27742, #22766, #12469, #9718, #6635, #22939, #33219, #15220, #33043, #9546, #9894, #20371, #1478, #30644, #12637, #7141, #25683, #19686, #14534, #23107, #20027, #27573, #24995, #22421, #30473, #6972, #28425, #10581, #29094, #15572, #18318, #4914, #18656, #10410, #264, #28589, #30996, #5087, #18146, #26026, #10246, #10751, #31168, #33571, #2518, #33920, #15394, #10069, #7659, #31337, #20727, #23798, #2340, #23626, #20888, #93, #8166, #21059, #21229, #12985, #17975, #26196, #12813, #23458, #5260, #5598, #16081, #7494, #31672, #26365, #26535, #7829, #2855, #20549, #25850, #31509, #28764, #23285, #8002, #33752, #15742, #2691, #13151, #18487, #3029, #28930, #5429, #15910, #13501, #13325, #24620, #18988, #21392, #29432, #8500, #5935, #598, #1094, #21560, #23966, #16414, #24300, #18820, #436, #32004, #21730, #11090, #14164, #26703, #13997, #772, #24458, #32502, #11413, #11577, #26866, #8331, #16574, #3200, #13831, #29591, #29932, #9002, #31837, #22058, #16742, #27200, #19483, #21889, #29264, #3361, #11253, #16247, #19316, #3524, #8669, #32339, #32175, #6092, #3855, #16907, #5767, #27369, #24132, #19152, #13668, #27029, #934, #6436, #10920, #8833, #29758, #6264, #3691, #30262, #1264, #33000, #19812, #22731, #20165, #27705, #22386, #9507, #17074, #4535, #9165, #14497, #22549, #22901, #9682, #19988, #6765, #12432, #4022, #6935, #1958, #30435, #7276, #30608, #9326, #7104, #24954, #33180, #22223, #32835, #17418, #17587, #14838, #11743, #28048, #27879, #33360, #1436, #17244, #15009, #25479, #6598, #4363, #9856, #20333, #30783, #4194, #17759, #28217, #25304, #32670, #1774, #14666, #14329, #19649, #24785, #27534, #30091, #25126, #11915, #12254, #1604, #12081, #18103, #13281, #13114, #33711, #12776, #10709, #18279, #23588, #28725, #2478, #12945, #31131, #5391, #23072, #2304, #23250, #21189, #15532, #31631, #5220, #7623, #221, #15703, #28389, #10209, #4878, #25814, #33533, #28551, #10036, #25985, #15869, #20511, #20690, #26326, #5049, #30957, #2814, #2652, #7455, #23418, #20851, #21018, #23756, #17939, #10373, #53, #33880, #18617, #8129, #4704, #10541, #31297, #7789, #26157, #7961, #31470, #15359, #15185, #18448, #25649, #28891, #2127, #12603, #10881, #14124, #5894, #16700, #22015, #32133, #31798, #24417, #8460, #24094, #13954, #18949, #11213, #23927, #894, #11052, #11375, #396, #16208, #29394, #21356, #21517, #16039, #26494, #29055, #24581, #727, #27156, #6219, #3648, #32296, #3483, #1052, #29224, #8790, #19274, #8290, #11532, #21686, #16373, #21851, #24257, #3322, #5730, #18780, #26662, #562, #3159, #8628, #32460, #19111, #26826, #8960, #29715, #31966, #13630, #5560, #29550, #2989, #6050, #13789, #16533, #26984, #13458, #4279, #17503, #27965, #2391, #30694, #12860, #33446, #12346, #15443, #30870, #9598, #14924, #20080, #7021, #14753, #33274, #25215, #7191, #31046, #1693, #4447, #7539, #20252, #12169, #18024, #17850, #22643, #17673, #2045, #2210, #25565, #30522, #12520, #25391, #1868, #6853, #4621, #22815, #28303, #25731, #9768, #28134, #15100, #33095, #10120, #22988, #9945, #20421, #28470, #15270, #7364, #4790, #4963, #12689, #23157, #25897, #33621, #23337, #20600, #33799, #19441, #30351, #17331, #27794, #18364, #26411, #13545, #10797, #7708, #16126, #23844, #31880, #20936, #26244, #29140, #3076, #2566, #2904, #3240, #18531, #24008, #20771, #15620, #8210, #28809, #31215, #21275, #13034, #18194, #28977, #5134, #31718, #5811, #2733, #5475, #26072, #29309, #21105, #10962, #5305, #28637, #15788, #13196, #23673, #31384, #21437, #7875, #5643, #309, #8045, #15955, #137, #8376, #23506, #10628, #31549, #26747, #13373, #13708, #18701, #26580, #16289, #479, #33964, #18862, #10458, #24174, #10294, #14040, #19033, #21932, #11790, #5977, #32221, #22269 ) ),
 .UNSPECIFIED., .F., .F., .T. ) 
 B_SPLINE_SURFACE_WITH_KNOTS ( ( 2, 2 ),
 ( 3, 2, 2, 2, 2, 2, 2, 2, 2, 2, 2, 2, 2, 2, 2, 2, 2, 2, 2, 2, 2, 2, 2, 2, 2, 2, 2, 2, 2, 2, 2, 2, 2, 2, 2, 2, 2, 2, 2, 2, 2, 2, 2, 2, 2, 2, 2, 2, 2, 2, 2, 2, 2, 2, 2, 2, 2, 2, 2, 2, 2, 2, 2, 2, 2, 2, 2, 2, 2, 2, 2, 2, 2, 2, 2, 2, 2, 2, 2, 2, 2, 2, 2, 2, 2, 2, 2, 2, 2, 2, 2, 2, 2, 2, 2, 2, 2, 2, 2, 2, 2, 2, 2, 2, 2, 2, 2, 2, 2, 2, 2, 2, 2, 2, 2, 2, 2, 2, 2, 2, 2, 2, 2, 2, 2, 2, 2, 2, 2, 2, 2, 2, 2, 2, 2, 2, 2, 2, 2, 2, 2, 2, 2, 2, 2, 2, 2, 2, 2, 2, 2, 2, 2, 2, 2, 2, 2, 2, 2, 2, 2, 2, 2, 2, 2, 2, 2, 2, 2, 2, 2, 2, 2, 2, 2, 2, 2, 2, 2, 2, 2, 2, 2, 2, 2, 2, 2, 2, 2, 2, 2, 2, 2, 2, 2, 2, 2, 2, 2, 2, 2, 2, 2, 2, 2, 2, 2, 2, 2, 2, 2, 2, 2, 2, 2, 2, 2, 2, 2, 2, 2, 2, 2, 2, 2, 2, 2, 2, 2, 2, 2, 2, 2, 2, 2, 2, 2, 2, 2, 2, 2, 2, 2, 2, 2, 2, 2, 2, 2, 2, 2, 2, 2, 2, 2, 2, 2, 2, 2, 2, 2, 2, 2, 2, 2, 2, 2, 2, 2, 2, 2, 2, 2, 2, 2, 2, 2, 2, 2, 2, 2, 2, 2, 2, 2, 2, 2, 2, 2, 2, 2, 2, 2, 2, 2, 2, 2, 2, 2, 2, 2, 2, 2, 2, 2, 2, 2, 2, 2, 2, 2, 2, 2, 2, 2, 2, 2, 2, 2, 2, 2, 2, 2, 2, 2, 2, 2, 2, 2, 2, 2, 2, 2, 2, 2, 2, 2, 2, 2, 2, 2, 2, 2, 2, 2, 2, 2, 2, 2, 2, 2, 2, 2, 2, 2, 2, 2, 2, 2, 2, 2, 2, 2, 2, 2, 2, 2, 2, 2, 2, 2, 2, 2, 2, 2, 2, 2, 2, 2, 2, 2, 2, 2, 2, 2, 2, 2, 2, 2, 2, 3 ),
 ( 0.000000000000000000, 1.000000000000000000 ),
 ( 0.000000000000000000, 0.002564102564102564100, 0.005128205128205128201, 0.007692307692307692735, 0.01025641025641025640, 0.01282051282051282007, 0.01538461538461538547, 0.01794871794871794740, 0.02051282051282051280, 0.02307692307692307820, 0.02564102564102564014, 0.02820512820512820554, 0.03076923076923077094, 0.03333333333333333287, 0.03589743589743589480, 0.03846153846153846367, 0.04102564102564102561, 0.04358974358974358754, 0.04615384615384615641, 0.04871794871794871834, 0.05128205128205128027, 0.05384615384615384914, 0.05641025641025641107, 0.05897435897435897301, 0.06153846153846154188, 0.06410256410256409687, 0.06666666666666666574, 0.06923076923076923461, 0.07179487179487178961, 0.07435897435897435848, 0.07692307692307692735, 0.07948717948717948234, 0.08205128205128205121, 0.08461538461538462008, 0.08717948717948717507, 0.08974358974358974395, 0.09230769230769231282, 0.09487179487179486781, 0.09743589743589743668, 0.1000000000000000056, 0.1025641025641025605, 0.1051282051282051294, 0.1076923076923076983, 0.1102564102564102533, 0.1128205128205128221, 0.1153846153846153910, 0.1179487179487179460, 0.1205128205128205149, 0.1230769230769230838, 0.1256410256410256387, 0.1282051282051281937, 0.1307692307692307765, 0.1333333333333333315, 0.1358974358974358865, 0.1384615384615384692, 0.1410256410256410242, 0.1435897435897435792, 0.1461538461538461620, 0.1487179487179487170, 0.1512820512820512719, 0.1538461538461538547, 0.1564102564102564097, 0.1589743589743589647, 0.1615384615384615474, 0.1641025641025641024, 0.1666666666666666574, 0.1692307692307692402, 0.1717948717948717952, 0.1743589743589743501, 0.1769230769230769329, 0.1794871794871794879, 0.1820512820512820429, 0.1846153846153846256, 0.1871794871794871806, 0.1897435897435897356, 0.1923076923076923184, 0.1948717948717948734, 0.1974358974358974284, 0.2000000000000000111, 0.2025641025641025661, 0.2051282051282051211, 0.2076923076923077038, 0.2102564102564102588, 0.2128205128205128138, 0.2153846153846153966, 0.2179487179487179516, 0.2205128205128205066, 0.2230769230769230893, 0.2256410256410256443, 0.2282051282051281993, 0.2307692307692307820, 0.2333333333333333370, 0.2358974358974358920, 0.2384615384615384748, 0.2410256410256410298, 0.2435897435897435848, 0.2461538461538461675, 0.2487179487179487225, 0.2512820512820512775, 0.2538461538461538325, 0.2564102564102563875, 0.2589743589743589980, 0.2615384615384615530, 0.2641025641025641080, 0.2666666666666666630, 0.2692307692307692180, 0.2717948717948717730, 0.2743589743589743835, 0.2769230769230769384, 0.2794871794871794934, 0.2820512820512820484, 0.2846153846153846034, 0.2871794871794871584, 0.2897435897435897689, 0.2923076923076923239, 0.2948717948717948789, 0.2974358974358974339, 0.2999999999999999889, 0.3025641025641025439, 0.3051282051282051544, 0.3076923076923077094, 0.3102564102564102644, 0.3128205128205128194, 0.3153846153846153744, 0.3179487179487179294, 0.3205128205128205399, 0.3230769230769230949, 0.3256410256410256499, 0.3282051282051282048, 0.3307692307692307598, 0.3333333333333333148, 0.3358974358974358698, 0.3384615384615384803, 0.3410256410256410353, 0.3435897435897435903, 0.3461538461538461453, 0.3487179487179487003, 0.3512820512820512553, 0.3538461538461538658, 0.3564102564102564208, 0.3589743589743589758, 0.3615384615384615308, 0.3641025641025640858, 0.3666666666666666408, 0.3692307692307692513, 0.3717948717948718063, 0.3743589743589743613, 0.3769230769230769162, 0.3794871794871794712, 0.3820512820512820262, 0.3846153846153846367, 0.3871794871794871917, 0.3897435897435897467, 0.3923076923076923017, 0.3948717948717948567, 0.3974358974358974117, 0.4000000000000000222, 0.4025641025641025772, 0.4051282051282051322, 0.4076923076923076872, 0.4102564102564102422, 0.4128205128205127972, 0.4153846153846154077, 0.4179487179487179627, 0.4205128205128205177, 0.4230769230769230727, 0.4256410256410256276, 0.4282051282051281826, 0.4307692307692307931, 0.4333333333333333481, 0.4358974358974359031, 0.4384615384615384581, 0.4410256410256410131, 0.4435897435897435681, 0.4461538461538461786, 0.4487179487179487336, 0.4512820512820512886, 0.4538461538461538436, 0.4564102564102563986, 0.4589743589743589536, 0.4615384615384615641, 0.4641025641025641191, 0.4666666666666666741, 0.4692307692307692291, 0.4717948717948717841, 0.4743589743589743390, 0.4769230769230769496, 0.4794871794871795045, 0.4820512820512820595, 0.4846153846153846145, 0.4871794871794871695, 0.4897435897435897245, 0.4923076923076923350, 0.4948717948717948900, 0.4974358974358974450, 0.5000000000000000000, 0.5025641025641025550, 0.5051282051282051100, 0.5076923076923076650, 0.5102564102564102200, 0.5128205128205127750, 0.5153846153846153300, 0.5179487179487179960, 0.5205128205128205510, 0.5230769230769231060, 0.5256410256410256610, 0.5282051282051282159, 0.5307692307692307709, 0.5333333333333333259, 0.5358974358974358809, 0.5384615384615384359, 0.5410256410256409909, 0.5435897435897435459, 0.5461538461538461009, 0.5487179487179487669, 0.5512820512820513219, 0.5538461538461538769, 0.5564102564102564319, 0.5589743589743589869, 0.5615384615384615419, 0.5641025641025640969, 0.5666666666666666519, 0.5692307692307692069, 0.5717948717948717618, 0.5743589743589743168, 0.5769230769230768718, 0.5794871794871795379, 0.5820512820512820928, 0.5846153846153846478, 0.5871794871794872028, 0.5897435897435897578, 0.5923076923076923128, 0.5948717948717948678, 0.5974358974358974228, 0.5999999999999999778, 0.6025641025641025328, 0.6051282051282050878, 0.6076923076923076428, 0.6102564102564103088, 0.6128205128205128638, 0.6153846153846154188, 0.6179487179487179738, 0.6205128205128205288, 0.6230769230769230838, 0.6256410256410256387, 0.6282051282051281937, 0.6307692307692307487, 0.6333333333333333037, 0.6358974358974358587, 0.6384615384615384137, 0.6410256410256410797, 0.6435897435897436347, 0.6461538461538461897, 0.6487179487179487447, 0.6512820512820512997, 0.6538461538461538547, 0.6564102564102564097, 0.6589743589743589647, 0.6615384615384615197, 0.6641025641025640747, 0.6666666666666666297, 0.6692307692307691847, 0.6717948717948717396, 0.6743589743589744057, 0.6769230769230769607, 0.6794871794871795156, 0.6820512820512820706, 0.6846153846153846256, 0.6871794871794871806, 0.6897435897435897356, 0.6923076923076922906, 0.6948717948717948456, 0.6974358974358974006, 0.6999999999999999556, 0.7025641025641025106, 0.7051282051282051766, 0.7076923076923077316, 0.7102564102564102866, 0.7128205128205128416, 0.7153846153846153966, 0.7179487179487179516, 0.7205128205128205066, 0.7230769230769230616, 0.7256410256410256165, 0.7282051282051281715, 0.7307692307692307265, 0.7333333333333332815, 0.7358974358974359475, 0.7384615384615385025, 0.7410256410256410575, 0.7435897435897436125, 0.7461538461538461675, 0.7487179487179487225, 0.7512820512820512775, 0.7538461538461538325, 0.7564102564102563875, 0.7589743589743589425, 0.7615384615384614975, 0.7641025641025640525, 0.7666666666666667185, 0.7692307692307692735, 0.7717948717948718285, 0.7743589743589743835, 0.7769230769230769384, 0.7794871794871794934, 0.7820512820512820484, 0.7846153846153846034, 0.7871794871794871584, 0.7897435897435897134, 0.7923076923076922684, 0.7948717948717948234, 0.7974358974358974894, 0.8000000000000000444, 0.8025641025641025994, 0.8051282051282051544, 0.8076923076923077094, 0.8102564102564102644, 0.8128205128205128194, 0.8153846153846153744, 0.8179487179487179294, 0.8205128205128204844, 0.8230769230769230393, 0.8256410256410255943, 0.8282051282051282604, 0.8307692307692308153, 0.8333333333333333703, 0.8358974358974359253, 0.8384615384615384803, 0.8410256410256410353, 0.8435897435897435903, 0.8461538461538461453, 0.8487179487179487003, 0.8512820512820512553, 0.8538461538461538103, 0.8564102564102563653, 0.8589743589743589203, 0.8615384615384615863, 0.8641025641025641413, 0.8666666666666666963, 0.8692307692307692513, 0.8717948717948718063, 0.8743589743589743613, 0.8769230769230769162, 0.8794871794871794712, 0.8820512820512820262, 0.8846153846153845812, 0.8871794871794871362, 0.8897435897435896912, 0.8923076923076923572, 0.8948717948717949122, 0.8974358974358974672, 0.9000000000000000222, 0.9025641025641025772, 0.9051282051282051322, 0.9076923076923076872, 0.9102564102564102422, 0.9128205128205127972, 0.9153846153846153522, 0.9179487179487179072, 0.9205128205128204621, 0.9230769230769231282, 0.9256410256410256832, 0.9282051282051282382, 0.9307692307692307931, 0.9333333333333333481, 0.9358974358974359031, 0.9384615384615384581, 0.9410256410256410131, 0.9435897435897435681, 0.9461538461538461231, 0.9487179487179486781, 0.9512820512820512331, 0.9538461538461538991, 0.9564102564102564541, 0.9589743589743590091, 0.9615384615384615641, 0.9641025641025641191, 0.9666666666666666741, 0.9692307692307692291, 0.9717948717948717841, 0.9743589743589743390, 0.9769230769230768940, 0.9794871794871794490, 0.9820512820512820040, 0.9846153846153846700, 0.9871794871794872250, 0.9897435897435897800, 0.9923076923076923350, 0.9948717948717948900, 0.9974358974358974450, 1.000000000000000000 ),
 .UNSPECIFIED. ) 
 GEOMETRIC_REPRESENTATION_ITEM ( )  RATIONAL_B_SPLINE_SURFACE ( (
 ( 1.000000000000000000, 0.9510565162951535312, 1.000000000000000000, 0.9510565162951535312, 1.000000000000000000, 0.9510565162951535312, 1.000000000000000000, 0.9510565162951535312, 1.000000000000000000, 0.9510565162951535312, 1.000000000000000000, 0.9510565162951535312, 1.000000000000000000, 0.9510565162951535312, 1.000000000000000000, 0.9510565162951535312, 1.000000000000000000, 0.9510565162951535312, 1.000000000000000000, 0.9510565162951535312, 1.000000000000000000, 0.9510565162951535312, 1.000000000000000000, 0.9510565162951535312, 1.000000000000000000, 0.9510565162951535312, 1.000000000000000000, 0.9510565162951535312, 1.000000000000000000, 0.9510565162951535312, 1.000000000000000000, 0.9510565162951535312, 1.000000000000000000, 0.9510565162951535312, 1.000000000000000000, 0.9510565162951535312, 1.000000000000000000, 0.9510565162951535312, 1.000000000000000000, 0.9510565162951535312, 1.000000000000000000, 0.9510565162951535312, 1.000000000000000000, 0.9510565162951535312, 1.000000000000000000, 0.9510565162951535312, 1.000000000000000000, 0.9510565162951535312, 1.000000000000000000, 0.9510565162951535312, 1.000000000000000000, 0.9510565162951535312, 1.000000000000000000, 0.9510565162951535312, 1.000000000000000000, 0.9510565162951535312, 1.000000000000000000, 0.9510565162951535312, 1.000000000000000000, 0.9510565162951535312, 1.000000000000000000, 0.9510565162951535312, 1.000000000000000000, 0.9510565162951535312, 1.000000000000000000, 0.9510565162951535312, 1.000000000000000000, 0.9510565162951535312, 1.000000000000000000, 0.9510565162951535312, 1.000000000000000000, 0.9510565162951535312, 1.000000000000000000, 0.9510565162951535312, 1.000000000000000000, 0.9510565162951535312, 1.000000000000000000, 0.9510565162951535312, 1.000000000000000000, 0.9510565162951535312, 1.000000000000000000, 0.9510565162951535312, 1.000000000000000000, 0.9510565162951535312, 1.000000000000000000, 0.9510565162951535312, 1.000000000000000000, 0.9510565162951535312, 1.000000000000000000, 0.9510565162951535312, 1.000000000000000000, 0.9510565162951535312, 1.000000000000000000, 0.9510565162951535312, 1.000000000000000000, 0.9510565162951535312, 1.000000000000000000, 0.9510565162951535312, 1.000000000000000000, 0.9510565162951535312, 1.000000000000000000, 0.9510565162951535312, 1.000000000000000000, 0.9510565162951535312, 1.000000000000000000, 0.9510565162951535312, 1.000000000000000000, 0.9510565162951535312, 1.000000000000000000, 0.9510565162951535312, 1.000000000000000000, 0.9510565162951535312, 1.000000000000000000, 0.9510565162951535312, 1.000000000000000000, 0.9510565162951535312, 1.000000000000000000, 0.9510565162951535312, 1.000000000000000000, 0.9510565162951535312, 1.000000000000000000, 0.9510565162951535312, 1.000000000000000000, 0.9510565162951535312, 1.000000000000000000, 0.9510565162951535312, 1.000000000000000000, 0.9510565162951535312, 1.000000000000000000, 0.9510565162951535312, 1.000000000000000000, 0.9510565162951535312, 1.000000000000000000, 0.9510565162951535312, 1.000000000000000000, 0.9510565162951535312, 1.000000000000000000, 0.9510565162951535312, 1.000000000000000000, 0.9510565162951535312, 1.000000000000000000, 0.9510565162951535312, 1.000000000000000000, 0.9510565162951535312, 1.000000000000000000, 0.9510565162951535312, 1.000000000000000000, 0.9510565162951535312, 1.000000000000000000, 0.9510565162951535312, 1.000000000000000000, 0.9510565162951535312, 1.000000000000000000, 0.9510565162951535312, 1.000000000000000000, 0.9510565162951535312, 1.000000000000000000, 0.9510565162951535312, 1.000000000000000000, 0.9510565162951535312, 1.000000000000000000, 0.9510565162951535312, 1.000000000000000000, 0.9510565162951535312, 1.000000000000000000, 0.9510565162951535312, 1.000000000000000000, 0.9510565162951535312, 1.000000000000000000, 0.9510565162951535312, 1.000000000000000000, 0.9510565162951535312, 1.000000000000000000, 0.9510565162951535312, 1.000000000000000000, 0.9510565162951535312, 1.000000000000000000, 0.9510565162951535312, 1.000000000000000000, 0.9510565162951535312, 1.000000000000000000, 0.9510565162951535312, 1.000000000000000000, 0.9510565162951535312, 1.000000000000000000, 0.9510565162951535312, 1.000000000000000000, 0.9510565162951535312, 1.000000000000000000, 0.9510565162951535312, 1.000000000000000000, 0.9510565162951535312, 1.000000000000000000, 0.9510565162951535312, 1.000000000000000000, 0.9510565162951535312, 1.000000000000000000, 0.9510565162951535312, 1.000000000000000000, 0.9510565162951535312, 1.000000000000000000, 0.9510565162951535312, 1.000000000000000000, 0.9510565162951535312, 1.000000000000000000, 0.9510565162951535312, 1.000000000000000000, 0.9510565162951535312, 1.000000000000000000, 0.9510565162951535312, 1.000000000000000000, 0.9510565162951535312, 1.000000000000000000, 0.9510565162951535312, 1.000000000000000000, 0.9510565162951535312, 1.000000000000000000, 0.9510565162951535312, 1.000000000000000000, 0.9510565162951535312, 1.000000000000000000, 0.9510565162951535312, 1.000000000000000000, 0.9510565162951535312, 1.000000000000000000, 0.9510565162951535312, 1.000000000000000000, 0.9510565162951535312, 1.000000000000000000, 0.9510565162951535312, 1.000000000000000000, 0.9510565162951535312, 1.000000000000000000, 0.9510565162951535312, 1.000000000000000000, 0.9510565162951535312, 1.000000000000000000, 0.9510565162951535312, 1.000000000000000000, 0.9510565162951535312, 1.000000000000000000, 0.9510565162951535312, 1.000000000000000000, 0.9510565162951535312, 1.000000000000000000, 0.9510565162951535312, 1.000000000000000000, 0.9510565162951535312, 1.000000000000000000, 0.9510565162951535312, 1.000000000000000000, 0.9510565162951535312, 1.000000000000000000, 0.9510565162951535312, 1.000000000000000000, 0.9510565162951535312, 1.000000000000000000, 0.9510565162951535312, 1.000000000000000000, 0.9510565162951535312, 1.000000000000000000, 0.9510565162951535312, 1.000000000000000000, 0.9510565162951535312, 1.000000000000000000, 0.9510565162951535312, 1.000000000000000000, 0.9510565162951535312, 1.000000000000000000, 0.9510565162951535312, 1.000000000000000000, 0.9510565162951535312, 1.000000000000000000, 0.9510565162951535312, 1.000000000000000000, 0.9510565162951535312, 1.000000000000000000, 0.9510565162951535312, 1.000000000000000000, 0.9510565162951535312, 1.000000000000000000, 0.9510565162951535312, 1.000000000000000000, 0.9510565162951535312, 1.000000000000000000, 0.9510565162951535312, 1.000000000000000000, 0.9510565162951535312, 1.000000000000000000, 0.9510565162951535312, 1.000000000000000000, 0.9510565162951535312, 1.000000000000000000, 0.9510565162951535312, 1.000000000000000000, 0.9510565162951535312, 1.000000000000000000, 0.9510565162951535312, 1.000000000000000000, 0.9510565162951535312, 1.000000000000000000, 0.9510565162951535312, 1.000000000000000000, 0.9510565162951535312, 1.000000000000000000, 0.9510565162951535312, 1.000000000000000000, 0.9510565162951535312, 1.000000000000000000, 0.9510565162951535312, 1.000000000000000000, 0.9510565162951535312, 1.000000000000000000, 0.9510565162951535312, 1.000000000000000000, 0.9510565162951535312, 1.000000000000000000, 0.9510565162951535312, 1.000000000000000000, 0.9510565162951535312, 1.000000000000000000, 0.9510565162951535312, 1.000000000000000000, 0.9510565162951535312, 1.000000000000000000, 0.9510565162951535312, 1.000000000000000000, 0.9510565162951535312, 1.000000000000000000, 0.9510565162951535312, 1.000000000000000000, 0.9510565162951535312, 1.000000000000000000, 0.9510565162951535312, 1.000000000000000000, 0.9510565162951535312, 1.000000000000000000, 0.9510565162951535312, 1.000000000000000000, 0.9510565162951535312, 1.000000000000000000, 0.9510565162951535312, 1.000000000000000000, 0.9510565162951535312, 1.000000000000000000, 0.9510565162951535312, 1.000000000000000000, 0.9510565162951535312, 1.000000000000000000, 0.9510565162951535312, 1.000000000000000000, 0.9510565162951535312, 1.000000000000000000, 0.9510565162951535312, 1.000000000000000000, 0.9510565162951535312, 1.000000000000000000, 0.9510565162951535312, 1.000000000000000000, 0.9510565162951535312, 1.000000000000000000, 0.9510565162951535312, 1.000000000000000000, 0.9510565162951535312, 1.000000000000000000, 0.9510565162951535312, 1.000000000000000000, 0.9510565162951535312, 1.000000000000000000, 0.9510565162951535312, 1.000000000000000000, 0.9510565162951535312, 1.000000000000000000, 0.9510565162951535312, 1.000000000000000000, 0.9510565162951535312, 1.000000000000000000, 0.9510565162951535312, 1.000000000000000000, 0.9510565162951535312, 1.000000000000000000, 0.9510565162951535312, 1.000000000000000000, 0.9510565162951535312, 1.000000000000000000, 0.9510565162951535312, 1.000000000000000000, 0.9510565162951535312, 1.000000000000000000, 0.9510565162951535312, 1.000000000000000000, 0.9510565162951535312, 1.000000000000000000, 0.9510565162951535312, 1.000000000000000000, 0.9510565162951535312, 1.000000000000000000, 0.9510565162951535312, 1.000000000000000000, 0.9510565162951535312, 1.000000000000000000, 0.9510565162951535312, 1.000000000000000000, 0.9510565162951535312, 1.000000000000000000, 0.9510565162951535312, 1.000000000000000000, 0.9510565162951535312, 1.000000000000000000, 0.9510565162951535312, 1.000000000000000000, 0.9510565162951535312, 1.000000000000000000, 0.9510565162951535312, 1.000000000000000000, 0.9510565162951535312, 1.000000000000000000, 0.9510565162951535312, 1.000000000000000000, 0.9510565162951535312, 1.000000000000000000, 0.9510565162951535312, 1.000000000000000000, 0.9510565162951535312, 1.000000000000000000, 0.9510565162951535312, 1.000000000000000000, 0.9510565162951535312, 1.000000000000000000, 0.9510565162951535312, 1.000000000000000000, 0.9510565162951535312, 1.000000000000000000, 0.9510565162951535312, 1.000000000000000000, 0.9510565162951535312, 1.000000000000000000, 0.9510565162951535312, 1.000000000000000000, 0.9510565162951535312, 1.000000000000000000, 0.9510565162951535312, 1.000000000000000000, 0.9510565162951535312, 1.000000000000000000, 0.9510565162951535312, 1.000000000000000000, 0.9510565162951535312, 1.000000000000000000, 0.9510565162951535312, 1.000000000000000000, 0.9510565162951535312, 1.000000000000000000, 0.9510565162951535312, 1.000000000000000000, 0.9510565162951535312, 1.000000000000000000, 0.9510565162951535312, 1.000000000000000000, 0.9510565162951535312, 1.000000000000000000, 0.9510565162951535312, 1.000000000000000000, 0.9510565162951535312, 1.000000000000000000, 0.9510565162951535312, 1.000000000000000000, 0.9510565162951535312, 1.000000000000000000, 0.9510565162951535312, 1.000000000000000000, 0.9510565162951535312, 1.000000000000000000, 0.9510565162951535312, 1.000000000000000000, 0.9510565162951535312, 1.000000000000000000, 0.9510565162951535312, 1.000000000000000000, 0.9510565162951535312, 1.000000000000000000, 0.9510565162951535312, 1.000000000000000000, 0.9510565162951535312, 1.000000000000000000, 0.9510565162951535312, 1.000000000000000000, 0.9510565162951535312, 1.000000000000000000, 0.9510565162951535312, 1.000000000000000000, 0.9510565162951535312, 1.000000000000000000, 0.9510565162951535312, 1.000000000000000000, 0.9510565162951535312, 1.000000000000000000, 0.9510565162951535312, 1.000000000000000000, 0.9510565162951535312, 1.000000000000000000, 0.9510565162951535312, 1.000000000000000000, 0.9510565162951535312, 1.000000000000000000, 0.9510565162951535312, 1.000000000000000000, 0.9510565162951535312, 1.000000000000000000, 0.9510565162951535312, 1.000000000000000000, 0.9510565162951535312, 1.000000000000000000, 0.9510565162951535312, 1.000000000000000000, 0.9510565162951535312, 1.000000000000000000, 0.9510565162951535312, 1.000000000000000000, 0.9510565162951535312, 1.000000000000000000, 0.9510565162951535312, 1.000000000000000000, 0.9510565162951535312, 1.000000000000000000, 0.9510565162951535312, 1.000000000000000000, 0.9510565162951535312, 1.000000000000000000, 0.9510565162951535312, 1.000000000000000000, 0.9510565162951535312, 1.000000000000000000, 0.9510565162951535312, 1.000000000000000000, 0.9510565162951535312, 1.000000000000000000, 0.9510565162951535312, 1.000000000000000000, 0.9510565162951535312, 1.000000000000000000, 0.9510565162951535312, 1.000000000000000000, 0.9510565162951535312, 1.000000000000000000, 0.9510565162951535312, 1.000000000000000000, 0.9510565162951535312, 1.000000000000000000, 0.9510565162951535312, 1.000000000000000000, 0.9510565162951535312, 1.000000000000000000, 0.9510565162951535312, 1.000000000000000000, 0.9510565162951535312, 1.000000000000000000, 0.9510565162951535312, 1.000000000000000000, 0.9510565162951535312, 1.000000000000000000, 0.9510565162951535312, 1.000000000000000000, 0.9510565162951535312, 1.000000000000000000, 0.9510565162951535312, 1.000000000000000000, 0.9510565162951535312, 1.000000000000000000, 0.9510565162951535312, 1.000000000000000000, 0.9510565162951535312, 1.000000000000000000, 0.9510565162951535312, 1.000000000000000000, 0.9510565162951535312, 1.000000000000000000, 0.9510565162951535312, 1.000000000000000000, 0.9510565162951535312, 1.000000000000000000, 0.9510565162951535312, 1.000000000000000000, 0.9510565162951535312, 1.000000000000000000, 0.9510565162951535312, 1.000000000000000000, 0.9510565162951535312, 1.000000000000000000, 0.9510565162951535312, 1.000000000000000000, 0.9510565162951535312, 1.000000000000000000, 0.9510565162951535312, 1.000000000000000000, 0.9510565162951535312, 1.000000000000000000, 0.9510565162951535312, 1.000000000000000000, 0.9510565162951535312, 1.000000000000000000, 0.9510565162951535312, 1.000000000000000000, 0.9510565162951535312, 1.000000000000000000, 0.9510565162951535312, 1.000000000000000000, 0.9510565162951535312, 1.000000000000000000, 0.9510565162951535312, 1.000000000000000000, 0.9510565162951535312, 1.000000000000000000, 0.9510565162951535312, 1.000000000000000000, 0.9510565162951535312, 1.000000000000000000, 0.9510565162951535312, 1.000000000000000000, 0.9510565162951535312, 1.000000000000000000, 0.9510565162951535312, 1.000000000000000000, 0.9510565162951535312, 1.000000000000000000, 0.9510565162951535312, 1.000000000000000000, 0.9510565162951535312, 1.000000000000000000, 0.9510565162951535312, 1.000000000000000000, 0.9510565162951535312, 1.000000000000000000, 0.9510565162951535312, 1.000000000000000000, 0.9510565162951535312, 1.000000000000000000, 0.9510565162951535312, 1.000000000000000000, 0.9510565162951535312, 1.000000000000000000, 0.9510565162951535312, 1.000000000000000000, 0.9510565162951535312, 1.000000000000000000, 0.9510565162951535312, 1.000000000000000000, 0.9510565162951535312, 1.000000000000000000, 0.9510565162951535312, 1.000000000000000000, 0.9510565162951535312, 1.000000000000000000, 0.9510565162951535312, 1.000000000000000000, 0.9510565162951535312, 1.000000000000000000, 0.9510565162951535312, 1.000000000000000000, 0.9510565162951535312, 1.000000000000000000, 0.9510565162951535312, 1.000000000000000000, 0.9510565162951535312, 1.000000000000000000, 0.9510565162951535312, 1.000000000000000000, 0.9510565162951535312, 1.000000000000000000, 0.9510565162951535312, 1.000000000000000000, 0.9510565162951535312, 1.000000000000000000, 0.9510565162951535312, 1.000000000000000000, 0.9510565162951535312, 1.000000000000000000, 0.9510565162951535312, 1.000000000000000000, 0.9510565162951535312, 1.000000000000000000, 0.9510565162951535312, 1.000000000000000000, 0.9510565162951535312, 1.000000000000000000, 0.9510565162951535312, 1.000000000000000000, 0.9510565162951535312, 1.000000000000000000, 0.9510565162951535312, 1.000000000000000000, 0.9510565162951535312, 1.000000000000000000, 0.9510565162951535312, 1.000000000000000000, 0.9510565162951535312, 1.000000000000000000, 0.9510565162951535312, 1.000000000000000000, 0.9510565162951535312, 1.000000000000000000, 0.9510565162951535312, 1.000000000000000000, 0.9510565162951535312, 1.000000000000000000, 0.9510565162951535312, 1.000000000000000000, 0.9510565162951535312, 1.000000000000000000, 0.9510565162951535312, 1.000000000000000000, 0.9510565162951535312, 1.000000000000000000, 0.9510565162951535312, 1.000000000000000000, 0.9510565162951535312, 1.000000000000000000, 0.9510565162951535312, 1.000000000000000000, 0.9510565162951535312, 1.000000000000000000, 0.9510565162951535312, 1.000000000000000000, 0.9510565162951535312, 1.000000000000000000, 0.9510565162951535312, 1.000000000000000000, 0.9510565162951535312, 1.000000000000000000, 0.9510565162951535312, 1.000000000000000000, 0.9510565162951535312, 1.000000000000000000, 0.9510565162951535312, 1.000000000000000000, 0.9510565162951535312, 1.000000000000000000, 0.9510565162951535312, 1.000000000000000000, 0.9510565162951535312, 1.000000000000000000, 0.9510565162951535312, 1.000000000000000000, 0.9510565162951535312, 1.000000000000000000, 0.9510565162951535312, 1.000000000000000000, 0.9510565162951535312, 1.000000000000000000, 0.9510565162951535312, 1.000000000000000000, 0.9510565162951535312, 1.000000000000000000, 0.9510565162951535312, 1.000000000000000000, 0.9510565162951535312, 1.000000000000000000, 0.9510565162951535312, 1.000000000000000000, 0.9510565162951535312, 1.000000000000000000, 0.9510565162951535312, 1.000000000000000000, 0.9510565162951535312, 1.000000000000000000, 0.9510565162951535312, 1.000000000000000000, 0.9510565162951535312, 1.000000000000000000, 0.9510565162951535312, 1.000000000000000000, 0.9510565162951535312, 1.000000000000000000, 0.9510565162951535312, 1.000000000000000000, 0.9510565162951535312, 1.000000000000000000, 0.9510565162951535312, 1.000000000000000000, 0.9510565162951535312, 1.000000000000000000),
 ( 1.000000000000000000, 0.9510565162951535312, 1.000000000000000000, 0.9510565162951535312, 1.000000000000000000, 0.9510565162951535312, 1.000000000000000000, 0.9510565162951535312, 1.000000000000000000, 0.9510565162951535312, 1.000000000000000000, 0.9510565162951535312, 1.000000000000000000, 0.9510565162951535312, 1.000000000000000000, 0.9510565162951535312, 1.000000000000000000, 0.9510565162951535312, 1.000000000000000000, 0.9510565162951535312, 1.000000000000000000, 0.9510565162951535312, 1.000000000000000000, 0.9510565162951535312, 1.000000000000000000, 0.9510565162951535312, 1.000000000000000000, 0.9510565162951535312, 1.000000000000000000, 0.9510565162951535312, 1.000000000000000000, 0.9510565162951535312, 1.000000000000000000, 0.9510565162951535312, 1.000000000000000000, 0.9510565162951535312, 1.000000000000000000, 0.9510565162951535312, 1.000000000000000000, 0.9510565162951535312, 1.000000000000000000, 0.9510565162951535312, 1.000000000000000000, 0.9510565162951535312, 1.000000000000000000, 0.9510565162951535312, 1.000000000000000000, 0.9510565162951535312, 1.000000000000000000, 0.9510565162951535312, 1.000000000000000000, 0.9510565162951535312, 1.000000000000000000, 0.9510565162951535312, 1.000000000000000000, 0.9510565162951535312, 1.000000000000000000, 0.9510565162951535312, 1.000000000000000000, 0.9510565162951535312, 1.000000000000000000, 0.9510565162951535312, 1.000000000000000000, 0.9510565162951535312, 1.000000000000000000, 0.9510565162951535312, 1.000000000000000000, 0.9510565162951535312, 1.000000000000000000, 0.9510565162951535312, 1.000000000000000000, 0.9510565162951535312, 1.000000000000000000, 0.9510565162951535312, 1.000000000000000000, 0.9510565162951535312, 1.000000000000000000, 0.9510565162951535312, 1.000000000000000000, 0.9510565162951535312, 1.000000000000000000, 0.9510565162951535312, 1.000000000000000000, 0.9510565162951535312, 1.000000000000000000, 0.9510565162951535312, 1.000000000000000000, 0.9510565162951535312, 1.000000000000000000, 0.9510565162951535312, 1.000000000000000000, 0.9510565162951535312, 1.000000000000000000, 0.9510565162951535312, 1.000000000000000000, 0.9510565162951535312, 1.000000000000000000, 0.9510565162951535312, 1.000000000000000000, 0.9510565162951535312, 1.000000000000000000, 0.9510565162951535312, 1.000000000000000000, 0.9510565162951535312, 1.000000000000000000, 0.9510565162951535312, 1.000000000000000000, 0.9510565162951535312, 1.000000000000000000, 0.9510565162951535312, 1.000000000000000000, 0.9510565162951535312, 1.000000000000000000, 0.9510565162951535312, 1.000000000000000000, 0.9510565162951535312, 1.000000000000000000, 0.9510565162951535312, 1.000000000000000000, 0.9510565162951535312, 1.000000000000000000, 0.9510565162951535312, 1.000000000000000000, 0.9510565162951535312, 1.000000000000000000, 0.9510565162951535312, 1.000000000000000000, 0.9510565162951535312, 1.000000000000000000, 0.9510565162951535312, 1.000000000000000000, 0.9510565162951535312, 1.000000000000000000, 0.9510565162951535312, 1.000000000000000000, 0.9510565162951535312, 1.000000000000000000, 0.9510565162951535312, 1.000000000000000000, 0.9510565162951535312, 1.000000000000000000, 0.9510565162951535312, 1.000000000000000000, 0.9510565162951535312, 1.000000000000000000, 0.9510565162951535312, 1.000000000000000000, 0.9510565162951535312, 1.000000000000000000, 0.9510565162951535312, 1.000000000000000000, 0.9510565162951535312, 1.000000000000000000, 0.9510565162951535312, 1.000000000000000000, 0.9510565162951535312, 1.000000000000000000, 0.9510565162951535312, 1.000000000000000000, 0.9510565162951535312, 1.000000000000000000, 0.9510565162951535312, 1.000000000000000000, 0.9510565162951535312, 1.000000000000000000, 0.9510565162951535312, 1.000000000000000000, 0.9510565162951535312, 1.000000000000000000, 0.9510565162951535312, 1.000000000000000000, 0.9510565162951535312, 1.000000000000000000, 0.9510565162951535312, 1.000000000000000000, 0.9510565162951535312, 1.000000000000000000, 0.9510565162951535312, 1.000000000000000000, 0.9510565162951535312, 1.000000000000000000, 0.9510565162951535312, 1.000000000000000000, 0.9510565162951535312, 1.000000000000000000, 0.9510565162951535312, 1.000000000000000000, 0.9510565162951535312, 1.000000000000000000, 0.9510565162951535312, 1.000000000000000000, 0.9510565162951535312, 1.000000000000000000, 0.9510565162951535312, 1.000000000000000000, 0.9510565162951535312, 1.000000000000000000, 0.9510565162951535312, 1.000000000000000000, 0.9510565162951535312, 1.000000000000000000, 0.9510565162951535312, 1.000000000000000000, 0.9510565162951535312, 1.000000000000000000, 0.9510565162951535312, 1.000000000000000000, 0.9510565162951535312, 1.000000000000000000, 0.9510565162951535312, 1.000000000000000000, 0.9510565162951535312, 1.000000000000000000, 0.9510565162951535312, 1.000000000000000000, 0.9510565162951535312, 1.000000000000000000, 0.9510565162951535312, 1.000000000000000000, 0.9510565162951535312, 1.000000000000000000, 0.9510565162951535312, 1.000000000000000000, 0.9510565162951535312, 1.000000000000000000, 0.9510565162951535312, 1.000000000000000000, 0.9510565162951535312, 1.000000000000000000, 0.9510565162951535312, 1.000000000000000000, 0.9510565162951535312, 1.000000000000000000, 0.9510565162951535312, 1.000000000000000000, 0.9510565162951535312, 1.000000000000000000, 0.9510565162951535312, 1.000000000000000000, 0.9510565162951535312, 1.000000000000000000, 0.9510565162951535312, 1.000000000000000000, 0.9510565162951535312, 1.000000000000000000, 0.9510565162951535312, 1.000000000000000000, 0.9510565162951535312, 1.000000000000000000, 0.9510565162951535312, 1.000000000000000000, 0.9510565162951535312, 1.000000000000000000, 0.9510565162951535312, 1.000000000000000000, 0.9510565162951535312, 1.000000000000000000, 0.9510565162951535312, 1.000000000000000000, 0.9510565162951535312, 1.000000000000000000, 0.9510565162951535312, 1.000000000000000000, 0.9510565162951535312, 1.000000000000000000, 0.9510565162951535312, 1.000000000000000000, 0.9510565162951535312, 1.000000000000000000, 0.9510565162951535312, 1.000000000000000000, 0.9510565162951535312, 1.000000000000000000, 0.9510565162951535312, 1.000000000000000000, 0.9510565162951535312, 1.000000000000000000, 0.9510565162951535312, 1.000000000000000000, 0.9510565162951535312, 1.000000000000000000, 0.9510565162951535312, 1.000000000000000000, 0.9510565162951535312, 1.000000000000000000, 0.9510565162951535312, 1.000000000000000000, 0.9510565162951535312, 1.000000000000000000, 0.9510565162951535312, 1.000000000000000000, 0.9510565162951535312, 1.000000000000000000, 0.9510565162951535312, 1.000000000000000000, 0.9510565162951535312, 1.000000000000000000, 0.9510565162951535312, 1.000000000000000000, 0.9510565162951535312, 1.000000000000000000, 0.9510565162951535312, 1.000000000000000000, 0.9510565162951535312, 1.000000000000000000, 0.9510565162951535312, 1.000000000000000000, 0.9510565162951535312, 1.000000000000000000, 0.9510565162951535312, 1.000000000000000000, 0.9510565162951535312, 1.000000000000000000, 0.9510565162951535312, 1.000000000000000000, 0.9510565162951535312, 1.000000000000000000, 0.9510565162951535312, 1.000000000000000000, 0.9510565162951535312, 1.000000000000000000, 0.9510565162951535312, 1.000000000000000000, 0.9510565162951535312, 1.000000000000000000, 0.9510565162951535312, 1.000000000000000000, 0.9510565162951535312, 1.000000000000000000, 0.9510565162951535312, 1.000000000000000000, 0.9510565162951535312, 1.000000000000000000, 0.9510565162951535312, 1.000000000000000000, 0.9510565162951535312, 1.000000000000000000, 0.9510565162951535312, 1.000000000000000000, 0.9510565162951535312, 1.000000000000000000, 0.9510565162951535312, 1.000000000000000000, 0.9510565162951535312, 1.000000000000000000, 0.9510565162951535312, 1.000000000000000000, 0.9510565162951535312, 1.000000000000000000, 0.9510565162951535312, 1.000000000000000000, 0.9510565162951535312, 1.000000000000000000, 0.9510565162951535312, 1.000000000000000000, 0.9510565162951535312, 1.000000000000000000, 0.9510565162951535312, 1.000000000000000000, 0.9510565162951535312, 1.000000000000000000, 0.9510565162951535312, 1.000000000000000000, 0.9510565162951535312, 1.000000000000000000, 0.9510565162951535312, 1.000000000000000000, 0.9510565162951535312, 1.000000000000000000, 0.9510565162951535312, 1.000000000000000000, 0.9510565162951535312, 1.000000000000000000, 0.9510565162951535312, 1.000000000000000000, 0.9510565162951535312, 1.000000000000000000, 0.9510565162951535312, 1.000000000000000000, 0.9510565162951535312, 1.000000000000000000, 0.9510565162951535312, 1.000000000000000000, 0.9510565162951535312, 1.000000000000000000, 0.9510565162951535312, 1.000000000000000000, 0.9510565162951535312, 1.000000000000000000, 0.9510565162951535312, 1.000000000000000000, 0.9510565162951535312, 1.000000000000000000, 0.9510565162951535312, 1.000000000000000000, 0.9510565162951535312, 1.000000000000000000, 0.9510565162951535312, 1.000000000000000000, 0.9510565162951535312, 1.000000000000000000, 0.9510565162951535312, 1.000000000000000000, 0.9510565162951535312, 1.000000000000000000, 0.9510565162951535312, 1.000000000000000000, 0.9510565162951535312, 1.000000000000000000, 0.9510565162951535312, 1.000000000000000000, 0.9510565162951535312, 1.000000000000000000, 0.9510565162951535312, 1.000000000000000000, 0.9510565162951535312, 1.000000000000000000, 0.9510565162951535312, 1.000000000000000000, 0.9510565162951535312, 1.000000000000000000, 0.9510565162951535312, 1.000000000000000000, 0.9510565162951535312, 1.000000000000000000, 0.9510565162951535312, 1.000000000000000000, 0.9510565162951535312, 1.000000000000000000, 0.9510565162951535312, 1.000000000000000000, 0.9510565162951535312, 1.000000000000000000, 0.9510565162951535312, 1.000000000000000000, 0.9510565162951535312, 1.000000000000000000, 0.9510565162951535312, 1.000000000000000000, 0.9510565162951535312, 1.000000000000000000, 0.9510565162951535312, 1.000000000000000000, 0.9510565162951535312, 1.000000000000000000, 0.9510565162951535312, 1.000000000000000000, 0.9510565162951535312, 1.000000000000000000, 0.9510565162951535312, 1.000000000000000000, 0.9510565162951535312, 1.000000000000000000, 0.9510565162951535312, 1.000000000000000000, 0.9510565162951535312, 1.000000000000000000, 0.9510565162951535312, 1.000000000000000000, 0.9510565162951535312, 1.000000000000000000, 0.9510565162951535312, 1.000000000000000000, 0.9510565162951535312, 1.000000000000000000, 0.9510565162951535312, 1.000000000000000000, 0.9510565162951535312, 1.000000000000000000, 0.9510565162951535312, 1.000000000000000000, 0.9510565162951535312, 1.000000000000000000, 0.9510565162951535312, 1.000000000000000000, 0.9510565162951535312, 1.000000000000000000, 0.9510565162951535312, 1.000000000000000000, 0.9510565162951535312, 1.000000000000000000, 0.9510565162951535312, 1.000000000000000000, 0.9510565162951535312, 1.000000000000000000, 0.9510565162951535312, 1.000000000000000000, 0.9510565162951535312, 1.000000000000000000, 0.9510565162951535312, 1.000000000000000000, 0.9510565162951535312, 1.000000000000000000, 0.9510565162951535312, 1.000000000000000000, 0.9510565162951535312, 1.000000000000000000, 0.9510565162951535312, 1.000000000000000000, 0.9510565162951535312, 1.000000000000000000, 0.9510565162951535312, 1.000000000000000000, 0.9510565162951535312, 1.000000000000000000, 0.9510565162951535312, 1.000000000000000000, 0.9510565162951535312, 1.000000000000000000, 0.9510565162951535312, 1.000000000000000000, 0.9510565162951535312, 1.000000000000000000, 0.9510565162951535312, 1.000000000000000000, 0.9510565162951535312, 1.000000000000000000, 0.9510565162951535312, 1.000000000000000000, 0.9510565162951535312, 1.000000000000000000, 0.9510565162951535312, 1.000000000000000000, 0.9510565162951535312, 1.000000000000000000, 0.9510565162951535312, 1.000000000000000000, 0.9510565162951535312, 1.000000000000000000, 0.9510565162951535312, 1.000000000000000000, 0.9510565162951535312, 1.000000000000000000, 0.9510565162951535312, 1.000000000000000000, 0.9510565162951535312, 1.000000000000000000, 0.9510565162951535312, 1.000000000000000000, 0.9510565162951535312, 1.000000000000000000, 0.9510565162951535312, 1.000000000000000000, 0.9510565162951535312, 1.000000000000000000, 0.9510565162951535312, 1.000000000000000000, 0.9510565162951535312, 1.000000000000000000, 0.9510565162951535312, 1.000000000000000000, 0.9510565162951535312, 1.000000000000000000, 0.9510565162951535312, 1.000000000000000000, 0.9510565162951535312, 1.000000000000000000, 0.9510565162951535312, 1.000000000000000000, 0.9510565162951535312, 1.000000000000000000, 0.9510565162951535312, 1.000000000000000000, 0.9510565162951535312, 1.000000000000000000, 0.9510565162951535312, 1.000000000000000000, 0.9510565162951535312, 1.000000000000000000, 0.9510565162951535312, 1.000000000000000000, 0.9510565162951535312, 1.000000000000000000, 0.9510565162951535312, 1.000000000000000000, 0.9510565162951535312, 1.000000000000000000, 0.9510565162951535312, 1.000000000000000000, 0.9510565162951535312, 1.000000000000000000, 0.9510565162951535312, 1.000000000000000000, 0.9510565162951535312, 1.000000000000000000, 0.9510565162951535312, 1.000000000000000000, 0.9510565162951535312, 1.000000000000000000, 0.9510565162951535312, 1.000000000000000000, 0.9510565162951535312, 1.000000000000000000, 0.9510565162951535312, 1.000000000000000000, 0.9510565162951535312, 1.000000000000000000, 0.9510565162951535312, 1.000000000000000000, 0.9510565162951535312, 1.000000000000000000, 0.9510565162951535312, 1.000000000000000000, 0.9510565162951535312, 1.000000000000000000, 0.9510565162951535312, 1.000000000000000000, 0.9510565162951535312, 1.000000000000000000, 0.9510565162951535312, 1.000000000000000000, 0.9510565162951535312, 1.000000000000000000, 0.9510565162951535312, 1.000000000000000000, 0.9510565162951535312, 1.000000000000000000, 0.9510565162951535312, 1.000000000000000000, 0.9510565162951535312, 1.000000000000000000, 0.9510565162951535312, 1.000000000000000000, 0.9510565162951535312, 1.000000000000000000, 0.9510565162951535312, 1.000000000000000000, 0.9510565162951535312, 1.000000000000000000, 0.9510565162951535312, 1.000000000000000000, 0.9510565162951535312, 1.000000000000000000, 0.9510565162951535312, 1.000000000000000000, 0.9510565162951535312, 1.000000000000000000, 0.9510565162951535312, 1.000000000000000000, 0.9510565162951535312, 1.000000000000000000, 0.9510565162951535312, 1.000000000000000000, 0.9510565162951535312, 1.000000000000000000, 0.9510565162951535312, 1.000000000000000000, 0.9510565162951535312, 1.000000000000000000, 0.9510565162951535312, 1.000000000000000000, 0.9510565162951535312, 1.000000000000000000, 0.9510565162951535312, 1.000000000000000000, 0.9510565162951535312, 1.000000000000000000, 0.9510565162951535312, 1.000000000000000000, 0.9510565162951535312, 1.000000000000000000, 0.9510565162951535312, 1.000000000000000000, 0.9510565162951535312, 1.000000000000000000, 0.9510565162951535312, 1.000000000000000000, 0.9510565162951535312, 1.000000000000000000, 0.9510565162951535312, 1.000000000000000000, 0.9510565162951535312, 1.000000000000000000, 0.9510565162951535312, 1.000000000000000000, 0.9510565162951535312, 1.000000000000000000, 0.9510565162951535312, 1.000000000000000000, 0.9510565162951535312, 1.000000000000000000, 0.9510565162951535312, 1.000000000000000000, 0.9510565162951535312, 1.000000000000000000, 0.9510565162951535312, 1.000000000000000000, 0.9510565162951535312, 1.000000000000000000, 0.9510565162951535312, 1.000000000000000000, 0.9510565162951535312, 1.000000000000000000, 0.9510565162951535312, 1.000000000000000000, 0.9510565162951535312, 1.000000000000000000, 0.9510565162951535312, 1.000000000000000000, 0.9510565162951535312, 1.000000000000000000, 0.9510565162951535312, 1.000000000000000000, 0.9510565162951535312, 1.000000000000000000, 0.9510565162951535312, 1.000000000000000000, 0.9510565162951535312, 1.000000000000000000, 0.9510565162951535312, 1.000000000000000000, 0.9510565162951535312, 1.000000000000000000, 0.9510565162951535312, 1.000000000000000000, 0.9510565162951535312, 1.000000000000000000, 0.9510565162951535312, 1.000000000000000000, 0.9510565162951535312, 1.000000000000000000, 0.9510565162951535312, 1.000000000000000000, 0.9510565162951535312, 1.000000000000000000, 0.9510565162951535312, 1.000000000000000000, 0.9510565162951535312, 1.000000000000000000, 0.9510565162951535312, 1.000000000000000000, 0.9510565162951535312, 1.000000000000000000, 0.9510565162951535312, 1.000000000000000000, 0.9510565162951535312, 1.000000000000000000, 0.9510565162951535312, 1.000000000000000000, 0.9510565162951535312, 1.000000000000000000, 0.9510565162951535312, 1.000000000000000000, 0.9510565162951535312, 1.000000000000000000, 0.9510565162951535312, 1.000000000000000000, 0.9510565162951535312, 1.000000000000000000, 0.9510565162951535312, 1.000000000000000000, 0.9510565162951535312, 1.000000000000000000, 0.9510565162951535312, 1.000000000000000000, 0.9510565162951535312, 1.000000000000000000, 0.9510565162951535312, 1.000000000000000000, 0.9510565162951535312, 1.000000000000000000, 0.9510565162951535312, 1.000000000000000000, 0.9510565162951535312, 1.000000000000000000, 0.9510565162951535312, 1.000000000000000000, 0.9510565162951535312, 1.000000000000000000, 0.9510565162951535312, 1.000000000000000000, 0.9510565162951535312, 1.000000000000000000, 0.9510565162951535312, 1.000000000000000000, 0.9510565162951535312, 1.000000000000000000, 0.9510565162951535312, 1.000000000000000000, 0.9510565162951535312, 1.000000000000000000) ) ) 
 REPRESENTATION_ITEM ( '' )  SURFACE ( )  );
#10690 = CARTESIAN_POINT ( 'NONE',  ( 33.58253175000000823, 52.02500000273118985, 10.91162601494192863 ) ) ;
#10691 = CARTESIAN_POINT ( 'NONE',  ( -10.37757302488623701, 19.77500000273117564, 31.93888565452638417 ) ) ;
#10692 = CARTESIAN_POINT ( 'NONE',  ( -33.58253175000000113, 5.275000002731187188, -10.91162601494193218 ) ) ;
#10693 = CARTESIAN_POINT ( 'NONE',  ( 24.20753774853731244, 43.94010416666665719, -13.97622843553633132 ) ) ;
#10694 = CARTESIAN_POINT ( 'NONE',  ( -20.53372385742071771, 26.32850666759063785, 20.47846945139902530 ) ) ;
#10695 = CARTESIAN_POINT ( 'NONE',  ( -28.00173670424535644, 20.30170166574269075, 7.543491769121936308 ) ) ;
#10696 = CARTESIAN_POINT ( 'NONE',  ( 26.29305231718578995, 71.70000000546238539, -19.10302069950538240 ) ) ;
#10697 = CARTESIAN_POINT ( 'NONE',  ( 32.61426705943282656, 52.00000000000002842, 7.648559219946585053 ) ) ;
#10698 = CARTESIAN_POINT ( 'NONE',  ( -20.75514604977248112, 39.42500000273118843, 28.56700777964554661 ) ) ;
#10699 = CARTESIAN_POINT ( 'NONE',  ( -19.06425588902558133, 50.95274333240935505, 19.11951029504797006 ) ) ;
#10700 = CARTESIAN_POINT ( 'NONE',  ( 1.507698388325705758E-15, 13.12499999726881228, -24.62258325217400312 ) ) ;
#10701 = CARTESIAN_POINT ( 'NONE',  ( 3.000384657911015469E-15, 0.000000000000000000, -24.50000000000000000 ) ) ;
#10702 = ORIENTED_EDGE ( 'NONE', *, *, #10286, .F. ) ;
#10703 = EDGE_CURVE ( 'NONE', #4231, #17758, #14024, .T. ) ;
#10704 = CARTESIAN_POINT ( 'NONE',  ( 33.58253175000000823, 48.27500000273119696, 10.91162601494192863 ) ) ;
#10705 = CARTESIAN_POINT ( 'NONE',  ( -13.94119854578936923, 44.51861083425730214, -24.22776226481241224 ) ) ;
#10706 = CARTESIAN_POINT ( 'NONE',  ( -2.162160676586881955E-15, 70.87500000273118417, -35.31076352940723240 ) ) ;
#10707 = ADVANCED_FACE ( 'NONE', ( #6696 ), #15686, .T. ) ;
#10708 = ORIENTED_EDGE ( 'NONE', *, *, #15565, .F. ) ;
#10709 = CARTESIAN_POINT ( 'NONE',  ( -20.75514604977248823, 26.82500000273117280, -28.56700777964554305 ) ) ;
#10710 = CARTESIAN_POINT ( 'NONE',  ( -15.01150461594642138, 22.45572916666666430, -26.00068869287340334 ) ) ;
#10711 = STYLED_ITEM ( 'NONE', ( #17860 ), #22997 ) ;
#10712 = ORIENTED_EDGE ( 'NONE', *, *, #12161, .T. ) ;
#10713 = CARTESIAN_POINT ( 'NONE',  ( 32.50000000000000711, 29.40000000546238823, 10.55989012756945122 ) ) ;
#10714 = CARTESIAN_POINT ( 'NONE',  ( -10.37757302488623701, 61.52500000273120406, 31.93888565452638417 ) ) ;
#10715 = CARTESIAN_POINT ( 'NONE',  ( -28.01184896238304134, 52.96354166666666430, -7.505752307972844761 ) ) ;
#10716 = CARTESIAN_POINT ( 'NONE',  ( 5.779280353836490358E-15, 67.00000000546236834, 32.49999999999999289 ) ) ;
#10717 = CARTESIAN_POINT ( 'NONE',  ( -23.41746824999999887, 8.124999997268817609, -2.867812753649727150E-15 ) ) ;
#10718 = CARTESIAN_POINT ( 'NONE',  ( 27.16883889988624290, 3.925000002731188431, 19.73931689729373673 ) ) ;
#10719 = CARTESIAN_POINT ( 'NONE',  ( 33.58253175000000113, 28.47500000273118204, -10.91162601494193751 ) ) ;
#10720 =( LENGTH_UNIT ( ) NAMED_UNIT ( * ) SI_UNIT ( .MILLI., .METRE. ) );
#10721 = CARTESIAN_POINT ( 'NONE',  ( -20.47846945139866648, 57.82774333240935505, 20.53372385742108008 ) ) ;
#10722 = CARTESIAN_POINT ( 'NONE',  ( -33.58253175000000113, 79.27500000273118985, -10.91162601494193218 ) ) ;
#10723 = CARTESIAN_POINT ( 'NONE',  ( 5.779280353836490358E-15, 65.00000000546236834, 32.49999999999999289 ) ) ;
#10724 = CARTESIAN_POINT ( 'NONE',  ( -20.08610463437157989, 69.69999999999997442, -27.64615127144129758 ) ) ;
#10725 = ADVANCED_BREP_SHAPE_REPRESENTATION ( '', ( #32129, #1376 ), #10174 ) ;
#10726 = CARTESIAN_POINT ( 'NONE',  ( -32.50000000000000000, 18.00000000000000355, 0.000000000000000000 ) ) ;
#10727 = CARTESIAN_POINT ( 'NONE',  ( 26.07999730980490227, 58.11979166666665719, 6.988114217767821046 ) ) ;
#10728 = CARTESIAN_POINT ( 'NONE',  ( 19.82091636218621389, 17.94999999453764161, -14.40073868116559197 ) ) ;
#10729 = CARTESIAN_POINT ( 'NONE',  ( -11.25946833292375793, 79.07500000273121543, 8.180482586598737171 ) ) ;
#10730 = CARTESIAN_POINT ( 'NONE',  ( 24.20753774853731244, 33.62760416666665719, -13.97622843553632599 ) ) ;
#10731 = CARTESIAN_POINT ( 'NONE',  ( -10.37757302488623701, 27.52500000273119696, 31.93888565452638417 ) ) ;
#10732 = CARTESIAN_POINT ( 'NONE',  ( 20.75514604977249178, 73.82500000273121543, 28.56700777964553950 ) ) ;
#10733 = CARTESIAN_POINT ( 'NONE',  ( 33.58253175000000823, 36.27500000273119696, 10.91162601494192863 ) ) ;
#10734 = CARTESIAN_POINT ( 'NONE',  ( 33.58253175000000113, 12.47500000273119447, -10.91162601494193574 ) ) ;
#10735 = DIRECTION ( 'NONE',  ( 0.000000000000000000, 0.000000000000000000, 1.000000000000000000 ) ) ;
#10736 = CARTESIAN_POINT ( 'NONE',  ( 14.01125832528286352, 55.40402750092397355, -24.18731323226246843 ) ) ;
#10737 = CARTESIAN_POINT ( 'NONE',  ( -20.75514604977248823, 68.82500000273118701, -28.56700777964554305 ) ) ;
#10738 = CARTESIAN_POINT ( 'NONE',  ( 26.29305231718579350, 59.30000000546237260, 19.10302069950537529 ) ) ;
#10739 = CARTESIAN_POINT ( 'NONE',  ( -20.08610463437156923, 56.29999999999999716, 27.64615127144130113 ) ) ;
#10740 = DIRECTION ( 'NONE',  ( -0.000000000000000000, -1.000000000000000000, -0.000000000000000000 ) ) ;
#10741 = CARTESIAN_POINT ( 'NONE',  ( -33.58253175000000113, 61.02500000273118985, -10.91162601494193041 ) ) ;
#10742 = CARTESIAN_POINT ( 'NONE',  ( -14.47279130897152122, 10.42499999726881299, 19.92008829642072243 ) ) ;
#10743 = ADVANCED_FACE ( 'NONE', ( #21656 ), #6364, .T. ) ;
#10744 = ORIENTED_EDGE ( 'NONE', *, *, #15171, .F. ) ;
#10745 = CARTESIAN_POINT ( 'NONE',  ( -10.37757302488624411, 72.97500000273120691, -31.93888565452638417 ) ) ;
#10746 = DIRECTION ( 'NONE',  ( 0.000000000000000000, 0.000000000000000000, -1.000000000000000000 ) ) ;
#10747 = AXIS2_PLACEMENT_3D ( 'NONE', #21490, #21328, #26126 ) ;
#10748 = CARTESIAN_POINT ( 'NONE',  ( -7.236395654485757944, 1.224999997268799712, -22.27133577429736988 ) ) ;
#10749 = CARTESIAN_POINT ( 'NONE',  ( -26.09010956794232428, 12.86496500092397710, 6.950374756619732253 ) ) ;
#10750 = ORIENTED_EDGE ( 'NONE', *, *, #8214, .T. ) ;
#10751 = CARTESIAN_POINT ( 'NONE',  ( -33.58253175000000113, 45.02500000273117564, -10.91162601494193218 ) ) ;
#10752 = FACE_OUTER_BOUND ( 'NONE', #5512, .T. ) ;
#10753 = EDGE_LOOP ( 'NONE', ( #26841, #32316, #33359, #26027 ) ) ;
#10754 = CARTESIAN_POINT ( 'NONE',  ( 26.00068869287367335, 44.51302083333331439, 15.01150461594596308 ) ) ;
#10755 = CARTESIAN_POINT ( 'NONE',  ( -12.90513655866680587, 66.99999999999998579, -31.00393344628902881 ) ) ;
#10756 = CARTESIAN_POINT ( 'NONE',  ( 32.50000000000000711, 7.400000005462386454, 10.55989012756945122 ) ) ;
#10757 = CARTESIAN_POINT ( 'NONE',  ( 20.08610463437157279, 27.80000000546238326, -27.64615127144129758 ) ) ;
#10758 = CARTESIAN_POINT ( 'NONE',  ( -15.01150461594642138, 22.45572916666666430, -26.00068869287340334 ) ) ;
#10759 = CARTESIAN_POINT ( 'NONE',  ( 15.14183272437241889, 1.700000000000004396, 20.84094480462498211 ) ) ;
#10760 = CARTESIAN_POINT ( 'NONE',  ( 27.16883889988623935, 8.575000002731202997, -19.73931689729374384 ) ) ;
#10761 = CARTESIAN_POINT ( 'NONE',  ( -20.08610463437157989, 57.70000000000000284, -27.64615127144129758 ) ) ;
#10762 = CARTESIAN_POINT ( 'NONE',  ( 32.50000000000000000, 57.50000000546237544, -3.980102097228898626E-15 ) ) ;
#10763 = CARTESIAN_POINT ( 'NONE',  ( -26.29305231718578995, 30.20000000000000284, 19.10302069950538595 ) ) ;
#10764 = CARTESIAN_POINT ( 'NONE',  ( 7.468012846824281681, 35.19753499907601935, -28.02196122052058058 ) ) ;
#10765 = B_SPLINE_CURVE_WITH_KNOTS ( 'NONE', 3,
 ( #8095, #26292, #10845, #24059, #26460, #18, #26794, #23720, #16338, #20984, #527, #29190, #10506, #3286, #18582, #18913, #13754, #23890, #7926, #13595, #10674, #24225 ),
 .UNSPECIFIED., .F., .F.,
 ( 4, 2, 2, 2, 2, 2, 2, 2, 2, 2, 4 ),
 ( 2.442512830937285584E-16, 0.002730916255965320019, 0.005461832511930396310, 0.008192748767895472600, 0.009558206895878010312, 0.01092366502386054629, 0.01365458127982561651, 0.01638549753579068499, 0.01775095566377321576, 0.01911641379175575001, 0.02184733004772081155 ),
 .UNSPECIFIED. ) ;
#10766 = CARTESIAN_POINT ( 'NONE',  ( -13.91746824999999887, 75.37500000273116996, 0.000000000000000000 ) ) ;
#10767 = CARTESIAN_POINT ( 'NONE',  ( -15.01150461594642316, 46.51822916666666430, -26.00068869287341045 ) ) ;
#10768 = CONTEXT_DEPENDENT_SHAPE_REPRESENTATION ( #28295, #17523 ) ;
#10769 = CARTESIAN_POINT ( 'NONE',  ( 3.980102097228898626E-15, 80.00000000000001421, 32.50000000000000000 ) ) ;
#10770 = CARTESIAN_POINT ( 'NONE',  ( -1.053607264507113999E-13, 64.50000000000000000, 32.50000000000000711 ) ) ;
#10771 = CARTESIAN_POINT ( 'NONE',  ( -32.50000000000000000, 4.099999999999986322, 10.55989012756946366 ) ) ;
#10772 = DIRECTION ( 'NONE',  ( -1.000000000000000000, 0.000000000000000000, 0.000000000000000000 ) ) ;
#10773 = CARTESIAN_POINT ( 'NONE',  ( 19.11951029504797006, 63.84336833240935505, 19.06425588902558133 ) ) ;
#10774 = CARTESIAN_POINT ( 'NONE',  ( 10.37757302488624767, 43.72500000273119269, 31.93888565452638417 ) ) ;
#10775 = CARTESIAN_POINT ( 'NONE',  ( 15.00000000000000000, 73.25000000546239676, -1.836970198721029589E-15 ) ) ;
#10776 = CARTESIAN_POINT ( 'NONE',  ( -27.16883889988624290, 57.17500000273119554, -19.73931689729374028 ) ) ;
#10777 = CARTESIAN_POINT ( 'NONE',  ( -10.37757302488624411, 34.97500000273118559, -31.93888565452638417 ) ) ;
#10778 = CARTESIAN_POINT ( 'NONE',  ( 26.29305231718579350, 24.79999999999999005, 19.10302069950537529 ) ) ;
#10779 = CARTESIAN_POINT ( 'NONE',  ( -19.09188309203694445, 25.74999999999999645, -19.09188309203661049 ) ) ;
#10780 = CARTESIAN_POINT ( 'NONE',  ( -5.147494310547377161, 61.55125428154684641, -32.50000000000002132 ) ) ;
#10781 = CARTESIAN_POINT ( 'NONE',  ( 5.779280353836490358E-15, 23.00000000546237899, 32.49999999999999289 ) ) ;
#10782 = CARTESIAN_POINT ( 'NONE',  ( -10.04305231718578462, 74.40000000000000568, 30.90933677959249337 ) ) ;
#10783 = CARTESIAN_POINT ( 'NONE',  ( 10.37757302488624767, 13.72500000273117671, 31.93888565452638417 ) ) ;
#10784 = DIRECTION ( 'NONE',  ( 0.000000000000000000, -1.000000000000000000, 0.000000000000000000 ) ) ;
#10785 = CARTESIAN_POINT ( 'NONE',  ( 5.779280353836490358E-15, 40.49999999999999289, 32.49999999999999289 ) ) ;
#10786 = CARTESIAN_POINT ( 'NONE',  ( 19.11951029504797006, 15.71836833240935327, 19.06425588902558133 ) ) ;
#10787 = CARTESIAN_POINT ( 'NONE',  ( -20.08610463437156923, 34.80000000546240102, 27.64615127144130113 ) ) ;
#10788 =( BOUNDED_SURFACE ( )  B_SPLINE_SURFACE ( 1, 2, ( 
 ( #7738, #7910, #20966, #31417, #1903, #12380, #22848, #33307, #15304, #30729, #7223, #4655, #20455, #30906, #7400, #17886, #21924, #11613, #30129, #19187, #19354, #10659, #15820, #808, #26274, #32374, #24494, #22261, #14200, #6128, #29966, #1299, #2763, #16945, #21138, #967, #24655, #8870, #19518, #14032, #3559, #19683, #16776, #13868, #18564, #11781, #31579, #11448, #3729, #24333, #32703, #27236, #16612, #9198, #29796, #6300, #27403, #6473, #1128, #13228, #27065, #22095, #23703, #32539, #9039, #14364, #29625, #3892, #24821, #169, #8078, #29007, #5970, #16447, #26899, #11289, #3398, #21768, #32211, #8704, #6969, #28253, #1475, #27914, #30641, #27739, #6632, #25511, #6799, #12290, #7309, #17454, #4397, #22763, #22936, #15047, #17278, #14531, #30298, #4736, #33216, #14871, #33392, #25335, #20198, #25680, #32867, #1813, #4229, #14703, #9715, #7138, #9891, #25161, #28080, #1991, #24992, #1639, #23104, #17619, #20368, #20024, #33568, #4569, #12466, #30817, #17794, #12634, #15217, #2160, #10066, #20546, #17111, #27570, #4058, #11949, #22418, #9364, #19846, #12115, #22587, #33039, #9543, #30470, #10578, #10243, #2851, #23963, #13148, #28422, #12981, #5084, #23622, #13322, #90, #31164, #33748, #4911, #7999, #15569, #26193, #5426, #12810, #28927, #7656, #20723, #26532, #23282, #23455, #29091, #25847, #10406, #10917, #2688, #21056, #31506, #18143, #5595, #15391, #261, #28586 ),
 ( #18483, #31334, #13497, #15738, #15906, #31669, #10748, #18315, #30992, #20885, #26362, #3026, #23795, #21225, #16077, #7826, #28761, #8163, #18653, #7491, #33917, #433, #2337, #17971, #26023, #2514, #5257, #29587, #14326, #21727, #8999, #16244, #8665, #11410, #8497, #21389, #6260, #21557, #27026, #22054, #32172, #19149, #3521, #3687, #29755, #32001, #29260, #11086, #19480, #13994, #6089, #14161, #16571, #930, #6432, #13665, #24455, #18985, #29429, #21886, #32336, #24617, #5932, #8829, #16739, #5764, #16410, #3851, #19313, #1091, #769, #24782, #27197, #11574, #32499, #29929, #27366, #16904, #1260, #31834, #8328, #18817, #26699, #3196, #24129, #595, #26863, #3358, #13828, #24297, #11250, #7101, #17414, #30432, #4019, #1771, #14663, #19646, #6931, #19809, #25123, #22546, #1601, #9504, #11911, #19985, #32997, #27531, #22383, #30088, #27876, #17241, #4360, #14835, #4532, #6594, #25301, #14493, #9679, #4191, #30605, #12251, #22728, #24951, #33177, #1954, #27701, #20161, #17584, #30259, #28045, #9162, #15006, #12428, #9322, #17071, #22220, #6762, #25475, #11740, #1432, #32832, #32667, #12078, #9996, #14799, #9819, #1567, #22863, #28010, #20469, #14972, #30744, #2264, #9468, #25440, #17378, #4325, #20296, #4496, #30921, #25264, #4668, #12566, #12043, #6897, #33671, #12393, #7414, #30571, #10168, #1916, #33321, #17900, #15148, #23209, #7235, #28181, #12738, #17723, #25612 ) ),
 .UNSPECIFIED., .F., .F., .T. ) 
 B_SPLINE_SURFACE_WITH_KNOTS ( ( 2, 2 ),
 ( 3, 2, 2, 2, 2, 2, 2, 2, 2, 2, 2, 2, 2, 2, 2, 2, 2, 2, 2, 2, 2, 2, 2, 2, 2, 2, 2, 2, 2, 2, 2, 2, 2, 2, 2, 2, 2, 2, 2, 2, 2, 2, 2, 2, 2, 2, 2, 2, 2, 2, 2, 2, 2, 2, 2, 2, 2, 2, 2, 2, 2, 2, 2, 2, 2, 2, 2, 2, 2, 2, 2, 2, 2, 2, 2, 2, 2, 2, 2, 2, 2, 2, 2, 2, 2, 2, 2, 2, 2, 2, 3 ),
 ( 0.000000000000000000, 1.000000000000000000 ),
 ( 0.000000000000000000, 0.01111111111111111154, 0.02222222222222222307, 0.03333333333333333287, 0.04444444444444444614, 0.05555555555555555247, 0.06666666666666666574, 0.07777777777777777901, 0.08888888888888889228, 0.1000000000000000056, 0.1111111111111111049, 0.1222222222222222182, 0.1333333333333333315, 0.1444444444444444309, 0.1555555555555555580, 0.1666666666666666574, 0.1777777777777777846, 0.1888888888888888840, 0.2000000000000000111, 0.2111111111111111105, 0.2222222222222222099, 0.2333333333333333370, 0.2444444444444444364, 0.2555555555555555358, 0.2666666666666666630, 0.2777777777777777901, 0.2888888888888888618, 0.2999999999999999889, 0.3111111111111111160, 0.3222222222222222432, 0.3333333333333333148, 0.3444444444444444420, 0.3555555555555555691, 0.3666666666666666408, 0.3777777777777777679, 0.3888888888888888951, 0.4000000000000000222, 0.4111111111111110938, 0.4222222222222222210, 0.4333333333333333481, 0.4444444444444444198, 0.4555555555555555469, 0.4666666666666666741, 0.4777777777777778012, 0.4888888888888888729, 0.5000000000000000000, 0.5111111111111110716, 0.5222222222222222543, 0.5333333333333333259, 0.5444444444444443976, 0.5555555555555555802, 0.5666666666666666519, 0.5777777777777777235, 0.5888888888888889062, 0.5999999999999999778, 0.6111111111111111605, 0.6222222222222222321, 0.6333333333333333037, 0.6444444444444444864, 0.6555555555555555580, 0.6666666666666666297, 0.6777777777777778123, 0.6888888888888888840, 0.6999999999999999556, 0.7111111111111111382, 0.7222222222222222099, 0.7333333333333332815, 0.7444444444444444642, 0.7555555555555555358, 0.7666666666666667185, 0.7777777777777777901, 0.7888888888888888618, 0.8000000000000000444, 0.8111111111111111160, 0.8222222222222221877, 0.8333333333333333703, 0.8444444444444444420, 0.8555555555555555136, 0.8666666666666666963, 0.8777777777777777679, 0.8888888888888888395, 0.9000000000000000222, 0.9111111111111110938, 0.9222222222222222765, 0.9333333333333333481, 0.9444444444444444198, 0.9555555555555556024, 0.9666666666666666741, 0.9777777777777777457, 0.9888888888888889284, 1.000000000000000000 ),
 .UNSPECIFIED. ) 
 GEOMETRIC_REPRESENTATION_ITEM ( )  RATIONAL_B_SPLINE_SURFACE ( (
 ( 1.000000000000000000, 0.9510565162951535312, 1.000000000000000000, 0.9510565162951535312, 1.000000000000000000, 0.9510565162951535312, 1.000000000000000000, 0.9510565162951535312, 1.000000000000000000, 0.9510565162951535312, 1.000000000000000000, 0.9510565162951535312, 1.000000000000000000, 0.9510565162951535312, 1.000000000000000000, 0.9510565162951535312, 1.000000000000000000, 0.9510565162951535312, 1.000000000000000000, 0.9510565162951535312, 1.000000000000000000, 0.9510565162951535312, 1.000000000000000000, 0.9510565162951535312, 1.000000000000000000, 0.9510565162951535312, 1.000000000000000000, 0.9510565162951535312, 1.000000000000000000, 0.9510565162951535312, 1.000000000000000000, 0.9510565162951535312, 1.000000000000000000, 0.9510565162951535312, 1.000000000000000000, 0.9510565162951535312, 1.000000000000000000, 0.9510565162951535312, 1.000000000000000000, 0.9510565162951535312, 1.000000000000000000, 0.9510565162951535312, 1.000000000000000000, 0.9510565162951535312, 1.000000000000000000, 0.9510565162951535312, 1.000000000000000000, 0.9510565162951535312, 1.000000000000000000, 0.9510565162951535312, 1.000000000000000000, 0.9510565162951535312, 1.000000000000000000, 0.9510565162951535312, 1.000000000000000000, 0.9510565162951535312, 1.000000000000000000, 0.9510565162951535312, 1.000000000000000000, 0.9510565162951535312, 1.000000000000000000, 0.9510565162951535312, 1.000000000000000000, 0.9510565162951535312, 1.000000000000000000, 0.9510565162951535312, 1.000000000000000000, 0.9510565162951535312, 1.000000000000000000, 0.9510565162951535312, 1.000000000000000000, 0.9510565162951535312, 1.000000000000000000, 0.9510565162951535312, 1.000000000000000000, 0.9510565162951535312, 1.000000000000000000, 0.9510565162951535312, 1.000000000000000000, 0.9510565162951535312, 1.000000000000000000, 0.9510565162951535312, 1.000000000000000000, 0.9510565162951535312, 1.000000000000000000, 0.9510565162951535312, 1.000000000000000000, 0.9510565162951535312, 1.000000000000000000, 0.9510565162951535312, 1.000000000000000000, 0.9510565162951535312, 1.000000000000000000, 0.9510565162951535312, 1.000000000000000000, 0.9510565162951535312, 1.000000000000000000, 0.9510565162951535312, 1.000000000000000000, 0.9510565162951535312, 1.000000000000000000, 0.9510565162951535312, 1.000000000000000000, 0.9510565162951535312, 1.000000000000000000, 0.9510565162951535312, 1.000000000000000000, 0.9510565162951535312, 1.000000000000000000, 0.9510565162951535312, 1.000000000000000000, 0.9510565162951535312, 1.000000000000000000, 0.9510565162951535312, 1.000000000000000000, 0.9510565162951535312, 1.000000000000000000, 0.9510565162951535312, 1.000000000000000000, 0.9510565162951535312, 1.000000000000000000, 0.9510565162951535312, 1.000000000000000000, 0.9510565162951535312, 1.000000000000000000, 0.9510565162951535312, 1.000000000000000000, 0.9510565162951535312, 1.000000000000000000, 0.9510565162951535312, 1.000000000000000000, 0.9510565162951535312, 1.000000000000000000, 0.9510565162951535312, 1.000000000000000000, 0.9510565162951535312, 1.000000000000000000, 0.9510565162951535312, 1.000000000000000000, 0.9510565162951535312, 1.000000000000000000, 0.9510565162951535312, 1.000000000000000000, 0.9510565162951535312, 1.000000000000000000, 0.9510565162951535312, 1.000000000000000000, 0.9510565162951535312, 1.000000000000000000, 0.9510565162951535312, 1.000000000000000000, 0.9510565162951535312, 1.000000000000000000, 0.9510565162951535312, 1.000000000000000000, 0.9510565162951535312, 1.000000000000000000, 0.9510565162951535312, 1.000000000000000000, 0.9510565162951535312, 1.000000000000000000, 0.9510565162951535312, 1.000000000000000000, 0.9510565162951535312, 1.000000000000000000, 0.9510565162951535312, 1.000000000000000000, 0.9510565162951535312, 1.000000000000000000, 0.9510565162951535312, 1.000000000000000000, 0.9510565162951535312, 1.000000000000000000, 0.9510565162951535312, 1.000000000000000000, 0.9510565162951535312, 1.000000000000000000, 0.9510565162951535312, 1.000000000000000000, 0.9510565162951535312, 1.000000000000000000),
 ( 1.000000000000000000, 0.9510565162951535312, 1.000000000000000000, 0.9510565162951535312, 1.000000000000000000, 0.9510565162951535312, 1.000000000000000000, 0.9510565162951535312, 1.000000000000000000, 0.9510565162951535312, 1.000000000000000000, 0.9510565162951535312, 1.000000000000000000, 0.9510565162951535312, 1.000000000000000000, 0.9510565162951535312, 1.000000000000000000, 0.9510565162951535312, 1.000000000000000000, 0.9510565162951535312, 1.000000000000000000, 0.9510565162951535312, 1.000000000000000000, 0.9510565162951535312, 1.000000000000000000, 0.9510565162951535312, 1.000000000000000000, 0.9510565162951535312, 1.000000000000000000, 0.9510565162951535312, 1.000000000000000000, 0.9510565162951535312, 1.000000000000000000, 0.9510565162951535312, 1.000000000000000000, 0.9510565162951535312, 1.000000000000000000, 0.9510565162951535312, 1.000000000000000000, 0.9510565162951535312, 1.000000000000000000, 0.9510565162951535312, 1.000000000000000000, 0.9510565162951535312, 1.000000000000000000, 0.9510565162951535312, 1.000000000000000000, 0.9510565162951535312, 1.000000000000000000, 0.9510565162951535312, 1.000000000000000000, 0.9510565162951535312, 1.000000000000000000, 0.9510565162951535312, 1.000000000000000000, 0.9510565162951535312, 1.000000000000000000, 0.9510565162951535312, 1.000000000000000000, 0.9510565162951535312, 1.000000000000000000, 0.9510565162951535312, 1.000000000000000000, 0.9510565162951535312, 1.000000000000000000, 0.9510565162951535312, 1.000000000000000000, 0.9510565162951535312, 1.000000000000000000, 0.9510565162951535312, 1.000000000000000000, 0.9510565162951535312, 1.000000000000000000, 0.9510565162951535312, 1.000000000000000000, 0.9510565162951535312, 1.000000000000000000, 0.9510565162951535312, 1.000000000000000000, 0.9510565162951535312, 1.000000000000000000, 0.9510565162951535312, 1.000000000000000000, 0.9510565162951535312, 1.000000000000000000, 0.9510565162951535312, 1.000000000000000000, 0.9510565162951535312, 1.000000000000000000, 0.9510565162951535312, 1.000000000000000000, 0.9510565162951535312, 1.000000000000000000, 0.9510565162951535312, 1.000000000000000000, 0.9510565162951535312, 1.000000000000000000, 0.9510565162951535312, 1.000000000000000000, 0.9510565162951535312, 1.000000000000000000, 0.9510565162951535312, 1.000000000000000000, 0.9510565162951535312, 1.000000000000000000, 0.9510565162951535312, 1.000000000000000000, 0.9510565162951535312, 1.000000000000000000, 0.9510565162951535312, 1.000000000000000000, 0.9510565162951535312, 1.000000000000000000, 0.9510565162951535312, 1.000000000000000000, 0.9510565162951535312, 1.000000000000000000, 0.9510565162951535312, 1.000000000000000000, 0.9510565162951535312, 1.000000000000000000, 0.9510565162951535312, 1.000000000000000000, 0.9510565162951535312, 1.000000000000000000, 0.9510565162951535312, 1.000000000000000000, 0.9510565162951535312, 1.000000000000000000, 0.9510565162951535312, 1.000000000000000000, 0.9510565162951535312, 1.000000000000000000, 0.9510565162951535312, 1.000000000000000000, 0.9510565162951535312, 1.000000000000000000, 0.9510565162951535312, 1.000000000000000000, 0.9510565162951535312, 1.000000000000000000, 0.9510565162951535312, 1.000000000000000000, 0.9510565162951535312, 1.000000000000000000, 0.9510565162951535312, 1.000000000000000000, 0.9510565162951535312, 1.000000000000000000, 0.9510565162951535312, 1.000000000000000000, 0.9510565162951535312, 1.000000000000000000, 0.9510565162951535312, 1.000000000000000000, 0.9510565162951535312, 1.000000000000000000, 0.9510565162951535312, 1.000000000000000000, 0.9510565162951535312, 1.000000000000000000, 0.9510565162951535312, 1.000000000000000000, 0.9510565162951535312, 1.000000000000000000, 0.9510565162951535312, 1.000000000000000000, 0.9510565162951535312, 1.000000000000000000, 0.9510565162951535312, 1.000000000000000000, 0.9510565162951535312, 1.000000000000000000, 0.9510565162951535312, 1.000000000000000000, 0.9510565162951535312, 1.000000000000000000, 0.9510565162951535312, 1.000000000000000000, 0.9510565162951535312, 1.000000000000000000) ) ) 
 REPRESENTATION_ITEM ( '' )  SURFACE ( )  );
#10789 = CARTESIAN_POINT ( 'NONE',  ( 32.50000000000000000, 11.00000000000001066, -3.980102097228898626E-15 ) ) ;
#10790 = CARTESIAN_POINT ( 'NONE',  ( 20.75514604977249178, 19.82500000273119412, 28.56700777964553950 ) ) ;
#10791 = CARTESIAN_POINT ( 'NONE',  ( -6.988114217768288228, 43.22395833333332860, -26.07999730980477437 ) ) ;
#10792 = ORIENTED_EDGE ( 'NONE', *, *, #2764, .F. ) ;
#10793 = CARTESIAN_POINT ( 'NONE',  ( -27.16883889988623935, 61.32500000273120833, 19.73931689729374739 ) ) ;
#10794 = ORIENTED_EDGE ( 'NONE', *, *, #4749, .T. ) ;
#10795 = CARTESIAN_POINT ( 'NONE',  ( -26.00068869287368756, 15.29427083333332504, -15.01150461594595775 ) ) ;
#10796 = CARTESIAN_POINT ( 'NONE',  ( -14.97647472619946285, 13.58111083425730925, -26.02091320914851025 ) ) ;
#10797 = CARTESIAN_POINT ( 'NONE',  ( 20.75514604977249178, 7.825000002731194115, 28.56700777964553950 ) ) ;
#10798 = EDGE_LOOP ( 'NONE', ( #23034, #23287, #13026, #15178 ) ) ;
#10799 = CARTESIAN_POINT ( 'NONE',  ( 5.779280353836490358E-15, 44.49999999999999289, 32.49999999999999289 ) ) ;
#10800 = CARTESIAN_POINT ( 'NONE',  ( 33.58253175000000113, 26.47500000273118559, -10.91162601494193751 ) ) ;
#10801 = CARTESIAN_POINT ( 'NONE',  ( -20.08610463437156923, 34.80000000546240102, 27.64615127144130113 ) ) ;
#10802 = CARTESIAN_POINT ( 'NONE',  ( 12.13525491562421088, 72.80000000000002558, 8.816778784387095058 ) ) ;
#10803 = DIRECTION ( 'NONE',  ( -1.224646799147353454E-16, 1.000000000000000000, -0.000000000000000000 ) ) ;
#10804 = CARTESIAN_POINT ( 'NONE',  ( 1.555960095263670572E-15, 6.499999999999994671, -24.50000000000000000 ) ) ;
#10805 = CARTESIAN_POINT ( 'NONE',  ( 20.75514604977248467, 40.67500000273116711, -28.56700777964554305 ) ) ;
#10806 = AXIS2_PLACEMENT_3D ( 'NONE', #13993, #11409, #10746 ) ;
#10807 = CARTESIAN_POINT ( 'NONE',  ( 32.50000000000000000, 21.00000000000000355, -3.980102097228898626E-15 ) ) ;
#10808 = CARTESIAN_POINT ( 'NONE',  ( 26.29305231718578995, 21.19999999999999574, -19.10302069950538240 ) ) ;
#10809 = CARTESIAN_POINT ( 'NONE',  ( -7.570916362186215665, 5.399999999999987921, 23.30088464923126423 ) ) ;
#10810 = CARTESIAN_POINT ( 'NONE',  ( -33.58253175000000113, 69.02500000273118985, -10.91162601494193218 ) ) ;
#10811 = CARTESIAN_POINT ( 'NONE',  ( -21.25115026575266697, 67.00000000000004263, 25.10892607490235306 ) ) ;
#10812 = CARTESIAN_POINT ( 'NONE',  ( -3.278034869283648511, 74.00000000000002842, -14.32477225908124829 ) ) ;
#10813 = CARTESIAN_POINT ( 'NONE',  ( -10.37757302488624411, 52.97500000273119980, -31.93888565452638417 ) ) ;
#10814 = CARTESIAN_POINT ( 'NONE',  ( -14.47279130897151767, 3.324999997268803131, -19.92008829642072598 ) ) ;
#10815 = CARTESIAN_POINT ( 'NONE',  ( 26.29305231718579350, 7.300000005462381480, 19.10302069950537529 ) ) ;
#10816 = CARTESIAN_POINT ( 'NONE',  ( 33.58253175000000113, 10.12500000273119838, -4.112674001490185761E-15 ) ) ;
#10817 = CARTESIAN_POINT ( 'NONE',  ( -24.22776226481240514, 26.47173583425730925, 13.94119854578937812 ) ) ;
#10818 = CARTESIAN_POINT ( 'NONE',  ( 7.689115195225237898, 67.00000000000000000, -32.34176759466016904 ) ) ;
#10819 = CARTESIAN_POINT ( 'NONE',  ( 2.376701315729479624, 51.99999999999999289, 33.34874525913693333 ) ) ;
#10820 = CARTESIAN_POINT ( 'NONE',  ( -10.37757302488624411, 36.72500000273119980, -31.93888565452638417 ) ) ;
#10821 = CARTESIAN_POINT ( 'NONE',  ( -32.50000000000000000, 18.60000000546238397, 10.55989012756946366 ) ) ;
#10822 = CARTESIAN_POINT ( 'NONE',  ( 27.16883889988623935, 52.57500000273117280, -19.73931689729374384 ) ) ;
#10823 = CARTESIAN_POINT ( 'NONE',  ( -4.300734207923759378, 78.47500000273116427, -13.23629886949340495 ) ) ;
#10824 = CARTESIAN_POINT ( 'NONE',  ( 15.04653450569339945, 43.36159749907602645, 25.98046417659831775 ) ) ;
#10825 = CARTESIAN_POINT ( 'NONE',  ( 32.50000000000000000, 51.50000000546238255, -3.980102097228898626E-15 ) ) ;
#10826 = CARTESIAN_POINT ( 'NONE',  ( 13.91746824999999887, 74.37500000273116996, -1.704398294459741270E-15 ) ) ;
#10827 = CARTESIAN_POINT ( 'NONE',  ( -26.07999730980477437, 14.86458333333333037, 6.988114217768305103 ) ) ;
#10828 = AXIS2_PLACEMENT_3D ( 'NONE', #18026, #22817, #15445 ) ;
#10829 = CARTESIAN_POINT ( 'NONE',  ( 26.29305231718578995, 67.70000000546238539, -19.10302069950538240 ) ) ;
#10830 = CARTESIAN_POINT ( 'NONE',  ( -26.00068869287340334, 21.59635416666666785, 15.01150461594643382 ) ) ;
#10831 = CARTESIAN_POINT ( 'NONE',  ( 20.75514604977248467, 28.67500000273117777, -28.56700777964554305 ) ) ;
#10832 = CARTESIAN_POINT ( 'NONE',  ( -14.47279130897151767, 11.82499999726882578, -19.92008829642072598 ) ) ;
#10833 = ORIENTED_EDGE ( 'NONE', *, *, #9249, .T. ) ;
#10834 = CARTESIAN_POINT ( 'NONE',  ( 20.47846945139902530, 39.21913166759063785, 20.53372385742071771 ) ) ;
#10835 = CARTESIAN_POINT ( 'NONE',  ( -32.50000000000000000, 14.60000000546239107, 10.55989012756946366 ) ) ;
#10836 = ADVANCED_FACE ( 'NONE', ( #1369 ), #27466, .T. ) ;
#10837 = CARTESIAN_POINT ( 'NONE',  ( -20.50609665441004736, 53.25000000000000000, -20.50609665440969565 ) ) ;
#10838 = CARTESIAN_POINT ( 'NONE',  ( -11.54700538379251995, 96.00000000000002842, -19.99999999999999645 ) ) ;
#10839 = CARTESIAN_POINT ( 'NONE',  ( -20.75514604977248112, 51.67500000273117422, 28.56700777964554661 ) ) ;
#10840 = CARTESIAN_POINT ( 'NONE',  ( 32.50000000000000000, 57.50000000546237544, -3.980102097228898626E-15 ) ) ;
#10841 = CARTESIAN_POINT ( 'NONE',  ( 13.91746824999999887, 76.37500000273116996, -1.704398294459741270E-15 ) ) ;
#10842 = CARTESIAN_POINT ( 'NONE',  ( -20.75514604977248112, 37.42500000273118843, 28.56700777964554661 ) ) ;
#10843 = CARTESIAN_POINT ( 'NONE',  ( 32.50000000000000000, 55.09999999999997300, -10.55989012756945833 ) ) ;
#10844 = CARTESIAN_POINT ( 'NONE',  ( -20.75514604977248823, 65.07500000273118701, -28.56700777964554305 ) ) ;
#10845 = CARTESIAN_POINT ( 'NONE',  ( 13.47594703999181043, 74.00000000000000000, -3.594779225894267682 ) ) ;
#10846 = ADVANCED_FACE ( 'NONE', ( #11186 ), #3456, .T. ) ;
#10847 = CARTESIAN_POINT ( 'NONE',  ( 10.37757302488624056, 56.52500000273118275, -31.93888565452638417 ) ) ;
#10848 = EDGE_CURVE ( 'NONE', #23926, #32333, #6467, .T. ) ;
#10849 = CARTESIAN_POINT ( 'NONE',  ( 26.00068869287341045, 23.31510416666666430, -15.01150461594642493 ) ) ;
#10850 = CARTESIAN_POINT ( 'NONE',  ( 26.29305231718579350, 38.80000000000000426, 19.10302069950537529 ) ) ;
#10851 = CARTESIAN_POINT ( 'NONE',  ( -23.41746824999999887, 7.624999997268816720, -2.867812753649727150E-15 ) ) ;
#10852 = CARTESIAN_POINT ( 'NONE',  ( -33.58253175000000113, 11.27500000273117031, -10.91162601494193218 ) ) ;
#10853 = DIRECTION ( 'NONE',  ( 0.000000000000000000, 0.000000000000000000, 1.000000000000000000 ) ) ;
#10854 = CARTESIAN_POINT ( 'NONE',  ( 24.18731323226221974, 32.18972249907602645, -14.01125832528328985 ) ) ;
#10855 = CYLINDRICAL_SURFACE ( 'NONE', #26495, 15.00000000000000000 ) ;
#10856 = CARTESIAN_POINT ( 'NONE',  ( 27.16883889988624290, 70.17500000273119554, 19.73931689729373673 ) ) ;
#10857 = DIRECTION ( 'NONE',  ( 0.000000000000000000, 0.000000000000000000, -1.000000000000000000 ) ) ;
#10858 = CARTESIAN_POINT ( 'NONE',  ( -20.75514604977248112, 67.67500000273116711, 28.56700777964554661 ) ) ;
#10859 = ORIENTED_EDGE ( 'NONE', *, *, #12067, .T. ) ;
#10860 = CARTESIAN_POINT ( 'NONE',  ( 23.41746825000000243, 19.02499999726880375, 7.608796670333735079 ) ) ;
#10861 = VECTOR ( 'NONE', #19014, 1000.000000000000000 ) ;
#10862 = CARTESIAN_POINT ( 'NONE',  ( -24.20753774853756823, 63.41927083333333570, -13.97622843553588723 ) ) ;
#10863 = CARTESIAN_POINT ( 'NONE',  ( -2.162160676586881955E-15, 54.62500000273116996, -35.31076352940723240 ) ) ;
#10864 = CARTESIAN_POINT ( 'NONE',  ( -2.162160676586881955E-15, 14.87500000273120193, -35.31076352940723240 ) ) ;
#10865 = CARTESIAN_POINT ( 'NONE',  ( 20.75514604977248467, 2.675000002731181770, -28.56700777964554305 ) ) ;
#10866 = CARTESIAN_POINT ( 'NONE',  ( 6.988114217767829928, 43.51041666666666430, -26.07999730980489872 ) ) ;
#10867 = CARTESIAN_POINT ( 'NONE',  ( 15.04653450569292872, 31.34152750092398421, -25.98046417659857710 ) ) ;
#10868 = CARTESIAN_POINT ( 'NONE',  ( -30.02300923189239867, 17.00743083240935860, 0.04044903255044988294 ) ) ;
#10869 = CARTESIAN_POINT ( 'NONE',  ( 32.50000000000000711, 75.40000000546240244, 10.55989012756945122 ) ) ;
#10870 = CARTESIAN_POINT ( 'NONE',  ( -32.50000000000000000, 56.60000000546236976, 10.55989012756946366 ) ) ;
#10871 = CARTESIAN_POINT ( 'NONE',  ( 33.58253175000000823, 38.02500000273117564, 10.91162601494192685 ) ) ;
#10872 = CARTESIAN_POINT ( 'NONE',  ( 19.11951029504797006, 46.65586833240934794, 19.06425588902558133 ) ) ;
#10873 = CARTESIAN_POINT ( 'NONE',  ( -7.236395654485757944, 13.22499999726881015, -22.27133577429736988 ) ) ;
#10874 = LINE ( 'NONE', #33873, #22682 ) ;
#10875 = ORIENTED_EDGE ( 'NONE', *, *, #19034, .F. ) ;
#10876 = CARTESIAN_POINT ( 'NONE',  ( -27.16883889988623935, 45.57500000273119412, 19.73931689729374739 ) ) ;
#10877 = CARTESIAN_POINT ( 'NONE',  ( 9.270509831248425314, 76.70000000000001705, 12.75976212528059683 ) ) ;
#10878 = CARTESIAN_POINT ( 'NONE',  ( -19.11951029504763611, 46.95350666759064495, 19.06425588902592239 ) ) ;
#10879 = CARTESIAN_POINT ( 'NONE',  ( 20.75514604977249178, 68.07500000273118701, 28.56700777964553950 ) ) ;
#10880 = ORIENTED_EDGE ( 'NONE', *, *, #7358, .T. ) ;
#10881 = CARTESIAN_POINT ( 'NONE',  ( -27.16883889988624290, 20.92500000273118843, -19.73931689729374028 ) ) ;
#10882 = CARTESIAN_POINT ( 'NONE',  ( -26.00068869287340334, 25.03385416666666785, 15.01150461594643382 ) ) ;
#10883 = VERTEX_POINT ( 'NONE', #11507 ) ;
#10884 = CARTESIAN_POINT ( 'NONE',  ( -3.880418787951137816, 2.301254276084479411, -24.49999999999999645 ) ) ;
#10885 = CARTESIAN_POINT ( 'NONE',  ( 33.58253175000000113, 52.22500000273117848, -10.91162601494193751 ) ) ;
#10886 = CARTESIAN_POINT ( 'NONE',  ( 7.505752307973351023, 44.94270833333332860, 28.01184896238290278 ) ) ;
#10887 =( BOUNDED_CURVE ( )  B_SPLINE_CURVE ( 2, ( #27365, #24950, #12077, #27196, #30256, #29928, #22053, #25300, #9503, #14325, #6930, #25122, #19984 ),
 .UNSPECIFIED., .F., .F. ) 
 B_SPLINE_CURVE_WITH_KNOTS ( ( 3, 2, 2, 2, 2, 2, 3 ),
 ( 0.8012820512820513219, 0.8025641025641025994, 0.8051282051282051544, 0.8076923076923077094, 0.8102564102564102644, 0.8128205128205128194, 0.8141025641025640969 ),
 .UNSPECIFIED. ) 
 CURVE ( )  GEOMETRIC_REPRESENTATION_ITEM ( )  RATIONAL_B_SPLINE_CURVE ( ( 0.9755282581475768211, 0.9755282581475768211, 1.000000000000000000, 0.9510565162951535312, 1.000000000000000000, 0.9510565162951535312, 1.000000000000000000, 0.9510565162951535312, 1.000000000000000000, 0.9510565162951535312, 1.000000000000000000, 0.9755282581475768211, 0.9755282581475768211 ) ) 
 REPRESENTATION_ITEM ( '' )  );
#10888 = CARTESIAN_POINT ( 'NONE',  ( 32.50000000000000000, 17.60000000546238397, -10.55989012756945833 ) ) ;
#10889 = CARTESIAN_POINT ( 'NONE',  ( -24.50000000000000711, 6.849999994537629533, 7.960532557706201828 ) ) ;
#10890 = CARTESIAN_POINT ( 'NONE',  ( 23.41746824999999887, 9.024999997268826846, 7.608796670333735079 ) ) ;
#10891 =( BOUNDED_CURVE ( )  B_SPLINE_CURVE ( 2, ( #7984, #2840, #26350, #7647, #23273, #15728, #31494, #5072, #31657, #17962, #13309, #13136, #5246 ),
 .UNSPECIFIED., .F., .F. ) 
 B_SPLINE_CURVE_WITH_KNOTS ( ( 3, 2, 2, 2, 2, 2, 3 ),
 ( 0.3611111111111111049, 0.3666666666666666408, 0.3777777777777777679, 0.3888888888888888951, 0.4000000000000000222, 0.4111111111111110938, 0.4166666666666666852 ),
 .UNSPECIFIED. ) 
 CURVE ( )  GEOMETRIC_REPRESENTATION_ITEM ( )  RATIONAL_B_SPLINE_CURVE ( ( 0.9755282581475768211, 0.9755282581475768211, 1.000000000000000000, 0.9510565162951535312, 1.000000000000000000, 0.9510565162951535312, 1.000000000000000000, 0.9510565162951535312, 1.000000000000000000, 0.9510565162951535312, 1.000000000000000000, 0.9755282581475765991, 0.9755282581475767101 ) ) 
 REPRESENTATION_ITEM ( '' )  );
#10892 = CARTESIAN_POINT ( 'NONE',  ( 6.486482029760649416E-15, 29.87500000273119838, 35.31076352940723240 ) ) ;
#10893 = CARTESIAN_POINT ( 'NONE',  ( -20.53372385742107653, 62.12461833240934794, -20.47846945139867003 ) ) ;
#10894 = CARTESIAN_POINT ( 'NONE',  ( -19.82091636218621034, 14.80000000000000782, -14.40073868116559552 ) ) ;
#10895 = CARTESIAN_POINT ( 'NONE',  ( 13.91746824999999532, 77.97500000273119269, -4.522059556121118540 ) ) ;
#10896 = CARTESIAN_POINT ( 'NONE',  ( -32.50000000000000000, 69.90000000000000568, -10.55989012756945300 ) ) ;
#10897 = CARTESIAN_POINT ( 'NONE',  ( -32.50000000000000000, 9.899999999999991473, -10.55989012756945478 ) ) ;
#10898 = CARTESIAN_POINT ( 'NONE',  ( -6.988114217767819270, 58.97916666666666430, 26.07999730980490583 ) ) ;
#10899 = CARTESIAN_POINT ( 'NONE',  ( 24.50000000000000000, 19.74999999453763877, 0.000000000000000000 ) ) ;
#10900 = CARTESIAN_POINT ( 'NONE',  ( 11.25946833292375793, 74.07500000273120122, -8.180482586598735395 ) ) ;
#10901 = CARTESIAN_POINT ( 'NONE',  ( -2.428612866367529427E-13, 33.05468750000000000, -27.95245687107222921 ) ) ;
#10902 = EDGE_CURVE ( 'NONE', #8956, #12338, #24391, .T. ) ;
#10903 = CARTESIAN_POINT ( 'NONE',  ( 33.58253175000000113, 24.22500000273119625, -10.91162601494193751 ) ) ;
#10904 = CARTESIAN_POINT ( 'NONE',  ( -2.162160676586881955E-15, 70.62500000273118417, -35.31076352940723240 ) ) ;
#10905 = CARTESIAN_POINT ( 'NONE',  ( 27.16883889988623935, 34.57500000273118701, -19.73931689729374384 ) ) ;
#10906 = CARTESIAN_POINT ( 'NONE',  ( -10.37757302488624411, 16.97500000273119269, -31.93888565452638417 ) ) ;
#10907 = CARTESIAN_POINT ( 'NONE',  ( -7.025853678916393008, 56.97954833425730925, 26.06988505166735592 ) ) ;
#10908 = CARTESIAN_POINT ( 'NONE',  ( -10.37757302488624411, 70.72500000273119269, -31.93888565452638417 ) ) ;
#10909 = CARTESIAN_POINT ( 'NONE',  ( 32.50000000000000000, 3.500000005462383434, -3.980102097228898626E-15 ) ) ;
#10910 = CARTESIAN_POINT ( 'NONE',  ( 26.29305231718578995, 51.20000000000000995, -19.10302069950538240 ) ) ;
#10911 = CARTESIAN_POINT ( 'NONE',  ( 3.469446951953614189E-15, -45.00000000000000000, 0.000000000000000000 ) ) ;
#10912 = CARTESIAN_POINT ( 'NONE',  ( -10.37757302488623701, 59.52500000273119696, 31.93888565452638417 ) ) ;
#10913 = CARTESIAN_POINT ( 'NONE',  ( -14.47279130897151589, 15.82499999726881335, -19.92008829642072598 ) ) ;
#10914 = ORIENTED_EDGE ( 'NONE', *, *, #19531, .F. ) ;
#10915 = CARTESIAN_POINT ( 'NONE',  ( 33.58253175000000823, 66.27500000273118985, 10.91162601494192863 ) ) ;
#10916 = CARTESIAN_POINT ( 'NONE',  ( 10.37757302488624056, 2.525000002731203619, -31.93888565452638417 ) ) ;
#10917 = CARTESIAN_POINT ( 'NONE',  ( -18.94512977948576093, 18.32499999726880446, 13.76444248337722698 ) ) ;
#10918 = CARTESIAN_POINT ( 'NONE',  ( 26.09010956794232428, 21.45871500092397355, -6.950374756619718042 ) ) ;
#10919 = EDGE_LOOP ( 'NONE', ( #30691, #23566, #32455, #26359 ) ) ;
#10920 = CARTESIAN_POINT ( 'NONE',  ( 33.58253175000000113, 34.22500000273117848, -10.91162601494193751 ) ) ;
#10921 = CARTESIAN_POINT ( 'NONE',  ( -32.50000000000000000, 42.50000000546238965, 0.000000000000000000 ) ) ;
#10922 = ORIENTED_EDGE ( 'NONE', *, *, #19623, .T. ) ;
#10923 = CARTESIAN_POINT ( 'NONE',  ( -26.00068869287368756, 46.23177083333331439, -15.01150461594595775 ) ) ;
#10924 = CARTESIAN_POINT ( 'NONE',  ( -4.223320258572821363E-15, 78.75000000546238255, 15.00000000000000355 ) ) ;
#10925 = CARTESIAN_POINT ( 'NONE',  ( 20.50609665440969565, 19.73437500000000000, -20.50609665441004736 ) ) ;
#10926 = CARTESIAN_POINT ( 'NONE',  ( 23.41746824999999887, 18.62499999726882649, 0.000000000000000000 ) ) ;
#10927 = CARTESIAN_POINT ( 'NONE',  ( -10.37757302488624411, 10.97500000273118914, -31.93888565452638417 ) ) ;
#10928 = CARTESIAN_POINT ( 'NONE',  ( 32.50000000000000711, 58.90000000000000568, 10.55989012756945122 ) ) ;
#10929 = CARTESIAN_POINT ( 'NONE',  ( 13.91746824999999887, 77.87500000273116996, -1.704398294459741270E-15 ) ) ;
#10930 = DIRECTION ( 'NONE',  ( 0.000000000000000000, 0.000000000000000000, 1.000000000000000000 ) ) ;
#10931 = CARTESIAN_POINT ( 'NONE',  ( -15.04653450569338524, 38.20534749907601935, -25.98046417659831775 ) ) ;
#10932 = CARTESIAN_POINT ( 'NONE',  ( -8.960552108402742093E-16, 76.87500000273115575, -14.63369212191046387 ) ) ;
#10933 = CARTESIAN_POINT ( 'NONE',  ( -30.02300923189239867, 49.38281249999999289, 2.654126918244514854E-13 ) ) ;
#10934 = DIRECTION ( 'NONE',  ( -1.000000000000000000, -1.224646799147353454E-16, 0.000000000000000000 ) ) ;
#10935 = FACE_OUTER_BOUND ( 'NONE', #14921, .T. ) ;
#10936 = CARTESIAN_POINT ( 'NONE',  ( -27.16883889988624290, 79.17500000273119554, -19.73931689729374028 ) ) ;
#10937 = CARTESIAN_POINT ( 'NONE',  ( 40.00000000000000000, 52.00000000000000711, 23.09401076758503990 ) ) ;
#10938 = EDGE_CURVE ( 'NONE', #4399, #20157, #28813, .T. ) ;
#10939 = CARTESIAN_POINT ( 'NONE',  ( -24.22776226481266448, 58.54388916574269075, -13.94119854578892514 ) ) ;
#10940 = CARTESIAN_POINT ( 'NONE',  ( 10.37757302488624056, 46.52500000273118985, -31.93888565452638417 ) ) ;
#10941 = CARTESIAN_POINT ( 'NONE',  ( -4.635254915624211769, 71.85000000546237686, -14.26584774442730286 ) ) ;
#10942 = CARTESIAN_POINT ( 'NONE',  ( -33.58253175000000113, 55.27500000273120406, -10.91162601494193218 ) ) ;
#10943 = CARTESIAN_POINT ( 'NONE',  ( -27.16883889988623935, 37.57500000273117280, 19.73931689729374739 ) ) ;
#10944 = CARTESIAN_POINT ( 'NONE',  ( 32.50000000000000000, 23.50000000546237544, -3.980102097228898626E-15 ) ) ;
#10945 = EDGE_CURVE ( 'NONE', #33751, #6723, #14430, .T. ) ;
#10946 = CARTESIAN_POINT ( 'NONE',  ( -2.428612866367529427E-13, 26.17968750000000000, -27.95245687107223276 ) ) ;
#10947 = CARTESIAN_POINT ( 'NONE',  ( -5.147494310547423346, 18.44874571845315003, 32.50000000000000000 ) ) ;
#10948 = CARTESIAN_POINT ( 'NONE',  ( -9.270509831248419985, 76.30000000000001137, 12.75976212528060039 ) ) ;
#10949 = CARTESIAN_POINT ( 'NONE',  ( -32.50000000000000000, 73.90000000000003411, -10.55989012756945478 ) ) ;
#10950 = CARTESIAN_POINT ( 'NONE',  ( -2.162160676586881955E-15, 8.625000002731180615, -35.31076352940723240 ) ) ;
#10951 = CARTESIAN_POINT ( 'NONE',  ( -4.523095164977117273E-15, 6.124999997268802510, 24.62258325217400312 ) ) ;
#10952 = CARTESIAN_POINT ( 'NONE',  ( -19.82091636218621389, 10.94999999453763451, 14.40073868116558842 ) ) ;
#10953 = CARTESIAN_POINT ( 'NONE',  ( 24.22776226481265383, 25.88763916574269075, 13.94119854578893580 ) ) ;
#10954 = CARTESIAN_POINT ( 'NONE',  ( -2.375766604868048137, 76.69874572391553613, 14.99999999999999822 ) ) ;
#10955 = CARTESIAN_POINT ( 'NONE',  ( -27.16883889988624290, 20.92500000273117422, -19.73931689729374028 ) ) ;
#10956 = CARTESIAN_POINT ( 'NONE',  ( 19.09188309203694800, 44.65624999999999289, 19.09188309203660694 ) ) ;
#10957 = VERTEX_POINT ( 'NONE', #24885 ) ;
#10958 = CARTESIAN_POINT ( 'NONE',  ( 6.486482029760649416E-15, 59.62500000273118417, 35.31076352940723240 ) ) ;
#10959 = ORIENTED_EDGE ( 'NONE', *, *, #32068, .T. ) ;
#10960 = CARTESIAN_POINT ( 'NONE',  ( 20.50609665441005092, 17.15624999999999645, 20.50609665440969209 ) ) ;
#10961 = CARTESIAN_POINT ( 'NONE',  ( -14.97647472619946285, 10.14361083425730925, -26.02091320914851025 ) ) ;
#10962 = CARTESIAN_POINT ( 'NONE',  ( -10.37757302488624411, 4.725000002731183812, -31.93888565452638417 ) ) ;
#10963 =( REPRESENTATION_RELATIONSHIP ('NONE','NONE', #5873, #33740 ) REPRESENTATION_RELATIONSHIP_WITH_TRANSFORMATION ( #26212 )SHAPE_REPRESENTATION_RELATIONSHIP( ) );
#10964 = VERTEX_POINT ( 'NONE', #11346 ) ;
#10965 = DIRECTION ( 'NONE',  ( 0.000000000000000000, -1.000000000000000000, 0.000000000000000000 ) ) ;
#10966 = CARTESIAN_POINT ( 'NONE',  ( -27.16883889988623935, 25.57500000273119056, 19.73931689729374739 ) ) ;
#10967 = CARTESIAN_POINT ( 'NONE',  ( 32.50000000000000711, 29.40000000546239178, 10.55989012756945122 ) ) ;
#10968 = CARTESIAN_POINT ( 'NONE',  ( -10.04305231718579172, 79.60000000000000853, -30.90933677959248982 ) ) ;
#10969 = CARTESIAN_POINT ( 'NONE',  ( 3.980102097228898626E-15, 80.00000000000001421, 32.50000000000000000 ) ) ;
#10970 = CARTESIAN_POINT ( 'NONE',  ( 5.147494310547426899, 37.94874572391552192, -32.50000000000000000 ) ) ;
#10971 = CARTESIAN_POINT ( 'NONE',  ( 27.16883889988624290, 42.17500000273119554, 19.73931689729373673 ) ) ;
#10972 = FILL_AREA_STYLE ('',( #16135 ) ) ;
#10973 = CARTESIAN_POINT ( 'NONE',  ( -32.50000000000000000, 24.09999999999999787, 10.55989012756946366 ) ) ;
#10974 = CARTESIAN_POINT ( 'NONE',  ( 6.277390505771533514E-15, 20.49999999999999289, 34.17252228774368916 ) ) ;
#10975 = CARTESIAN_POINT ( 'NONE',  ( 19.82091636218621034, 5.799999999999999822, 14.40073868116559730 ) ) ;
#10976 = CARTESIAN_POINT ( 'NONE',  ( -20.75514604977248112, 61.42500000273118133, 28.56700777964554661 ) ) ;
#10977 = CARTESIAN_POINT ( 'NONE',  ( -31.04172217648553556, 66.99999999999998579, -12.81397374188210136 ) ) ;
#10978 = CARTESIAN_POINT ( 'NONE',  ( -32.50000000000000000, 76.60000000546236265, 10.55989012756946366 ) ) ;
#10979 = CARTESIAN_POINT ( 'NONE',  ( 27.16883889988623935, 54.57500000273118701, -19.73931689729374384 ) ) ;
#10980 = CARTESIAN_POINT ( 'NONE',  ( 7.236395654485755280, 2.224999997268800378, 22.27133577429736988 ) ) ;
#10981 = CARTESIAN_POINT ( 'NONE',  ( 0.000000000000000000, 80.00000000000001421, -32.50000000000000000 ) ) ;
#10982 = CARTESIAN_POINT ( 'NONE',  ( -27.16883889988624290, 4.925000002731189319, -19.73931689729374028 ) ) ;
#10983 = EDGE_CURVE ( 'NONE', #6369, #17976, #9086, .T. ) ;
#10984 = CARTESIAN_POINT ( 'NONE',  ( -0.04044903254992426173, 43.08631916759065916, 27.95245687107223276 ) ) ;
#10985 =( BOUNDED_CURVE ( )  B_SPLINE_CURVE ( 2, ( #25875, #21085, #23653, #18844, #23483, #23990, #290, #31534, #10778, #20911, #10436, #8027, #26392 ),
 .UNSPECIFIED., .F., .F. ) 
 B_SPLINE_CURVE_WITH_KNOTS ( ( 3, 2, 2, 2, 2, 2, 3 ),
 ( 0.6987179487179486781, 0.6999999999999999556, 0.7025641025641025106, 0.7051282051282051766, 0.7076923076923077316, 0.7102564102564102866, 0.7115384615384615641 ),
 .UNSPECIFIED. ) 
 CURVE ( )  GEOMETRIC_REPRESENTATION_ITEM ( )  RATIONAL_B_SPLINE_CURVE ( ( 0.9755282581475768211, 0.9755282581475768211, 1.000000000000000000, 0.9510565162951535312, 1.000000000000000000, 0.9510565162951535312, 1.000000000000000000, 0.9510565162951535312, 1.000000000000000000, 0.9510565162951535312, 1.000000000000000000, 0.9755282581475768211, 0.9755282581475768211 ) ) 
 REPRESENTATION_ITEM ( '' )  );
#10986 = CARTESIAN_POINT ( 'NONE',  ( 5.147494310547643614, 25.94874572391553258, -32.49999999999992895 ) ) ;
#10987 = CARTESIAN_POINT ( 'NONE',  ( -5.714234795769386643, 52.00000000000003553, 32.80324308525976562 ) ) ;
#10988 = UNCERTAINTY_MEASURE_WITH_UNIT (LENGTH_MEASURE( 1.000000000000000082E-05 ), #15818, 'distance_accuracy_value', 'NONE');
#10989 = CARTESIAN_POINT ( 'NONE',  ( 33.58253175000000113, 30.22500000273118559, -10.91162601494193751 ) ) ;
#10990 = CARTESIAN_POINT ( 'NONE',  ( 20.08610463437157279, 65.29999999999999716, -27.64615127144129758 ) ) ;
#10991 = DIRECTION ( 'NONE',  ( -1.224646799147353454E-16, 1.000000000000000000, -0.000000000000000000 ) ) ;
#10992 = CARTESIAN_POINT ( 'NONE',  ( 8.601468415847520532, 77.57500000273117280, 11.83890561707634603 ) ) ;
#10993 = CARTESIAN_POINT ( 'NONE',  ( 0.04044903255045854962, 53.96055583240936926, 30.02300923189239867 ) ) ;
#10994 = CARTESIAN_POINT ( 'NONE',  ( -10.04305231718578462, 54.90000000546239534, 30.90933677959249337 ) ) ;
#10995 = CARTESIAN_POINT ( 'NONE',  ( 10.04305231718578817, 49.39999999999999858, -30.90933677959249337 ) ) ;
#10996 = CARTESIAN_POINT ( 'NONE',  ( 10.04305231718578817, 61.40000000000001279, -30.90933677959249337 ) ) ;
#10997 = AXIS2_PLACEMENT_3D ( 'NONE', #3618, #8927, #24713 ) ;
#10998 = CARTESIAN_POINT ( 'NONE',  ( 24.20753774853756113, 13.57552083333332682, 13.97622843553589789 ) ) ;
#10999 = CARTESIAN_POINT ( 'NONE',  ( -32.50000000000000000, 72.60000000546236265, 10.55989012756946366 ) ) ;
#11000 = CARTESIAN_POINT ( 'NONE',  ( -26.00068869287368756, 18.73177083333332149, -15.01150461594595775 ) ) ;
#11001 = EDGE_CURVE ( 'NONE', #220, #13542, #16672, .T. ) ;
#11002 = CARTESIAN_POINT ( 'NONE',  ( 7.236395654485755280, 16.72499999726881370, 22.27133577429736988 ) ) ;
#11003 = VERTEX_POINT ( 'NONE', #21823 ) ;
#11004 = CARTESIAN_POINT ( 'NONE',  ( 14.97647472619947351, 42.79986083425731636, 26.02091320914850314 ) ) ;
#11005 = CARTESIAN_POINT ( 'NONE',  ( 10.04305231718578817, 19.90000000546236691, -30.90933677959249337 ) ) ;
#11006 = CARTESIAN_POINT ( 'NONE',  ( 26.00068869287367335, 47.95052083333331439, 15.01150461594596308 ) ) ;
#11007 = FACE_OUTER_BOUND ( 'NONE', #11871, .T. ) ;
#11008 = CARTESIAN_POINT ( 'NONE',  ( 10.37757302488624056, 46.77500000273118985, -31.93888565452638417 ) ) ;
#11009 = CARTESIAN_POINT ( 'NONE',  ( 32.50000000000000000, 59.50000000546237544, -3.980102097228898626E-15 ) ) ;
#11010 = CARTESIAN_POINT ( 'NONE',  ( -11.25946833292375793, 81.17500000273119554, -8.180482586598733619 ) ) ;
#11011 = CARTESIAN_POINT ( 'NONE',  ( 10.37757302488624056, 36.52500000273117564, -31.93888565452638417 ) ) ;
#11012 = DIRECTION ( 'NONE',  ( -0.000000000000000000, -1.000000000000000000, -0.000000000000000000 ) ) ;
#11013 = CARTESIAN_POINT ( 'NONE',  ( -10.37757302488623701, 63.77500000273117564, 31.93888565452638417 ) ) ;
#11014 = DIRECTION ( 'NONE',  ( 0.000000000000000000, 0.000000000000000000, -1.000000000000000000 ) ) ;
#11015 = CARTESIAN_POINT ( 'NONE',  ( -33.58253175000000113, 55.22500000273117848, 10.91162601494193929 ) ) ;
#11016 = CARTESIAN_POINT ( 'NONE',  ( 30.02300923189239867, 23.60156250000000000, -2.619432448724978208E-13 ) ) ;
#11017 = CARTESIAN_POINT ( 'NONE',  ( 32.50000000000000711, 42.90000000000001279, 10.55989012756945122 ) ) ;
#11018 = CARTESIAN_POINT ( 'NONE',  ( -4.523095164977116484E-15, 8.124999997268826490, 24.62258325217400312 ) ) ;
#11019 = CARTESIAN_POINT ( 'NONE',  ( -10.37757302488623701, 3.775000002731176973, 31.93888565452638417 ) ) ;
#11020 = CARTESIAN_POINT ( 'NONE',  ( 5.779280353836490358E-15, 35.00000000546238255, 32.49999999999999289 ) ) ;
#11021 = CARTESIAN_POINT ( 'NONE',  ( -33.04126587500000056, 78.81250000409679046, 0.000000000000000000 ) ) ;
#11022 = CARTESIAN_POINT ( 'NONE',  ( -20.75514604977248112, 73.67500000273120975, 28.56700777964554661 ) ) ;
#11023 = CARTESIAN_POINT ( 'NONE',  ( 24.50000000000000000, 3.749999994537622783, 0.000000000000000000 ) ) ;
#11024 = CARTESIAN_POINT ( 'NONE',  ( 33.58253175000000113, 66.47500000273119269, -10.91162601494193751 ) ) ;
#11025 = VERTEX_POINT ( 'NONE', #22159 ) ;
#11026 =( BOUNDED_CURVE ( )  B_SPLINE_CURVE ( 2, ( #20566, #12311, #25354, #22783, #28272, #12486, #22955, #33413, #1659, #9910, #1833, #7508, #33060 ),
 .UNSPECIFIED., .F., .T. ) 
 B_SPLINE_CURVE_WITH_KNOTS ( ( 3, 2, 2, 2, 2, 2, 3 ),
 ( 0.4423076923076922906, 0.4435897435897435681, 0.4461538461538461786, 0.4487179487179487336, 0.4512820512820512886, 0.4538461538461538436, 0.4551282051282051211 ),
 .UNSPECIFIED. ) 
 CURVE ( )  GEOMETRIC_REPRESENTATION_ITEM ( )  RATIONAL_B_SPLINE_CURVE ( ( 0.9755282581475768211, 0.9755282581475768211, 1.000000000000000000, 0.9510565162951535312, 1.000000000000000000, 0.9510565162951535312, 1.000000000000000000, 0.9510565162951535312, 1.000000000000000000, 0.9510565162951535312, 1.000000000000000000, 0.9755282581475768211, 0.9755282581475768211 ) ) 
 REPRESENTATION_ITEM ( '' )  );
#11027 = FACE_OUTER_BOUND ( 'NONE', #13738, .T. ) ;
#11028 = CARTESIAN_POINT ( 'NONE',  ( 6.988114217767829928, 60.69791666666667140, -26.07999730980489872 ) ) ;
#11029 = CARTESIAN_POINT ( 'NONE',  ( -20.75514604977248823, 50.82500000273116569, -28.56700777964554305 ) ) ;
#11030 = CARTESIAN_POINT ( 'NONE',  ( -20.75514604977248112, 9.675000002731193760, 28.56700777964554661 ) ) ;
#11031 = CARTESIAN_POINT ( 'NONE',  ( -20.75514604977248823, 65.07500000273118701, -28.56700777964554305 ) ) ;
#11032 = CARTESIAN_POINT ( 'NONE',  ( -26.07999730980477437, 42.36458333333332860, 6.988114217768305103 ) ) ;
#11033 = CARTESIAN_POINT ( 'NONE',  ( 7.468012846824777284, 25.75559000092397710, 28.02196122052045268 ) ) ;
#11034 = CARTESIAN_POINT ( 'NONE',  ( 30.02300923189239867, 18.72618083240936215, -0.04044903255044467877 ) ) ;
#11035 = CARTESIAN_POINT ( 'NONE',  ( -26.29305231718578995, 72.70000000546238539, 19.10302069950538595 ) ) ;
#11036 = VECTOR ( 'NONE', #4434, 1000.000000000000000 ) ;
#11037 = CARTESIAN_POINT ( 'NONE',  ( -13.91746824999999532, 78.77500000273117564, -4.522059556121115875 ) ) ;
#11038 = CARTESIAN_POINT ( 'NONE',  ( 27.16883889988624290, 35.92500000273118843, 19.73931689729373673 ) ) ;
#11039 = CARTESIAN_POINT ( 'NONE',  ( -6.950374756619247307, 47.22878499907602645, 26.09010956794245217 ) ) ;
#11040 = CARTESIAN_POINT ( 'NONE',  ( -7.236395654485757944, 15.22499999726881192, -22.27133577429736988 ) ) ;
#11041 = EDGE_CURVE ( 'NONE', #11374, #7955, #24897, .T. ) ;
#11042 = ADVANCED_FACE ( 'NONE', ( #7381 ), #22228, .T. ) ;
#11043 = CARTESIAN_POINT ( 'NONE',  ( 19.82091636218621034, 13.80000000000000604, 14.40073868116559730 ) ) ;
#11044 = ORIENTED_EDGE ( 'NONE', *, *, #11319, .T. ) ;
#11045 = CARTESIAN_POINT ( 'NONE',  ( 20.75514604977248467, 44.67500000273118843, -28.56700777964554305 ) ) ;
#11046 = CARTESIAN_POINT ( 'NONE',  ( 10.04305231718578817, 51.39999999999999858, -30.90933677959249337 ) ) ;
#11047 = VECTOR ( 'NONE', #9019, 1000.000000000000000 ) ;
#11048 = CIRCLE ( 'NONE', #6107, 30.00000000000004974 ) ;
#11049 = CARTESIAN_POINT ( 'NONE',  ( 0.04044903254993986036, 55.11756916759064495, -27.95245687107223986 ) ) ;
#11050 = CARTESIAN_POINT ( 'NONE',  ( -20.75514604977248112, 71.67500000273116711, 28.56700777964554661 ) ) ;
#11051 = ORIENTED_EDGE ( 'NONE', *, *, #4371, .T. ) ;
#11052 = CARTESIAN_POINT ( 'NONE',  ( -20.75514604977248112, 19.42500000273117777, 28.56700777964554661 ) ) ;
#11053 = EDGE_CURVE ( 'NONE', #25478, #15526, #27808, .T. ) ;
#11054 = CARTESIAN_POINT ( 'NONE',  ( -7.505752307972844761, 24.60416666666666430, 28.01184896238304134 ) ) ;
#11055 = ORIENTED_EDGE ( 'NONE', *, *, #31228, .F. ) ;
#11056 = CARTESIAN_POINT ( 'NONE',  ( 1.093617666956751375E-13, 66.00000000546238255, -32.50000000000000711 ) ) ;
#11057 = CARTESIAN_POINT ( 'NONE',  ( 33.58253175000000823, 56.02500000273117564, 10.91162601494192863 ) ) ;
#11058 = CARTESIAN_POINT ( 'NONE',  ( -20.50609665441004736, 46.37500000000000000, -20.50609665440969565 ) ) ;
#11059 = CARTESIAN_POINT ( 'NONE',  ( 10.04305231718578817, 19.90000000546238113, -30.90933677959249337 ) ) ;
#11060 = CARTESIAN_POINT ( 'NONE',  ( -15.00000000000000000, 80.25000000546239676, 0.000000000000000000 ) ) ;
#11061 = CARTESIAN_POINT ( 'NONE',  ( 18.94512977948575738, 6.924999997268810326, 13.76444248337723408 ) ) ;
#11062 = CARTESIAN_POINT ( 'NONE',  ( -10.37757302488623701, 21.77500000273119340, 31.93888565452638417 ) ) ;
#11063 = CARTESIAN_POINT ( 'NONE',  ( -20.08610463437156923, 64.29999999999996874, 27.64615127144130113 ) ) ;
#11064 = CARTESIAN_POINT ( 'NONE',  ( -7.468012846824272799, 60.97878499907603356, 28.02196122052058413 ) ) ;
#11065 = CARTESIAN_POINT ( 'NONE',  ( 10.04305231718578817, 75.90000000546237402, -30.90933677959249337 ) ) ;
#11066 = CARTESIAN_POINT ( 'NONE',  ( -26.29305231718579350, 9.800000000000016698, -19.10302069950537884 ) ) ;
#11067 = CARTESIAN_POINT ( 'NONE',  ( -26.07999730980477437, 59.55208333333332149, 6.988114217768305103 ) ) ;
#11068 = CARTESIAN_POINT ( 'NONE',  ( 7.570916362186213000, 18.14999999453761959, -23.30088464923126423 ) ) ;
#11069 = CARTESIAN_POINT ( 'NONE',  ( -8.601468415847518756, 78.57500000273120122, -11.83890561707634781 ) ) ;
#11070 = CARTESIAN_POINT ( 'NONE',  ( 6.988114217768294445, 31.19270833333333215, 26.07999730980477437 ) ) ;
#11071 = CARTESIAN_POINT ( 'NONE',  ( -2.162160676586881955E-15, 26.62500000273118417, -35.31076352940723240 ) ) ;
#11072 = CARTESIAN_POINT ( 'NONE',  ( -33.58253175000000113, 71.02500000273118985, -10.91162601494193218 ) ) ;
#11073 = CIRCLE ( 'NONE', #7780, 1.999999999999993117 ) ;
#11074 = CARTESIAN_POINT ( 'NONE',  ( -10.37757302488623701, 29.77500000273118630, 31.93888565452638417 ) ) ;
#11075 = CARTESIAN_POINT ( 'NONE',  ( -33.58253175000000113, 15.47500000273118381, 10.91162601494193929 ) ) ;
#11076 = CARTESIAN_POINT ( 'NONE',  ( -19.11951029504763611, 60.70350666759063785, 19.06425588902592239 ) ) ;
#11077 = CARTESIAN_POINT ( 'NONE',  ( -10.37757302488623701, 71.52500000273120406, 31.93888565452638417 ) ) ;
#11078 = DIRECTION ( 'NONE',  ( 0.000000000000000000, -0.9659258262890680902, 0.2588190451025213501 ) ) ;
#11079 = CARTESIAN_POINT ( 'NONE',  ( -32.50000000000000000, 56.00000000000000711, 0.000000000000000000 ) ) ;
#11080 = DIRECTION ( 'NONE',  ( 0.000000000000000000, -0.000000000000000000, 1.000000000000000000 ) ) ;
#11081 = CARTESIAN_POINT ( 'NONE',  ( 27.16883889988624290, 57.92500000273120975, 19.73931689729373673 ) ) ;
#11082 = CARTESIAN_POINT ( 'NONE',  ( 7.236395654485760609, 17.52499999726880731, -22.27133577429736633 ) ) ;
#11083 = EDGE_LOOP ( 'NONE', ( #4315, #12754, #11455, #31462 ) ) ;
#11084 = CARTESIAN_POINT ( 'NONE',  ( -20.75514604977248112, 65.67500000273118133, 28.56700777964554661 ) ) ;
#11085 = CARTESIAN_POINT ( 'NONE',  ( -20.75514604977248823, 2.825000002731177240, -28.56700777964554305 ) ) ;
#11086 = CARTESIAN_POINT ( 'NONE',  ( -14.47279130897151589, 5.324999997268799135, -19.92008829642072598 ) ) ;
#11087 = CARTESIAN_POINT ( 'NONE',  ( -0.04044903254992426173, 25.89881916759064140, 27.95245687107223276 ) ) ;
#11088 =( BOUNDED_CURVE ( )  B_SPLINE_CURVE ( 2, ( #9508, #12082, #1438, #22550, #4537, #33002, #9003, #22059, #19484, #19650, #17419, #32503, #27536 ),
 .UNSPECIFIED., .F., .T. ) 
 B_SPLINE_CURVE_WITH_KNOTS ( ( 3, 2, 2, 2, 2, 2, 3 ),
 ( 0.3055555555555555802, 0.3111111111111111160, 0.3222222222222222432, 0.3333333333333333148, 0.3444444444444444420, 0.3555555555555555691, 0.3611111111111111049 ),
 .UNSPECIFIED. ) 
 CURVE ( )  GEOMETRIC_REPRESENTATION_ITEM ( )  RATIONAL_B_SPLINE_CURVE ( ( 0.9755282581475767101, 0.9755282581475768211, 1.000000000000000000, 0.9510565162951535312, 1.000000000000000000, 0.9510565162951535312, 1.000000000000000000, 0.9510565162951535312, 1.000000000000000000, 0.9510565162951535312, 1.000000000000000000, 0.9755282581475768211, 0.9755282581475768211 ) ) 
 REPRESENTATION_ITEM ( '' )  );
#11089 = EDGE_LOOP ( 'NONE', ( #5344, #9676, #30223, #30819 ) ) ;
#11090 = CARTESIAN_POINT ( 'NONE',  ( 10.37757302488624056, 38.52500000273119696, -31.93888565452638417 ) ) ;
#11091 = CARTESIAN_POINT ( 'NONE',  ( -19.82091636218621389, 1.200000000000006617, 14.40073868116558842 ) ) ;
#11092 = ORIENTED_EDGE ( 'NONE', *, *, #22664, .F. ) ;
#11094 = CARTESIAN_POINT ( 'NONE',  ( -26.00068869287368756, 49.66927083333330728, -15.01150461594595775 ) ) ;
#11093 =( BOUNDED_CURVE ( )  B_SPLINE_CURVE ( 2, ( #27496, #3985, #32463, #17376, #14797, #25261, #14458, #1400, #11876, #13076, #30742, #23207, #26288 ),
 .UNSPECIFIED., .F., .T. ) 
 B_SPLINE_CURVE_WITH_KNOTS ( ( 3, 2, 2, 2, 2, 2, 3 ),
 ( 0.5833333333333332593, 0.5888888888888889062, 0.5999999999999999778, 0.6111111111111111605, 0.6222222222222222321, 0.6333333333333333037, 0.6388888888888889506 ),
 .UNSPECIFIED. ) 
 CURVE ( )  GEOMETRIC_REPRESENTATION_ITEM ( )  RATIONAL_B_SPLINE_CURVE ( ( 0.9755282581475768211, 0.9755282581475765991, 1.000000000000000000, 0.9510565162951535312, 1.000000000000000000, 0.9510565162951535312, 1.000000000000000000, 0.9510565162951535312, 1.000000000000000000, 0.9510565162951535312, 1.000000000000000000, 0.9755282581475765991, 0.9755282581475768211 ) ) 
 REPRESENTATION_ITEM ( '' )  );
#11095 = CARTESIAN_POINT ( 'NONE',  ( -1.778240108872766143E-15, 12.00000000546238077, -32.49999999999999289 ) ) ;
#11096 = CARTESIAN_POINT ( 'NONE',  ( 10.04305231718578817, 59.39999999999999147, -30.90933677959249337 ) ) ;
#11097 = CARTESIAN_POINT ( 'NONE',  ( -10.37757302488624411, 74.72500000273119269, -31.93888565452638417 ) ) ;
#11098 = CARTESIAN_POINT ( 'NONE',  ( -15.01150461594595775, 24.74739583333332504, 26.00068869287368756 ) ) ;
#11099 = CARTESIAN_POINT ( 'NONE',  ( 24.50000000000000355, 7.900000000000012790, 7.960532557706212486 ) ) ;
#11100 = CARTESIAN_POINT ( 'NONE',  ( 6.486482029760649416E-15, 7.875000002731193049, 35.31076352940723240 ) ) ;
#11101 = CARTESIAN_POINT ( 'NONE',  ( -20.75514604977248823, 24.82500000273117635, -28.56700777964554305 ) ) ;
#11102 = CARTESIAN_POINT ( 'NONE',  ( -13.91746824999999532, 76.97500000273119269, 4.522059556121122093 ) ) ;
#11103 = CARTESIAN_POINT ( 'NONE',  ( 23.41746824999999887, 0.8749999972688105032, 0.000000000000000000 ) ) ;
#11104 = CARTESIAN_POINT ( 'NONE',  ( 14.97647472619900455, 38.77826416574269075, -26.02091320914876960 ) ) ;
#11105 = CARTESIAN_POINT ( 'NONE',  ( 8.601468415847520532, 76.07500000273118701, 11.83890561707634781 ) ) ;
#11106 = CARTESIAN_POINT ( 'NONE',  ( -2.584737979205442066E-13, 46.80468750000000000, -30.02300923189239867 ) ) ;
#11107 = CARTESIAN_POINT ( 'NONE',  ( -15.14183272437242778, 11.29999999999999361, 20.84094480462497856 ) ) ;
#11108 = CARTESIAN_POINT ( 'NONE',  ( 5.779280353836490358E-15, 39.00000000546237544, 32.49999999999999289 ) ) ;
#11109 = CARTESIAN_POINT ( 'NONE',  ( 7.025853678916867295, 64.12982666574268364, 26.06988505166722803 ) ) ;
#11110 = CARTESIAN_POINT ( 'NONE',  ( 27.16883889988624290, 41.92500000273119554, 19.73931689729373673 ) ) ;
#11111 = VECTOR ( 'NONE', #2031, 1000.000000000000000 ) ;
#11112 = CARTESIAN_POINT ( 'NONE',  ( -8.601468415847518756, 80.57500000273118701, -11.83890561707634781 ) ) ;
#11113 = CARTESIAN_POINT ( 'NONE',  ( 20.75514604977248467, 56.67500000273119554, -28.56700777964554305 ) ) ;
#11114 = CARTESIAN_POINT ( 'NONE',  ( 27.16883889988623935, 36.57500000273117280, -19.73931689729374384 ) ) ;
#11115 = CARTESIAN_POINT ( 'NONE',  ( 6.350543635241933771, 16.99999999999999289, 23.08040691491506280 ) ) ;
#11116 = VECTOR ( 'NONE', #15845, 1000.000000000000000 ) ;
#11117 = CARTESIAN_POINT ( 'NONE',  ( -24.20753774853756823, 22.16927083333332860, -13.97622843553588723 ) ) ;
#11118 = CARTESIAN_POINT ( 'NONE',  ( 24.50000000000000000, 11.74999999453762989, 0.000000000000000000 ) ) ;
#11119 = CARTESIAN_POINT ( 'NONE',  ( -5.147494310547531704, 44.94874572391552192, 32.49999999999996447 ) ) ;
#11120 = CARTESIAN_POINT ( 'NONE',  ( -10.04305231718578462, 72.40000000000000568, 30.90933677959249337 ) ) ;
#11121 = CARTESIAN_POINT ( 'NONE',  ( 10.37757302488624767, 11.72500000273117493, 31.93888565452638417 ) ) ;
#11122 = CARTESIAN_POINT ( 'NONE',  ( 1.507698388325705758E-15, 3.124999997268809615, -24.62258325217400312 ) ) ;
#11123 = CARTESIAN_POINT ( 'NONE',  ( 2.445080149700053643E-15, 74.75000000546239676, 15.00000000000000000 ) ) ;
#11124 = CARTESIAN_POINT ( 'NONE',  ( -19.06425588902558133, 30.32774333240935150, 19.11951029504797006 ) ) ;
#11125 = CARTESIAN_POINT ( 'NONE',  ( -1.778240108872766143E-15, 59.50000000000000711, -32.49999999999999289 ) ) ;
#11126 = CARTESIAN_POINT ( 'NONE',  ( 33.58253175000000113, 18.22500000273118559, -10.91162601494193574 ) ) ;
#11127 = CARTESIAN_POINT ( 'NONE',  ( 24.20753774853756113, 54.82552083333331439, 13.97622843553589789 ) ) ;
#11128 = ORIENTED_EDGE ( 'NONE', *, *, #20063, .T. ) ;
#11129 = CARTESIAN_POINT ( 'NONE',  ( -2.162160676586881955E-15, 58.62500000273118417, -35.31076352940723240 ) ) ;
#11130 = ADVANCED_FACE ( 'NONE', ( #20617 ), #17884, .T. ) ;
#11131 = ORIENTED_EDGE ( 'NONE', *, *, #33267, .F. ) ;
#11132 = CARTESIAN_POINT ( 'NONE',  ( -2.584737979205441561E-13, 26.17968750000000000, -30.02300923189239512 ) ) ;
#11133 = CARTESIAN_POINT ( 'NONE',  ( -7.468012846824771955, 24.03684000092397000, -28.02196122052045624 ) ) ;
#11134 = DIRECTION ( 'NONE',  ( -1.000000000000000000, 0.000000000000000000, 0.000000000000000000 ) ) ;
#11135 = ADVANCED_FACE ( 'NONE', ( #17865, #14939 ), #7205, .F. ) ;
#11136 = ORIENTED_EDGE ( 'NONE', *, *, #22154, .F. ) ;
#11137 = CARTESIAN_POINT ( 'NONE',  ( 23.41746824999999887, 0.6249999972688102812, 0.000000000000000000 ) ) ;
#11138 = CARTESIAN_POINT ( 'NONE',  ( -20.75514604977248823, 31.07500000273118701, -28.56700777964554305 ) ) ;
#11139 = CARTESIAN_POINT ( 'NONE',  ( 20.08610463437158344, 29.20000000546237118, 27.64615127144129403 ) ) ;
#11140 = CARTESIAN_POINT ( 'NONE',  ( 15.00000000000000000, 73.10000000000000853, -4.873795443493596835 ) ) ;
#11141 = CARTESIAN_POINT ( 'NONE',  ( -32.50000000000000000, 54.40000000546238823, -10.55989012756945300 ) ) ;
#11142 = CARTESIAN_POINT ( 'NONE',  ( 0.000000000000000000, 122.0000000000000000, 0.000000000000000000 ) ) ;
#11143 = CARTESIAN_POINT ( 'NONE',  ( 20.75514604977248467, 42.67500000273119554, -28.56700777964554305 ) ) ;
#11144 = CARTESIAN_POINT ( 'NONE',  ( 32.50000000000000000, 23.09999999999999787, -10.55989012756945833 ) ) ;
#11145 = CARTESIAN_POINT ( 'NONE',  ( 26.29305231718579350, 18.79999999999998295, 19.10302069950537529 ) ) ;
#11146 = CARTESIAN_POINT ( 'NONE',  ( -15.14183272437242600, 13.29999999999998650, 20.84094480462497856 ) ) ;
#11147 = CARTESIAN_POINT ( 'NONE',  ( -10.37757302488623701, 61.52500000273120406, 31.93888565452638417 ) ) ;
#11148 = CARTESIAN_POINT ( 'NONE',  ( -24.50000000000001066, 8.849999994537624204, 7.960532557706201828 ) ) ;
#11149 = CARTESIAN_POINT ( 'NONE',  ( -33.58253175000000113, 53.37500000273118417, 0.000000000000000000 ) ) ;
#11150 = CARTESIAN_POINT ( 'NONE',  ( 14.47279130897151944, 10.92499999726882365, -19.92008829642072598 ) ) ;
#11151 = CARTESIAN_POINT ( 'NONE',  ( -7.570916362186210335, 8.599999999999996092, -23.30088464923126779 ) ) ;
#11152 = CARTESIAN_POINT ( 'NONE',  ( 27.16883889988624290, 5.925000002731190207, 19.73931689729373673 ) ) ;
#11153 = CARTESIAN_POINT ( 'NONE',  ( -19.11951029504763611, 43.51600666759065206, 19.06425588902592239 ) ) ;
#11154 = CARTESIAN_POINT ( 'NONE',  ( 32.46022989551244819, 67.00000000000000000, -2.703243202363984299 ) ) ;
#11155 = CARTESIAN_POINT ( 'NONE',  ( -10.04305231718579172, 19.60000000000000497, -30.90933677959248982 ) ) ;
#11156 = CARTESIAN_POINT ( 'NONE',  ( -20.75514604977248112, 29.42500000273118133, 28.56700777964554661 ) ) ;
#11157 = CARTESIAN_POINT ( 'NONE',  ( -32.50000000000000000, 56.60000000546236976, 10.55989012756946366 ) ) ;
#11158 = CARTESIAN_POINT ( 'NONE',  ( 10.04305231718579705, 61.10000000546238397, 30.90933677959248982 ) ) ;
#11159 = CIRCLE ( 'NONE', #4014, 26.50000000000000355 ) ;
#11160 = CARTESIAN_POINT ( 'NONE',  ( -26.29305231718579350, 30.30000000546237260, -19.10302069950537884 ) ) ;
#11161 = CARTESIAN_POINT ( 'NONE',  ( -20.53372385742107653, 55.24961833240936926, -20.47846945139867003 ) ) ;
#11162 = CARTESIAN_POINT ( 'NONE',  ( -2.092463501923844636E-15, 48.00000000546238255, -34.17252228774368916 ) ) ;
#11163 = CARTESIAN_POINT ( 'NONE',  ( -11.25946833292375793, 73.57500000273120122, 8.180482586598737171 ) ) ;
#11164 = CARTESIAN_POINT ( 'NONE',  ( -26.29305231718578995, 58.70000000546237118, 19.10302069950538595 ) ) ;
#11165 = CARTESIAN_POINT ( 'NONE',  ( -13.97622843553632421, 25.89322916666666430, -24.20753774853731599 ) ) ;
#11166 = ORIENTED_EDGE ( 'NONE', *, *, #17545, .F. ) ;
#11167 = CARTESIAN_POINT ( 'NONE',  ( 33.58253175000000113, 74.22500000273119269, -10.91162601494193751 ) ) ;
#11168 = CARTESIAN_POINT ( 'NONE',  ( -28.01184896238290278, 28.61458333333333215, 7.505752307973363457 ) ) ;
#11169 = CARTESIAN_POINT ( 'NONE',  ( 23.41746824999999887, 13.02499999726881619, 7.608796670333735079 ) ) ;
#11170 = ORIENTED_EDGE ( 'NONE', *, *, #5900, .F. ) ;
#11171 = CARTESIAN_POINT ( 'NONE',  ( -14.97647472619946285, 41.08111083425730214, -26.02091320914851025 ) ) ;
#11172 = CARTESIAN_POINT ( 'NONE',  ( -10.04305231718579172, 16.10000000546236976, -30.90933677959248982 ) ) ;
#11173 = CARTESIAN_POINT ( 'NONE',  ( -28.01184896238304134, 49.52604166666666430, -7.505752307972844761 ) ) ;
#11174 = CARTESIAN_POINT ( 'NONE',  ( -30.02300923189239512, 66.57031250000000000, 2.654126918244515359E-13 ) ) ;
#11175 = CARTESIAN_POINT ( 'NONE',  ( 20.75514604977248467, 44.67500000273118843, -28.56700777964554305 ) ) ;
#11176 = CARTESIAN_POINT ( 'NONE',  ( 10.04305231718579705, 53.10000000546239107, 30.90933677959248982 ) ) ;
#11177 = CARTESIAN_POINT ( 'NONE',  ( -8.960552108402742093E-16, 80.87500000273116996, -14.63369212191046387 ) ) ;
#11178 = CARTESIAN_POINT ( 'NONE',  ( 27.16883889988624290, 35.92500000273118843, 19.73931689729373673 ) ) ;
#11179 = LINE ( 'NONE', #21650, #7195 ) ;
#11180 = CARTESIAN_POINT ( 'NONE',  ( 6.486482029760649416E-15, 63.87500000273119127, 35.31076352940723240 ) ) ;
#11181 = AXIS2_PLACEMENT_3D ( 'NONE', #5705, #29200, #10857 ) ;
#11182 = CARTESIAN_POINT ( 'NONE',  ( -2.092463501923844636E-15, 43.49999999999999289, -34.17252228774368916 ) ) ;
#11183 = CARTESIAN_POINT ( 'NONE',  ( 18.94512977948576093, 8.824999997268822227, -13.76444248337722875 ) ) ;
#11184 =( BOUNDED_CURVE ( )  B_SPLINE_CURVE ( 2, ( #1676, #12151, #28455, #10277, #4945, #12503, #2029, #33785, #15081, #22971, #33430, #20918, #13182 ),
 .UNSPECIFIED., .F., .F. ) 
 B_SPLINE_CURVE_WITH_KNOTS ( ( 3, 2, 2, 2, 2, 2, 3 ),
 ( 0.1987179487179487336, 0.2000000000000000111, 0.2025641025641025661, 0.2051282051282051211, 0.2076923076923077038, 0.2102564102564102588, 0.2115384615384615363 ),
 .UNSPECIFIED. ) 
 CURVE ( )  GEOMETRIC_REPRESENTATION_ITEM ( )  RATIONAL_B_SPLINE_CURVE ( ( 0.9755282581475768211, 0.9755282581475770431, 1.000000000000000000, 0.9510565162951535312, 1.000000000000000000, 0.9510565162951535312, 1.000000000000000000, 0.9510565162951535312, 1.000000000000000000, 0.9510565162951535312, 1.000000000000000000, 0.9755282581475768211, 0.9755282581475768211 ) ) 
 REPRESENTATION_ITEM ( '' )  );
#11185 = CARTESIAN_POINT ( 'NONE',  ( 27.16883889988624290, 2.175000002731186655, 19.73931689729373673 ) ) ;
#11186 = FACE_OUTER_BOUND ( 'NONE', #28125, .T. ) ;
#11187 = CARTESIAN_POINT ( 'NONE',  ( -13.91746824999999532, 75.47500000273116427, 4.522059556121122093 ) ) ;
#11188 = CARTESIAN_POINT ( 'NONE',  ( 33.58253175000000113, 72.47500000273119269, -10.91162601494193574 ) ) ;
#11189 = DIRECTION ( 'NONE',  ( -0.000000000000000000, -1.000000000000000000, -0.000000000000000000 ) ) ;
#11190 = CARTESIAN_POINT ( 'NONE',  ( -10.37757302488624411, 68.97500000273119269, -31.93888565452638417 ) ) ;
#11191 = ORIENTED_EDGE ( 'NONE', *, *, #9439, .T. ) ;
#11192 = DIRECTION ( 'NONE',  ( -1.224646799147353454E-16, 1.000000000000000000, -0.000000000000000000 ) ) ;
#11193 = CARTESIAN_POINT ( 'NONE',  ( 0.04044903254993986036, 13.86756916759064318, -27.95245687107223986 ) ) ;
#11194 = DIRECTION ( 'NONE',  ( -1.224646799147353454E-16, 1.000000000000000000, -0.000000000000000000 ) ) ;
#11195 = CARTESIAN_POINT ( 'NONE',  ( -10.37757302488623701, 47.52500000273117564, 31.93888565452638417 ) ) ;
#11196 = CARTESIAN_POINT ( 'NONE',  ( -27.16883889988624290, 13.17500000273118310, -19.73931689729374028 ) ) ;
#11197 = CARTESIAN_POINT ( 'NONE',  ( -10.37757302488623701, 59.77500000273121117, 31.93888565452638417 ) ) ;
#11198 = CARTESIAN_POINT ( 'NONE',  ( -6.988114217768288228, 53.53645833333332860, -26.07999730980477437 ) ) ;
#11199 = CARTESIAN_POINT ( 'NONE',  ( -0.04044903254990864921, 36.21131916759064495, 30.02300923189239867 ) ) ;
#11200 = CARTESIAN_POINT ( 'NONE',  ( 25.98046417659831775, 32.18972249907602645, -15.04653450569338879 ) ) ;
#11201 = CARTESIAN_POINT ( 'NONE',  ( 10.04305231718579705, 67.10000000546239107, 30.90933677959248982 ) ) ;
#11202 = LINE ( 'NONE', #19100, #32491 ) ;
#11203 = CARTESIAN_POINT ( 'NONE',  ( 27.16883889988623935, 40.32500000273120122, -19.73931689729374384 ) ) ;
#11204 = CARTESIAN_POINT ( 'NONE',  ( 27.95245687107223276, 56.53868083240936215, -0.04044903255042905932 ) ) ;
#11205 = CARTESIAN_POINT ( 'NONE',  ( 14.47279130897151767, 12.92499999726881832, -19.92008829642072598 ) ) ;
#11206 = CARTESIAN_POINT ( 'NONE',  ( -24.50000000000000000, 4.649999994537640902, -7.960532557706207157 ) ) ;
#11207 = ORIENTED_EDGE ( 'NONE', *, *, #5341, .F. ) ;
#11208 = CARTESIAN_POINT ( 'NONE',  ( 10.37757302488624056, 46.77500000273120406, -31.93888565452638417 ) ) ;
#11209 = DIRECTION ( 'NONE',  ( 0.000000000000000000, 0.000000000000000000, 1.000000000000000000 ) ) ;
#11210 = CARTESIAN_POINT ( 'NONE',  ( 24.22776226481241224, 52.25298583425730925, -13.94119854578936923 ) ) ;
#11211 = CARTESIAN_POINT ( 'NONE',  ( 27.16883889988623935, 70.57500000273120122, -19.73931689729374384 ) ) ;
#11212 = VERTEX_POINT ( 'NONE', #4635 ) ;
#11213 = CARTESIAN_POINT ( 'NONE',  ( 10.37757302488624767, 19.72500000273118204, 31.93888565452638417 ) ) ;
#11214 = CARTESIAN_POINT ( 'NONE',  ( -15.01150461594642138, 25.89322916666666430, -26.00068869287340334 ) ) ;
#11215 = ORIENTED_EDGE ( 'NONE', *, *, #8603, .T. ) ;
#11216 = CARTESIAN_POINT ( 'NONE',  ( 5.147494310547434893, 65.05125428700922896, 32.49999999999999289 ) ) ;
#11217 = CARTESIAN_POINT ( 'NONE',  ( -33.58253175000000113, 55.02500000273118985, -10.91162601494193218 ) ) ;
#11218 = CARTESIAN_POINT ( 'NONE',  ( -28.01184896238304134, 56.40104166666666430, -7.505752307972844761 ) ) ;
#11219 = CARTESIAN_POINT ( 'NONE',  ( -32.50000000000000000, 16.40000000546239178, -10.55989012756945478 ) ) ;
#11220 = CARTESIAN_POINT ( 'NONE',  ( 0.000000000000000000, 0.000000000000000000, 0.000000000000000000 ) ) ;
#11221 = CARTESIAN_POINT ( 'NONE',  ( 18.94512977948576093, 11.32499999726882578, -13.76444248337722875 ) ) ;
#11222 = MECHANICAL_DESIGN_GEOMETRIC_PRESENTATION_REPRESENTATION (  '', ( #28197 ), #7369 ) ;
#11223 = CARTESIAN_POINT ( 'NONE',  ( 33.58253175000000823, 22.27500000273116854, 10.91162601494192863 ) ) ;
#11224 = CARTESIAN_POINT ( 'NONE',  ( -24.22776226481266448, 17.29388916574268720, -13.94119854578892514 ) ) ;
#11225 = CARTESIAN_POINT ( 'NONE',  ( -4.300734207923755825, 79.27500000273118985, 13.23629886949340673 ) ) ;
#11226 = LINE ( 'NONE', #21702, #19944 ) ;
#11227 = CARTESIAN_POINT ( 'NONE',  ( 6.277390505771533514E-15, 10.49999999999998757, 34.17252228774368916 ) ) ;
#11228 = VERTEX_POINT ( 'NONE', #25057 ) ;
#11229 = CARTESIAN_POINT ( 'NONE',  ( 23.41746825000000243, 3.224999997268806151, -7.608796670333727974 ) ) ;
#11230 = CARTESIAN_POINT ( 'NONE',  ( 8.601468415847516980, 76.17500000273116711, -11.83890561707634781 ) ) ;
#11231 = CARTESIAN_POINT ( 'NONE',  ( 2.584737979205441561E-13, 41.64843750000000000, 27.95245687107222921 ) ) ;
#11232 = CARTESIAN_POINT ( 'NONE',  ( 10.37757302488624056, 24.52500000273119696, -31.93888565452638417 ) ) ;
#11233 = CARTESIAN_POINT ( 'NONE',  ( 6.486482029760649416E-15, 69.62500000273118417, 35.31076352940723240 ) ) ;
#11234 = CARTESIAN_POINT ( 'NONE',  ( -2.162160676586881955E-15, 30.87500000273119483, -35.31076352940723240 ) ) ;
#11235 = CARTESIAN_POINT ( 'NONE',  ( -10.37757302488623701, 15.77500000273117386, 31.93888565452638417 ) ) ;
#11236 = CARTESIAN_POINT ( 'NONE',  ( -33.58253175000000113, 7.375000002731169069, 0.000000000000000000 ) ) ;
#11237 = CARTESIAN_POINT ( 'NONE',  ( -24.18731323226248264, 61.41965250092398776, -14.01125832528284931 ) ) ;
#11238 = CARTESIAN_POINT ( 'NONE',  ( -2.162160676586882350E-15, 72.62500000273118417, -35.31076352940722529 ) ) ;
#11239 = CARTESIAN_POINT ( 'NONE',  ( 15.01150461594596308, 53.96614583333333570, -26.00068869287367335 ) ) ;
#11240 = CARTESIAN_POINT ( 'NONE',  ( -1.778240108872766143E-15, 12.00000000546238077, -32.49999999999999289 ) ) ;
#11241 = CARTESIAN_POINT ( 'NONE',  ( 4.300734207923757602, 76.77500000273118985, -13.23629886949340673 ) ) ;
#11242 = CARTESIAN_POINT ( 'NONE',  ( -32.50000000000000000, 56.10000000000000853, 10.55989012756946366 ) ) ;
#11243 = CARTESIAN_POINT ( 'NONE',  ( 0.000000000000000000, 80.00000000000001421, 0.000000000000000000 ) ) ;
#11244 = CARTESIAN_POINT ( 'NONE',  ( 33.58253175000000113, 60.12500000273119127, -4.112674001490185761E-15 ) ) ;
#11245 = CARTESIAN_POINT ( 'NONE',  ( -14.47279130897152122, 14.42499999726880056, 19.92008829642072243 ) ) ;
#11246 = PRESENTATION_LAYER_ASSIGNMENT (  '', '', ( #12317 ) ) ;
#11247 = ORIENTED_EDGE ( 'NONE', *, *, #10983, .F. ) ;
#11248 = CARTESIAN_POINT ( 'NONE',  ( -33.58253175000000113, 67.27500000273117564, -10.91162601494193218 ) ) ;
#11249 = CARTESIAN_POINT ( 'NONE',  ( -26.29305231718578995, 16.19999999999999218, 19.10302069950538595 ) ) ;
#11250 = CARTESIAN_POINT ( 'NONE',  ( -23.41746824999999887, 9.624999997268817609, -2.867812753649727150E-15 ) ) ;
#11251 = CARTESIAN_POINT ( 'NONE',  ( -14.01125832528285109, 26.18527750092397710, 24.18731323226248264 ) ) ;
#11252 = EDGE_LOOP ( 'NONE', ( #2519, #20929, #16365, #14646 ) ) ;
#11253 = CARTESIAN_POINT ( 'NONE',  ( 33.58253175000000823, 36.02500000273117564, 10.91162601494192863 ) ) ;
#11254 = CARTESIAN_POINT ( 'NONE',  ( -20.08610463437156923, 68.80000000546236549, 27.64615127144130113 ) ) ;
#11255 = EDGE_CURVE ( 'NONE', #16123, #6266, #32932, .T. ) ;
#11256 = ORIENTED_EDGE ( 'NONE', *, *, #23684, .F. ) ;
#11257 = CARTESIAN_POINT ( 'NONE',  ( 26.00068869287340334, 54.25260416666666430, -15.01150461594642316 ) ) ;
#11258 = CARTESIAN_POINT ( 'NONE',  ( 33.58253175000000113, 66.47500000273119269, -10.91162601494193574 ) ) ;
#11259 = CARTESIAN_POINT ( 'NONE',  ( 32.50000000000000000, 59.09999999999999432, -10.55989012756945833 ) ) ;
#11260 = CARTESIAN_POINT ( 'NONE',  ( -33.58253175000000113, 75.12500000273119838, 0.000000000000000000 ) ) ;
#11261 = CARTESIAN_POINT ( 'NONE',  ( -20.50609665441004736, 25.74999999999999645, -20.50609665440969565 ) ) ;
#11262 = CARTESIAN_POINT ( 'NONE',  ( 15.14183272437242245, 6.300000000000004263, -20.84094480462497856 ) ) ;
#11263 = CARTESIAN_POINT ( 'NONE',  ( -27.16883889988624290, 7.175000002731191096, -19.73931689729374028 ) ) ;
#11264 = CARTESIAN_POINT ( 'NONE',  ( 10.37757302488624056, 18.52500000273118985, -31.93888565452638417 ) ) ;
#11265 = CARTESIAN_POINT ( 'NONE',  ( 8.601468415847516980, 76.17500000273118133, -11.83890561707634603 ) ) ;
#11266 = CARTESIAN_POINT ( 'NONE',  ( 4.635254915624212657, 76.85000000546237686, 14.26584774442730286 ) ) ;
#11267 = CARTESIAN_POINT ( 'NONE',  ( 20.53372385742108008, 43.21836833240935505, 20.47846945139866648 ) ) ;
#11268 = CARTESIAN_POINT ( 'NONE',  ( -9.270509831248425314, 77.70000000000003126, -12.75976212528059861 ) ) ;
#11269 = CARTESIAN_POINT ( 'NONE',  ( 7.505752307972854531, 46.94791666666666430, -28.01184896238303423 ) ) ;
#11270 = EDGE_CURVE ( 'NONE', #3811, #8544, #7433, .T. ) ;
#11271 = AXIS2_PLACEMENT_3D ( 'NONE', #6979, #20377, #7319 ) ;
#11272 = CARTESIAN_POINT ( 'NONE',  ( 10.04305231718578817, 71.40000000000001990, -30.90933677959249337 ) ) ;
#11273 = CARTESIAN_POINT ( 'NONE',  ( -24.22776226481266448, 61.98138916574268364, -13.94119854578892514 ) ) ;
#11274 = CARTESIAN_POINT ( 'NONE',  ( 20.75514604977249178, 45.82500000273118701, 28.56700777964553950 ) ) ;
#11275 = CARTESIAN_POINT ( 'NONE',  ( 13.91746824999999887, 79.87500000273118417, -1.704398294459741270E-15 ) ) ;
#11276 = CARTESIAN_POINT ( 'NONE',  ( -10.37757302488624411, 48.97500000273117848, -31.93888565452638417 ) ) ;
#11277 = CARTESIAN_POINT ( 'NONE',  ( 20.75514604977249178, 32.07500000273117990, 28.56700777964553950 ) ) ;
#11278 = CYLINDRICAL_SURFACE ( 'NONE', #18430, 24.50000000000000000 ) ;
#11279 = CARTESIAN_POINT ( 'NONE',  ( 24.20753774853756113, 20.45052083333332860, 13.97622843553589789 ) ) ;
#11280 = DIRECTION ( 'NONE',  ( -1.224646799147353454E-16, 1.000000000000000000, -0.000000000000000000 ) ) ;
#11281 = CARTESIAN_POINT ( 'NONE',  ( 32.50000000000000711, 30.89999999999998437, 10.55989012756945122 ) ) ;
#11282 = CARTESIAN_POINT ( 'NONE',  ( -10.04305231718579172, 73.59999999999998010, -30.90933677959248982 ) ) ;
#11283 = CARTESIAN_POINT ( 'NONE',  ( 27.16883889988624290, 7.925000002731205306, 19.73931689729373673 ) ) ;
#11284 = CARTESIAN_POINT ( 'NONE',  ( 23.41746824999999887, 4.524999997268823293, 7.608796670333735079 ) ) ;
#11285 = CYLINDRICAL_SURFACE ( 'NONE', #24781, 32.50000000000000000 ) ;
#11286 = CARTESIAN_POINT ( 'NONE',  ( 24.18731323226221974, 28.75222249907602290, -14.01125832528328985 ) ) ;
#11287 = FACE_OUTER_BOUND ( 'NONE', #17665, .T. ) ;
#11288 = CARTESIAN_POINT ( 'NONE',  ( 10.37757302488624767, 17.72500000273119625, 31.93888565452638417 ) ) ;
#11289 = CARTESIAN_POINT ( 'NONE',  ( -4.523095164977116484E-15, 8.624999997268810503, 24.62258325217400312 ) ) ;
#11290 = CARTESIAN_POINT ( 'NONE',  ( 19.09188309203694800, 51.53124999999999289, 19.09188309203660694 ) ) ;
#11291 = EDGE_LOOP ( 'NONE', ( #31422, #6869, #10664, #23421 ) ) ;
#11292 = CARTESIAN_POINT ( 'NONE',  ( -27.16883889988624290, 56.92500000273119554, -19.73931689729374028 ) ) ;
#11293 = ORIENTED_EDGE ( 'NONE', *, *, #3422, .F. ) ;
#11294 = CARTESIAN_POINT ( 'NONE',  ( 28.01184896238290278, 26.89583333333332860, -7.505752307973347470 ) ) ;
#11295 = CARTESIAN_POINT ( 'NONE',  ( -20.47846945139902175, 23.75038166759064140, -20.53372385742072481 ) ) ;
#11296 = CARTESIAN_POINT ( 'NONE',  ( -34.92499999999992610, 0.000000000000000000, 30.00000000000004974 ) ) ;
#11297 = CARTESIAN_POINT ( 'NONE',  ( 23.41746824999999887, 4.624999997268814056, 0.000000000000000000 ) ) ;
#11298 = CARTESIAN_POINT ( 'NONE',  ( 10.37757302488624056, 30.77500000273120051, -31.93888565452638417 ) ) ;
#11299 = CARTESIAN_POINT ( 'NONE',  ( -20.08610463437156923, 30.80000000546237615, 27.64615127144130113 ) ) ;
#11300 = VECTOR ( 'NONE', #5709, 1000.000000000000000 ) ;
#11301 = CARTESIAN_POINT ( 'NONE',  ( -32.50000000000000000, 76.10000000000002274, 10.55989012756946366 ) ) ;
#11302 = CARTESIAN_POINT ( 'NONE',  ( -2.165007332552593587E-13, 52.50000000000000711, 32.50000000000000000 ) ) ;
#11303 = CARTESIAN_POINT ( 'NONE',  ( 0.000000000000000000, -12.99999999999999822, 27.00000000000000000 ) ) ;
#11304 = CARTESIAN_POINT ( 'NONE',  ( 10.37757302488624767, 45.97500000273119269, 31.93888565452638417 ) ) ;
#11305 = CARTESIAN_POINT ( 'NONE',  ( 20.08610463437157279, 23.29999999999999361, -27.64615127144129758 ) ) ;
#11306 = CARTESIAN_POINT ( 'NONE',  ( -2.092463501923844636E-15, 19.49999999999998934, -34.17252228774368916 ) ) ;
#11307 = CARTESIAN_POINT ( 'NONE',  ( 1.577395562988744260E-15, 10.49999999999998757, -25.76082449383753925 ) ) ;
#11308 = CARTESIAN_POINT ( 'NONE',  ( 33.58253175000000113, 62.12500000273119127, -4.112674001490185761E-15 ) ) ;
#11309 = CARTESIAN_POINT ( 'NONE',  ( -20.75514604977248823, 53.07500000273118701, -28.56700777964554305 ) ) ;
#11310 = CARTESIAN_POINT ( 'NONE',  ( 14.47279130897151944, 8.924999997268800556, -19.92008829642072598 ) ) ;
#11311 = CARTESIAN_POINT ( 'NONE',  ( 33.58253175000000823, 8.025000002731188076, 10.91162601494192863 ) ) ;
#11312 = CARTESIAN_POINT ( 'NONE',  ( -19.11951029504763611, 40.07850666759064495, 19.06425588902592239 ) ) ;
#11313 = EDGE_CURVE ( 'NONE', #25517, #31633, #9979, .T. ) ;
#11314 = CARTESIAN_POINT ( 'NONE',  ( 20.08610463437157279, 25.80000000546238681, -27.64615127144129758 ) ) ;
#11315 = CARTESIAN_POINT ( 'NONE',  ( 24.50000000000000000, 1.849999994537612658, -7.960532557706203605 ) ) ;
#11316 = CARTESIAN_POINT ( 'NONE',  ( -2.162160676586881955E-15, 28.62500000273118062, -35.31076352940723240 ) ) ;
#11317 = CARTESIAN_POINT ( 'NONE',  ( 3.000384657911015469E-15, 0.000000000000000000, -24.50000000000000000 ) ) ;
#11318 = CARTESIAN_POINT ( 'NONE',  ( -26.29305231718578995, 58.70000000546238539, 19.10302069950538595 ) ) ;
#11319 = EDGE_CURVE ( 'NONE', #27878, #21883, #6866, .T. ) ;
#11320 = CARTESIAN_POINT ( 'NONE',  ( 19.82091636218621389, 14.19999999999999041, -14.40073868116559197 ) ) ;
#11321 = CARTESIAN_POINT ( 'NONE',  ( -7.468012846824272799, 57.54128499907602645, 28.02196122052058413 ) ) ;
#11322 = CARTESIAN_POINT ( 'NONE',  ( -10.04305231718579172, 48.10000000546236976, -30.90933677959248982 ) ) ;
#11323 = CARTESIAN_POINT ( 'NONE',  ( 8.601468415847516980, 72.67500000273120975, -11.83890561707634781 ) ) ;
#11324 = CARTESIAN_POINT ( 'NONE',  ( 13.97622843553589966, 26.46614583333332149, -24.20753774853756113 ) ) ;
#11325 = ORIENTED_EDGE ( 'NONE', *, *, #3903, .T. ) ;
#11326 = CARTESIAN_POINT ( 'NONE',  ( -33.58253175000000113, 73.02500000273120406, -10.91162601494193218 ) ) ;
#11327 = VECTOR ( 'NONE', #7214, 1000.000000000000114 ) ;
#11328 = CARTESIAN_POINT ( 'NONE',  ( -7.505752307972844761, 31.47916666666666075, 28.01184896238304134 ) ) ;
#11329 = LINE ( 'NONE', #14579, #5880 ) ;
#11330 = ORIENTED_EDGE ( 'NONE', *, *, #2379, .T. ) ;
#11331 = CARTESIAN_POINT ( 'NONE',  ( -26.02091320914849959, 47.09673583425730214, 14.97647472619947528 ) ) ;
#11332 = CARTESIAN_POINT ( 'NONE',  ( -20.08610463437156923, 10.80000000546236549, 27.64615127144130113 ) ) ;
#11333 = AXIS2_PLACEMENT_3D ( 'NONE', #11491, #19898, #19231 ) ;
#11334 = CARTESIAN_POINT ( 'NONE',  ( -30.02300923189239512, 56.25781249999997868, 2.654126918244515359E-13 ) ) ;
#11335 = CARTESIAN_POINT ( 'NONE',  ( -1.778240108872766143E-15, 64.00000000546238255, -32.49999999999999289 ) ) ;
#11336 = CARTESIAN_POINT ( 'NONE',  ( -27.16883889988624290, 45.17500000273119554, -19.73931689729374028 ) ) ;
#11337 = CARTESIAN_POINT ( 'NONE',  ( -2.092463501923844636E-15, 52.00000000546236834, -34.17252228774368916 ) ) ;
#11338 = CARTESIAN_POINT ( 'NONE',  ( 13.91746825000000065, 80.27500000273120406, 4.522059556121114987 ) ) ;
#11339 = CARTESIAN_POINT ( 'NONE',  ( -2.162160676586881955E-15, 34.62500000273119127, -35.31076352940723240 ) ) ;
#11340 = CARTESIAN_POINT ( 'NONE',  ( -5.147494310547423346, 24.44874571845316069, 32.50000000000000000 ) ) ;
#11341 = CARTESIAN_POINT ( 'NONE',  ( -10.37757302488623701, 61.77500000273117564, 31.93888565452638417 ) ) ;
#11342 = PRESENTATION_STYLE_ASSIGNMENT (( #9096 ) ) ;
#11343 = CARTESIAN_POINT ( 'NONE',  ( 20.08610463437157279, 39.30000000000001137, -27.64615127144129758 ) ) ;
#11344 = CARTESIAN_POINT ( 'NONE',  ( -7.236395654485763274, 14.02499999726880553, 22.27133577429736633 ) ) ;
#11345 = CARTESIAN_POINT ( 'NONE',  ( -33.58253175000000113, 3.475000002731185589, 10.91162601494193929 ) ) ;
#11346 = CARTESIAN_POINT ( 'NONE',  ( 24.50000000000000000, 1.749999994537621006, 0.000000000000000000 ) ) ;
#11347 = CARTESIAN_POINT ( 'NONE',  ( 11.25946833292375793, 80.17500000273119554, 8.180482586598731842 ) ) ;
#11348 = CARTESIAN_POINT ( 'NONE',  ( 33.58253175000000113, 74.37500000273116996, -4.112674001490185761E-15 ) ) ;
#11349 = CARTESIAN_POINT ( 'NONE',  ( 0.000000000000000000, 80.00000000000001421, -32.50000000000000000 ) ) ;
#11350 = CARTESIAN_POINT ( 'NONE',  ( -27.16883889988623935, 69.57500000273118701, 19.73931689729374739 ) ) ;
#11351 = ORIENTED_EDGE ( 'NONE', *, *, #33397, .F. ) ;
#11352 = CARTESIAN_POINT ( 'NONE',  ( 24.50000000000000355, 3.849999994537637082, -7.960532557706203605 ) ) ;
#11353 = CARTESIAN_POINT ( 'NONE',  ( -14.01125832528285109, 15.87277750092397710, 24.18731323226248264 ) ) ;
#11354 = EDGE_CURVE ( 'NONE', #19648, #17565, #32951, .T. ) ;
#11355 = FACE_OUTER_BOUND ( 'NONE', #15903, .T. ) ;
#11356 = CARTESIAN_POINT ( 'NONE',  ( 33.58253175000000113, 46.12500000273119127, -4.112674001490185761E-15 ) ) ;
#11357 = CARTESIAN_POINT ( 'NONE',  ( 10.37757302488624056, 8.775000002731166759, -31.93888565452638417 ) ) ;
#11358 = CARTESIAN_POINT ( 'NONE',  ( 10.37757302488624056, 64.77500000273118985, -31.93888565452638417 ) ) ;
#11359 = CARTESIAN_POINT ( 'NONE',  ( 26.07999730980477437, 54.39583333333332860, -6.988114217768290004 ) ) ;
#11360 = CARTESIAN_POINT ( 'NONE',  ( -26.02091320914849959, 43.65923583425730925, 14.97647472619947528 ) ) ;
#11361 = EDGE_CURVE ( 'NONE', #14943, #12209, #13499, .T. ) ;
#11362 = CIRCLE ( 'NONE', #8615, 15.00000000000000000 ) ;
#11363 = CARTESIAN_POINT ( 'NONE',  ( -20.47846945139866648, 26.89024333240934439, 20.53372385742108008 ) ) ;
#11364 = CARTESIAN_POINT ( 'NONE',  ( 20.08610463437158344, 65.20000000546235697, 27.64615127144129403 ) ) ;
#11365 = CARTESIAN_POINT ( 'NONE',  ( -13.91746824999999887, 80.87500000273118417, 0.000000000000000000 ) ) ;
#11366 = CARTESIAN_POINT ( 'NONE',  ( -6.950374756619247307, 57.54128499907602645, 26.09010956794245217 ) ) ;
#11367 = CARTESIAN_POINT ( 'NONE',  ( 18.94512977948576093, 12.82499999726882578, -13.76444248337722875 ) ) ;
#11368 = CARTESIAN_POINT ( 'NONE',  ( 20.08610463437157279, 13.80000000546235839, -27.64615127144129758 ) ) ;
#11369 = EDGE_LOOP ( 'NONE', ( #14102, #12296, #19625, #9896 ) ) ;
#11370 = CARTESIAN_POINT ( 'NONE',  ( 6.486482029760649416E-15, 49.87500000273119838, 35.31076352940723240 ) ) ;
#11371 = CARTESIAN_POINT ( 'NONE',  ( -20.08610463437156923, 76.30000000000001137, 27.64615127144130113 ) ) ;
#11372 = CARTESIAN_POINT ( 'NONE',  ( 26.06988505166735592, 49.24517333425730925, 7.025853678916393896 ) ) ;
#11373 = CARTESIAN_POINT ( 'NONE',  ( 10.37757302488624056, 66.77500000273117564, -31.93888565452638417 ) ) ;
#11374 = VERTEX_POINT ( 'NONE', #10472 ) ;
#11375 = CARTESIAN_POINT ( 'NONE',  ( -27.16883889988623935, 19.32500000273117280, 19.73931689729374739 ) ) ;
#11376 = CARTESIAN_POINT ( 'NONE',  ( -7.505752307972844761, 21.16666666666666430, 28.01184896238304134 ) ) ;
#11377 = ORIENTED_EDGE ( 'NONE', *, *, #11586, .T. ) ;
#11378 =( BOUNDED_CURVE ( )  B_SPLINE_CURVE ( 2, ( #16312, #10986, #24032, #11314, #16810, #14231, #24525, #32570, #24687, #3589, #29331, #8733, #19052 ),
 .UNSPECIFIED., .F., .T. ) 
 B_SPLINE_CURVE_WITH_KNOTS ( ( 3, 2, 2, 2, 2, 2, 3 ),
 ( 0.6730769230769231282, 0.6743589743589744057, 0.6769230769230769607, 0.6794871794871795156, 0.6820512820512820706, 0.6846153846153846256, 0.6858974358974359031 ),
 .UNSPECIFIED. ) 
 CURVE ( )  GEOMETRIC_REPRESENTATION_ITEM ( )  RATIONAL_B_SPLINE_CURVE ( ( 0.9755282581475768211, 0.9755282581475778203, 1.000000000000000000, 0.9510565162951535312, 1.000000000000000000, 0.9510565162951535312, 1.000000000000000000, 0.9510565162951535312, 1.000000000000000000, 0.9510565162951535312, 1.000000000000000000, 0.9755282581475768211, 0.9755282581475768211 ) ) 
 REPRESENTATION_ITEM ( '' )  );
#11379 = CARTESIAN_POINT ( 'NONE',  ( 26.29305231718578995, 65.70000000546238539, -19.10302069950538240 ) ) ;
#11380 = CARTESIAN_POINT ( 'NONE',  ( -2.162160676586881955E-15, 56.62500000273116996, -35.31076352940723240 ) ) ;
#11381 = CARTESIAN_POINT ( 'NONE',  ( -2.584737979205441561E-13, 57.11718750000000711, -30.02300923189239512 ) ) ;
#11382 = CARTESIAN_POINT ( 'NONE',  ( -32.50000000000000000, 12.40000000546237224, -10.55989012756945478 ) ) ;
#11383 = CARTESIAN_POINT ( 'NONE',  ( 7.570916362186213000, 16.14999999453761603, -23.30088464923126423 ) ) ;
#11384 = CARTESIAN_POINT ( 'NONE',  ( -7.236395654485763274, 16.52499999726880731, 22.27133577429736633 ) ) ;
#11385 = CARTESIAN_POINT ( 'NONE',  ( -10.37757302488624411, 22.97500000273117138, -31.93888565452638417 ) ) ;
#11386 = CARTESIAN_POINT ( 'NONE',  ( -7.025853678916861966, 17.72357666574268720, -26.06988505166722803 ) ) ;
#11387 = CARTESIAN_POINT ( 'NONE',  ( 13.91746825000000065, 79.77500000273118985, 4.522059556121114987 ) ) ;
#11388 = CARTESIAN_POINT ( 'NONE',  ( -10.04305231718578462, 12.40000000000000746, 30.90933677959249337 ) ) ;
#11389 = ORIENTED_EDGE ( 'NONE', *, *, #30246, .F. ) ;
#11390 = CARTESIAN_POINT ( 'NONE',  ( -18.94512977948575738, 5.924999997268809437, -13.76444248337723231 ) ) ;
#11391 = CARTESIAN_POINT ( 'NONE',  ( 8.601468415847520532, 73.57500000273117280, 11.83890561707634781 ) ) ;
#11392 = CARTESIAN_POINT ( 'NONE',  ( 24.20753774853756113, 37.63802083333331439, 13.97622843553589789 ) ) ;
#11393 = CARTESIAN_POINT ( 'NONE',  ( -10.37757302488624411, 26.72500000273120335, -31.93888565452638417 ) ) ;
#11394 = CARTESIAN_POINT ( 'NONE',  ( 33.58253175000000113, 68.22500000273116427, -10.91162601494193751 ) ) ;
#11395 = CARTESIAN_POINT ( 'NONE',  ( 27.16883889988623935, 30.57500000273117990, -19.73931689729374384 ) ) ;
#11396 = CARTESIAN_POINT ( 'NONE',  ( -33.58253175000000113, 19.37500000273119483, 0.000000000000000000 ) ) ;
#11397 = CARTESIAN_POINT ( 'NONE',  ( 10.37757302488624056, 6.775000002731179194, -31.93888565452638417 ) ) ;
#11398 = CARTESIAN_POINT ( 'NONE',  ( 28.00173670424549499, 11.43267333425730925, 7.543491769121417612 ) ) ;
#11399 = CARTESIAN_POINT ( 'NONE',  ( -15.01150461594642138, 49.95572916666665009, -26.00068869287340334 ) ) ;
#11400 = CARTESIAN_POINT ( 'NONE',  ( -1.778240108872766143E-15, 21.50000000000000000, -32.49999999999999289 ) ) ;
#11401 = CARTESIAN_POINT ( 'NONE',  ( -13.91746824999999532, 79.47500000273119269, 4.522059556121122093 ) ) ;
#11402 = CARTESIAN_POINT ( 'NONE',  ( 6.277390505771533514E-15, 44.49999999999999289, 34.17252228774368916 ) ) ;
#11403 = CARTESIAN_POINT ( 'NONE',  ( 0.000000000000000000, 16.50000000000002842, 0.000000000000000000 ) ) ;
#11404 = CARTESIAN_POINT ( 'NONE',  ( 33.58253175000000113, 54.12500000273118417, -4.112674001490185761E-15 ) ) ;
#11405 = CARTESIAN_POINT ( 'NONE',  ( -18.94512977948576093, 16.32499999726880091, 13.76444248337722698 ) ) ;
#11406 = CIRCLE ( 'NONE', #30012, 13.38408793869266411 ) ;
#11407 = ORIENTED_EDGE ( 'NONE', *, *, #27617, .F. ) ;
#11408 = CARTESIAN_POINT ( 'NONE',  ( 33.58253175000000113, 68.37500000273121259, -4.112674001490185761E-15 ) ) ;
#11409 = DIRECTION ( 'NONE',  ( 0.000000000000000000, -1.000000000000000000, 0.000000000000000000 ) ) ;
#11410 = CARTESIAN_POINT ( 'NONE',  ( -14.47279130897152122, 3.924999997268813434, 19.92008829642072243 ) ) ;
#11411 = CARTESIAN_POINT ( 'NONE',  ( 13.94119854578937812, 22.17486083425730925, 24.22776226481240514 ) ) ;
#11412 = ORIENTED_EDGE ( 'NONE', *, *, #23100, .F. ) ;
#11413 = CARTESIAN_POINT ( 'NONE',  ( 20.75514604977249178, 37.82500000273117280, 28.56700777964553950 ) ) ;
#11414 = CARTESIAN_POINT ( 'NONE',  ( -19.82091636218621034, 0.7999999999999951594, -14.40073868116559552 ) ) ;
#11415 = ADVANCED_FACE ( 'NONE', ( #26425 ), #25103, .T. ) ;
#11416 = VERTEX_POINT ( 'NONE', #21335 ) ;
#11417 = CARTESIAN_POINT ( 'NONE',  ( -2.584737979205441561E-13, 50.24218750000000711, -30.02300923189239512 ) ) ;
#11418 = CARTESIAN_POINT ( 'NONE',  ( -20.75514604977248112, 61.67500000273117422, 28.56700777964554661 ) ) ;
#11419 = CARTESIAN_POINT ( 'NONE',  ( 9.270509831248425314, 74.95000000546237118, 12.75976212528059683 ) ) ;
#11420 = CARTESIAN_POINT ( 'NONE',  ( 20.75514604977249178, 75.82500000273118701, 28.56700777964553950 ) ) ;
#11421 = CARTESIAN_POINT ( 'NONE',  ( 15.01150461594643204, 27.61197916666666430, 26.00068869287340334 ) ) ;
#11422 = CARTESIAN_POINT ( 'NONE',  ( -24.50000000000001066, 7.100000000000007638, 7.960532557706201828 ) ) ;
#11423 = CARTESIAN_POINT ( 'NONE',  ( 20.75514604977248467, 10.67500000273119021, -28.56700777964554305 ) ) ;
#11424 = CARTESIAN_POINT ( 'NONE',  ( -33.58253175000000113, 15.22500000273119447, 10.91162601494193929 ) ) ;
#11425 = CARTESIAN_POINT ( 'NONE',  ( 11.25946833292375793, 72.07500000273120122, -8.180482586598735395 ) ) ;
#11426 = CARTESIAN_POINT ( 'NONE',  ( 28.00173670424535644, 46.08295166574269075, -7.543491769121920321 ) ) ;
#11427 = CARTESIAN_POINT ( 'NONE',  ( -12.13525491562421088, 81.79999999999998295, -8.816778784387096835 ) ) ;
#11428 = CARTESIAN_POINT ( 'NONE',  ( -20.50609665440969209, 52.39062499999999289, 20.50609665441005092 ) ) ;
#11429 = CYLINDRICAL_SURFACE ( 'NONE', #3135, 24.50000000000000000 ) ;
#11430 = LINE ( 'NONE', #10937, #11047 ) ;
#11431 = CARTESIAN_POINT ( 'NONE',  ( 13.97622843553589966, 16.15364583333333215, -24.20753774853756113 ) ) ;
#11432 = CARTESIAN_POINT ( 'NONE',  ( 20.75514604977248467, 44.42500000273120264, -28.56700777964554305 ) ) ;
#11433 = CARTESIAN_POINT ( 'NONE',  ( 13.91746824999999887, 75.87500000273116996, -1.704398294459741270E-15 ) ) ;
#11434 = CARTESIAN_POINT ( 'NONE',  ( 10.37757302488624056, 48.77500000273120406, -31.93888565452638417 ) ) ;
#11435 = CARTESIAN_POINT ( 'NONE',  ( 33.58253175000000113, 26.37500000273118417, -4.112674001490185761E-15 ) ) ;
#11436 = DIRECTION ( 'NONE',  ( 0.000000000000000000, 0.000000000000000000, 1.000000000000000000 ) ) ;
#11437 = CARTESIAN_POINT ( 'NONE',  ( 26.07999730980490227, 20.30729166666666430, 6.988114217767821046 ) ) ;
#11438 = DIRECTION ( 'NONE',  ( 0.000000000000000000, 0.000000000000000000, 1.000000000000000000 ) ) ;
#11439 = CARTESIAN_POINT ( 'NONE',  ( -15.00000000000000000, 80.00000000000001421, 0.000000000000000000 ) ) ;
#11440 = CARTESIAN_POINT ( 'NONE',  ( -10.04305231718579172, 65.60000000000000853, -30.90933677959248982 ) ) ;
#11441 = CARTESIAN_POINT ( 'NONE',  ( 6.486482029760649416E-15, 11.62500000273118950, 35.31076352940723240 ) ) ;
#11442 = CARTESIAN_POINT ( 'NONE',  ( -7.236395654485763274, 6.024999997268825958, 22.27133577429736633 ) ) ;
#11443 = EDGE_CURVE ( 'NONE', #771, #1133, #20606, .T. ) ;
#11444 = CARTESIAN_POINT ( 'NONE',  ( -15.14183272437242067, 10.44999999453763095, -20.84094480462497856 ) ) ;
#11445 = CARTESIAN_POINT ( 'NONE',  ( 26.09010956794244507, 32.61940999907601224, 6.950374756619249084 ) ) ;
#11446 = CARTESIAN_POINT ( 'NONE',  ( -10.04305231718579172, 59.59999999999998721, -30.90933677959248982 ) ) ;
#11447 = CARTESIAN_POINT ( 'NONE',  ( -20.75514604977248823, 16.82500000273120122, -28.56700777964554305 ) ) ;
#11448 = CARTESIAN_POINT ( 'NONE',  ( -14.47279130897151589, 5.824999997268811569, -19.92008829642072598 ) ) ;
#11449 = CARTESIAN_POINT ( 'NONE',  ( -6.988114217767819270, 52.10416666666666430, 26.07999730980490583 ) ) ;
#11450 = EDGE_CURVE ( 'NONE', #10494, #21929, #23736, .T. ) ;
#11451 = ORIENTED_EDGE ( 'NONE', *, *, #22718, .F. ) ;
#11452 = CARTESIAN_POINT ( 'NONE',  ( 20.75514604977249178, 53.82500000273119412, 28.56700777964553950 ) ) ;
#11453 = ADVANCED_FACE ( 'NONE', ( #200 ), #10686, .T. ) ;
#11454 = CARTESIAN_POINT ( 'NONE',  ( -33.58253175000000113, 31.37500000273117706, 0.000000000000000000 ) ) ;
#11455 = ORIENTED_EDGE ( 'NONE', *, *, #3289, .T. ) ;
#11456 = CARTESIAN_POINT ( 'NONE',  ( 15.01150461594596308, 26.46614583333332149, -26.00068869287367335 ) ) ;
#11457 = CARTESIAN_POINT ( 'NONE',  ( 20.53372385742072481, 21.17225666759064850, -20.47846945139902175 ) ) ;
#11458 = DIRECTION ( 'NONE',  ( 0.000000000000000000, 0.000000000000000000, 1.000000000000000000 ) ) ;
#11459 = CARTESIAN_POINT ( 'NONE',  ( 15.14183272437242245, 14.04999999453763593, -20.84094480462497856 ) ) ;
#11460 = ADVANCED_FACE ( 'NONE', ( #16349 ), #31611, .T. ) ;
#11461 = CARTESIAN_POINT ( 'NONE',  ( 7.236395654485755280, 8.224999997268806595, 22.27133577429736988 ) ) ;
#11462 = CARTESIAN_POINT ( 'NONE',  ( 27.16883889988624290, 30.17500000273118488, 19.73931689729373673 ) ) ;
#11463 = CARTESIAN_POINT ( 'NONE',  ( -10.04305231718579172, 28.10000000546236620, -30.90933677959248982 ) ) ;
#11464 = CARTESIAN_POINT ( 'NONE',  ( 20.08610463437158344, 72.70000000000001705, 27.64615127144129403 ) ) ;
#11465 = CARTESIAN_POINT ( 'NONE',  ( 20.08610463437157279, 33.80000000546236549, -27.64615127144129758 ) ) ;
#11466 = CARTESIAN_POINT ( 'NONE',  ( 0.000000000000000000, 80.00000000000001421, 0.000000000000000000 ) ) ;
#11467 = CARTESIAN_POINT ( 'NONE',  ( 20.47846945139902530, 59.84413166759065206, 20.53372385742071771 ) ) ;
#11468 = CARTESIAN_POINT ( 'NONE',  ( -2.162160676586881955E-15, 42.87500000273119127, -35.31076352940723240 ) ) ;
#11469 = CARTESIAN_POINT ( 'NONE',  ( -14.47279130897151589, 9.824999997268802687, -19.92008829642072598 ) ) ;
#11470 = CARTESIAN_POINT ( 'NONE',  ( -26.29305231718578995, 12.19999999999998863, 19.10302069950538595 ) ) ;
#11471 = CARTESIAN_POINT ( 'NONE',  ( 19.82091636218621389, 10.20000000000001528, -14.40073868116559197 ) ) ;
#11472 = CARTESIAN_POINT ( 'NONE',  ( -14.01125832528328985, 41.64284749907602645, -24.18731323226223040 ) ) ;
#11473 = CARTESIAN_POINT ( 'NONE',  ( 10.37757302488624767, 63.72500000273117848, 31.93888565452638417 ) ) ;
#11474 = CARTESIAN_POINT ( 'NONE',  ( 10.37757302488624056, 46.77500000273118985, -31.93888565452638417 ) ) ;
#11475 = CARTESIAN_POINT ( 'NONE',  ( -18.94512977948575738, 9.424999997268812990, -13.76444248337723231 ) ) ;
#11476 = CARTESIAN_POINT ( 'NONE',  ( -4.223320258572819786E-15, 3.499999999999996891, 24.50000000000000000 ) ) ;
#11477 = CARTESIAN_POINT ( 'NONE',  ( 6.486482029760649416E-15, 7.625000002731170845, 35.31076352940723240 ) ) ;
#11478 = CARTESIAN_POINT ( 'NONE',  ( -24.22776226481240514, 40.22173583425730925, 13.94119854578937812 ) ) ;
#11479 = CARTESIAN_POINT ( 'NONE',  ( 21.01773679462570499, 16.99999999999998934, -10.35453523078706617 ) ) ;
#11480 = CARTESIAN_POINT ( 'NONE',  ( -15.83883214465799405, 52.00000000000004263, 29.08710441171866279 ) ) ;
#11481 = CARTESIAN_POINT ( 'NONE',  ( -20.75514604977248823, 28.82500000273116569, -28.56700777964554305 ) ) ;
#11482 = CARTESIAN_POINT ( 'NONE',  ( -26.29305231718579350, 56.30000000546238681, -19.10302069950537884 ) ) ;
#11483 = CARTESIAN_POINT ( 'NONE',  ( -20.08610463437157989, 58.20000000546238539, -27.64615127144129758 ) ) ;
#11484 = CARTESIAN_POINT ( 'NONE',  ( 10.04305231718579705, 60.60000000000000142, 30.90933677959248982 ) ) ;
#11485 = CARTESIAN_POINT ( 'NONE',  ( -26.02091320914878025, 51.66888916574269075, -14.97647472619899389 ) ) ;
#11486 = CARTESIAN_POINT ( 'NONE',  ( 10.04305231718578817, 47.90000000546239534, -30.90933677959249337 ) ) ;
#11487 = CARTESIAN_POINT ( 'NONE',  ( -11.25946833292375793, 71.57500000273120122, 8.180482586598737171 ) ) ;
#11488 = CARTESIAN_POINT ( 'NONE',  ( -24.20753774853756823, 29.04427083333332504, -13.97622843553588723 ) ) ;
#11489 = CARTESIAN_POINT ( 'NONE',  ( -2.162160676586881955E-15, 74.62500000273116996, -35.31076352940723240 ) ) ;
#11490 = CARTESIAN_POINT ( 'NONE',  ( 20.50609665441005092, 34.34374999999999289, 20.50609665440969209 ) ) ;
#11491 = CARTESIAN_POINT ( 'NONE',  ( -19.79898987322349768, 67.00000000000000000, -19.79898987322315307 ) ) ;
#11492 = ORIENTED_EDGE ( 'NONE', *, *, #32206, .T. ) ;
#11493 = CARTESIAN_POINT ( 'NONE',  ( 28.02196122052045268, 45.52121500092397355, -7.468012846824774620 ) ) ;
#11494 = CARTESIAN_POINT ( 'NONE',  ( 20.08610463437158344, 9.200000005462387165, 27.64615127144129403 ) ) ;
#11495 = CARTESIAN_POINT ( 'NONE',  ( -2.584737979205441561E-13, 57.11718750000000711, -30.02300923189239512 ) ) ;
#11496 = CARTESIAN_POINT ( 'NONE',  ( -32.50000000000000000, 46.50000000546239676, 0.000000000000000000 ) ) ;
#11497 = CARTESIAN_POINT ( 'NONE',  ( 6.486482029760649416E-15, 47.87500000273117706, 35.31076352940723240 ) ) ;
#11498 = CARTESIAN_POINT ( 'NONE',  ( -32.50000000000000000, 52.60000000546235555, 10.55989012756946366 ) ) ;
#11499 = CARTESIAN_POINT ( 'NONE',  ( -13.91746824999999887, 71.37500000273116996, 0.000000000000000000 ) ) ;
#11500 = CARTESIAN_POINT ( 'NONE',  ( 33.58253175000000823, 34.02500000273118275, 10.91162601494192863 ) ) ;
#11501 = CARTESIAN_POINT ( 'NONE',  ( 26.29305231718578995, 77.70000000546239960, -19.10302069950538240 ) ) ;
#11502 = CARTESIAN_POINT ( 'NONE',  ( -20.75514604977248112, 59.67500000273118133, 28.56700777964554661 ) ) ;
#11503 = CARTESIAN_POINT ( 'NONE',  ( -2.092463501923844636E-15, 35.49999999999998579, -34.17252228774368916 ) ) ;
#11504 = CARTESIAN_POINT ( 'NONE',  ( 20.08610463437157279, 43.30000000000000426, -27.64615127144129758 ) ) ;
#11505 = CARTESIAN_POINT ( 'NONE',  ( 7.236395654485760609, 13.02499999726880375, -22.27133577429736633 ) ) ;
#11506 = CARTESIAN_POINT ( 'NONE',  ( -20.75514604977248823, 7.075000002731188786, -28.56700777964554305 ) ) ;
#11507 = CARTESIAN_POINT ( 'NONE',  ( 23.41746824999999887, 0.6249999972688102812, 0.000000000000000000 ) ) ;
#11508 = CARTESIAN_POINT ( 'NONE',  ( -4.300734207923759378, 78.97500000273122112, -13.23629886949340495 ) ) ;
#11509 = CARTESIAN_POINT ( 'NONE',  ( 20.75514604977249178, 72.07500000273120122, 28.56700777964553950 ) ) ;
#11510 = CARTESIAN_POINT ( 'NONE',  ( -4.223320258572819786E-15, 19.24999999453763166, 24.50000000000000000 ) ) ;
#11511 = CARTESIAN_POINT ( 'NONE',  ( 10.37757302488624767, 65.97500000273119269, 31.93888565452638417 ) ) ;
#11512 = ORIENTED_EDGE ( 'NONE', *, *, #841, .F. ) ;
#11513 = CARTESIAN_POINT ( 'NONE',  ( -7.570916362186215665, 7.149999994537637349, 23.30088464923126423 ) ) ;
#11514 = CARTESIAN_POINT ( 'NONE',  ( 27.95245687107222921, 64.85156249999998579, -2.463307335887066074E-13 ) ) ;
#11515 = CARTESIAN_POINT ( 'NONE',  ( 5.779280353836490358E-15, 75.00000000546236834, 32.49999999999999289 ) ) ;
#11516 = CARTESIAN_POINT ( 'NONE',  ( 27.16883889988623935, 48.32500000273119412, -19.73931689729374384 ) ) ;
#11517 = CARTESIAN_POINT ( 'NONE',  ( 20.75514604977248467, 12.67500000273118488, -28.56700777964554305 ) ) ;
#11518 = CARTESIAN_POINT ( 'NONE',  ( 33.58253175000000113, 60.37500000273120548, -4.112674001490185761E-15 ) ) ;
#11519 = CARTESIAN_POINT ( 'NONE',  ( -27.95245687107223276, 45.94531249999998579, 2.498001805406602216E-13 ) ) ;
#11520 = CARTESIAN_POINT ( 'NONE',  ( 0.04044903254992426173, 41.36756916759064495, -30.02300923189239867 ) ) ;
#11521 = CARTESIAN_POINT ( 'NONE',  ( -25.98046417659831420, 27.03347249907602290, 15.04653450569339945 ) ) ;
#11522 = CARTESIAN_POINT ( 'NONE',  ( -20.08610463437157989, 66.20000000546238539, -27.64615127144129758 ) ) ;
#11523 = CARTESIAN_POINT ( 'NONE',  ( 11.25946833292375793, 77.67500000273119554, 8.180482586598731842 ) ) ;
#11524 = CARTESIAN_POINT ( 'NONE',  ( 7.025853678916867295, 53.81732666574268364, 26.06988505166722803 ) ) ;
#11525 = CYLINDRICAL_SURFACE ( 'NONE', #25281, 32.50000000000000000 ) ;
#11526 = CARTESIAN_POINT ( 'NONE',  ( -3.880418787951142701, 17.44874571845315359, 24.49999999999999645 ) ) ;
#11527 = ORIENTED_EDGE ( 'NONE', *, *, #20920, .F. ) ;
#11528 = CARTESIAN_POINT ( 'NONE',  ( -33.58253175000000113, 41.37500000273118417, 0.000000000000000000 ) ) ;
#11529 = CARTESIAN_POINT ( 'NONE',  ( 23.41746824999999887, 3.024999997268813079, 7.608796670333735079 ) ) ;
#11530 = CARTESIAN_POINT ( 'NONE',  ( -32.50000000000000000, 32.50000000546236834, 0.000000000000000000 ) ) ;
#11531 = VERTEX_POINT ( 'NONE', #26805 ) ;
#11532 = CARTESIAN_POINT ( 'NONE',  ( -33.58253175000000113, 17.22500000273118559, 10.91162601494193929 ) ) ;
#11533 = CARTESIAN_POINT ( 'NONE',  ( 28.01184896238290278, 30.33333333333332860, -7.505752307973347470 ) ) ;
#11535 = EDGE_LOOP ( 'NONE', ( #395, #8289, #29593, #27174 ) ) ;
#11534 = EDGE_CURVE ( 'NONE', #9120, #9319, #31776, .T. ) ;
#11536 = CARTESIAN_POINT ( 'NONE',  ( -19.82091636218621034, 2.549999994537616388, -14.40073868116559552 ) ) ;
#11537 = CARTESIAN_POINT ( 'NONE',  ( -27.16883889988623935, 57.32500000273119412, 19.73931689729374739 ) ) ;
#11538 = CARTESIAN_POINT ( 'NONE',  ( -26.00068869287340334, 55.97135416666665719, 15.01150461594643382 ) ) ;
#11539 = ADVANCED_FACE ( 'NONE', ( #11027 ), #8108, .F. ) ;
#11540 = CARTESIAN_POINT ( 'NONE',  ( -32.50000000000000000, 12.60000000546236620, 10.55989012756946366 ) ) ;
#11541 = CARTESIAN_POINT ( 'NONE',  ( 19.82091636218621034, 15.54999999453762705, 14.40073868116559730 ) ) ;
#11542 = CARTESIAN_POINT ( 'NONE',  ( -4.523095164977117273E-15, 16.62499999726881583, 24.62258325217400312 ) ) ;
#11543 = CARTESIAN_POINT ( 'NONE',  ( 32.50000000000000000, 59.09999999999999432, -10.55989012756945833 ) ) ;
#11544 = CARTESIAN_POINT ( 'NONE',  ( -33.58253175000000113, 23.27500000273116854, -10.91162601494193218 ) ) ;
#11545 = CARTESIAN_POINT ( 'NONE',  ( 20.08610463437158344, 5.200000005462368513, 27.64615127144129403 ) ) ;
#11546 = CARTESIAN_POINT ( 'NONE',  ( -14.01125832528328985, 14.14284749907602290, -24.18731323226223040 ) ) ;
#11547 = CARTESIAN_POINT ( 'NONE',  ( 11.25946833292375793, 77.67500000273119554, 8.180482586598731842 ) ) ;
#11548 = CYLINDRICAL_SURFACE ( 'NONE', #875, 24.50000000000000000 ) ;
#11549 = CARTESIAN_POINT ( 'NONE',  ( 32.50000000000000711, 14.89999999999999503, 10.55989012756945122 ) ) ;
#11550 = CARTESIAN_POINT ( 'NONE',  ( 10.04305231718578817, 11.40000000000000746, -30.90933677959249337 ) ) ;
#11551 = ORIENTED_EDGE ( 'NONE', *, *, #22368, .T. ) ;
#11552 = CARTESIAN_POINT ( 'NONE',  ( -18.94512977948576093, 8.324999997268822227, 13.76444248337722698 ) ) ;
#11553 = CARTESIAN_POINT ( 'NONE',  ( -8.601468415847515203, 73.17500000273119554, 11.83890561707634959 ) ) ;
#11554 = CARTESIAN_POINT ( 'NONE',  ( 19.09188309203694800, 41.21875000000000000, 19.09188309203660694 ) ) ;
#11555 = CARTESIAN_POINT ( 'NONE',  ( -27.16883889988623935, 15.32500000273118168, 19.73931689729374739 ) ) ;
#11556 = CARTESIAN_POINT ( 'NONE',  ( -2.162160676586881955E-15, 66.62500000273118417, -35.31076352940723240 ) ) ;
#11557 = CARTESIAN_POINT ( 'NONE',  ( -10.37757302488623701, 31.77500000273118630, 31.93888565452638417 ) ) ;
#11558 = CARTESIAN_POINT ( 'NONE',  ( 20.75514604977248467, 16.67500000273117777, -28.56700777964554305 ) ) ;
#11559 = CARTESIAN_POINT ( 'NONE',  ( 20.75514604977249178, 6.075000002731190563, 28.56700777964553950 ) ) ;
#11560 = CARTESIAN_POINT ( 'NONE',  ( -7.543491769121417612, 12.29204833425730925, 28.00173670424549499 ) ) ;
#11561 = CARTESIAN_POINT ( 'NONE',  ( -7.505752307973343918, 53.53645833333332860, -28.01184896238290989 ) ) ;
#11562 = CARTESIAN_POINT ( 'NONE',  ( -15.00000000000000000, 82.00000000000001421, 0.000000000000000000 ) ) ;
#11563 = CARTESIAN_POINT ( 'NONE',  ( 11.25946833292375793, 74.57500000273120122, -8.180482586598735395 ) ) ;
#11564 = CARTESIAN_POINT ( 'NONE',  ( 32.50000000000000711, 48.89999999999999858, 10.55989012756945122 ) ) ;
#11565 = AXIS2_PLACEMENT_3D ( 'NONE', #4244, #14718, #20384 ) ;
#11566 = VECTOR ( 'NONE', #27370, 1000.000000000000227 ) ;
#11567 = CARTESIAN_POINT ( 'NONE',  ( 24.50000000000000000, 7.849999994537627757, -7.960532557706203605 ) ) ;
#11568 = CARTESIAN_POINT ( 'NONE',  ( 20.75514604977248467, 54.42500000273117422, -28.56700777964554305 ) ) ;
#11569 = CARTESIAN_POINT ( 'NONE',  ( 18.94512977948576093, 17.32499999726880446, -13.76444248337722875 ) ) ;
#11570 = EDGE_LOOP ( 'NONE', ( #10744, #5088, #21350, #21312 ) ) ;
#11571 = CARTESIAN_POINT ( 'NONE',  ( -27.16883889988624290, 67.17500000273118133, -19.73931689729374028 ) ) ;
#11572 =( BOUNDED_CURVE ( )  B_SPLINE_CURVE ( 2, ( #9037, #5801, #8367, #32039, #24165, #29623, #24653, #6126, #16445, #11611, #11446, #8538, #11125 ),
 .UNSPECIFIED., .F., .T. ) 
 B_SPLINE_CURVE_WITH_KNOTS ( ( 3, 2, 2, 2, 2, 2, 3 ),
 ( 0.2500000000000000000, 0.2512820512820512775, 0.2538461538461538325, 0.2564102564102563875, 0.2589743589743589980, 0.2615384615384615530, 0.2628205128205128305 ),
 .UNSPECIFIED. ) 
 CURVE ( )  GEOMETRIC_REPRESENTATION_ITEM ( )  RATIONAL_B_SPLINE_CURVE ( ( 0.9755282581475768211, 0.9755282581475768211, 1.000000000000000000, 0.9510565162951535312, 1.000000000000000000, 0.9510565162951535312, 1.000000000000000000, 0.9510565162951535312, 1.000000000000000000, 0.9510565162951535312, 1.000000000000000000, 0.9755282581475768211, 0.9755282581475768211 ) ) 
 REPRESENTATION_ITEM ( '' )  );
#11573 = CYLINDRICAL_SURFACE ( 'NONE', #25044, 32.50000000000000000 ) ;
#11574 = CARTESIAN_POINT ( 'NONE',  ( -14.47279130897152122, 7.924999997268803220, 19.92008829642072243 ) ) ;
#11575 = CARTESIAN_POINT ( 'NONE',  ( 24.18731323226247554, 21.88840250092397710, 14.01125832528285997 ) ) ;
#11576 = EDGE_LOOP ( 'NONE', ( #22905, #32811, #19966, #31299 ) ) ;
#11577 = CARTESIAN_POINT ( 'NONE',  ( 10.37757302488624767, 37.72500000273119980, 31.93888565452638417 ) ) ;
#11578 = LINE ( 'NONE', #20166, #4465 ) ;
#11579 = ORIENTED_EDGE ( 'NONE', *, *, #22904, .F. ) ;
#11580 = CARTESIAN_POINT ( 'NONE',  ( 20.50609665440969565, 47.23437499999999289, -20.50609665441004736 ) ) ;
#11581 = CARTESIAN_POINT ( 'NONE',  ( 10.37757302488624056, 60.77500000273117564, -31.93888565452638417 ) ) ;
#11582 = CARTESIAN_POINT ( 'NONE',  ( -3.880418787951127602, 2.551254281546845082, -24.50000000000000000 ) ) ;
#11583 = CARTESIAN_POINT ( 'NONE',  ( -27.16883889988624290, 74.92500000273119554, -19.73931689729374028 ) ) ;
#11584 = CARTESIAN_POINT ( 'NONE',  ( -30.02300923189239512, 28.75781249999999645, 2.654126918244515359E-13 ) ) ;
#11585 = CARTESIAN_POINT ( 'NONE',  ( -19.82091636218621389, 7.200000000000011724, 14.40073868116558842 ) ) ;
#11586 = EDGE_CURVE ( 'NONE', #4172, #9084, #26643, .T. ) ;
#11587 = CARTESIAN_POINT ( 'NONE',  ( 33.58253175000000823, 4.275000002731189852, 10.91162601494192863 ) ) ;
#11588 = ADVANCED_FACE ( 'NONE', ( #26641 ), #8607, .T. ) ;
#11589 = CARTESIAN_POINT ( 'NONE',  ( 10.37757302488624767, 15.72500000273119269, 31.93888565452638417 ) ) ;
#11590 = CARTESIAN_POINT ( 'NONE',  ( 0.04044903255045854962, 40.21055583240935505, 30.02300923189239867 ) ) ;
#11591 = AXIS2_PLACEMENT_3D ( 'NONE', #19533, #32881, #17128 ) ;
#11592 = CARTESIAN_POINT ( 'NONE',  ( -15.00000000000000000, 78.00000000000001421, 0.000000000000000000 ) ) ;
#11593 = CARTESIAN_POINT ( 'NONE',  ( -7.505752307972844761, 62.41666666666666430, 28.01184896238304134 ) ) ;
#11594 = CARTESIAN_POINT ( 'NONE',  ( -24.50000000000000000, 16.64999999453763735, -7.960532557706207157 ) ) ;
#11595 = CARTESIAN_POINT ( 'NONE',  ( -32.50000000000000000, 38.60000000546239107, 10.55989012756946366 ) ) ;
#11596 = CARTESIAN_POINT ( 'NONE',  ( 6.988114217768294445, 17.44270833333333215, 26.07999730980477437 ) ) ;
#11597 = CARTESIAN_POINT ( 'NONE',  ( 10.37757302488624056, 34.52500000273117564, -31.93888565452638417 ) ) ;
#11598 = CARTESIAN_POINT ( 'NONE',  ( -4.300734207923759378, 74.47500000273116427, -13.23629886949340495 ) ) ;
#11599 = CARTESIAN_POINT ( 'NONE',  ( 33.58253175000000823, 50.27500000273118985, 10.91162601494192863 ) ) ;
#11600 = CARTESIAN_POINT ( 'NONE',  ( -33.58253175000000113, 25.37500000273118417, 0.000000000000000000 ) ) ;
#11601 = CARTESIAN_POINT ( 'NONE',  ( 16.68329339294214364, 16.99999999999999289, 16.74724684563455313 ) ) ;
#11602 = CARTESIAN_POINT ( 'NONE',  ( 2.584737979205442066E-13, 27.89843749999999645, 27.95245687107223276 ) ) ;
#11603 = CARTESIAN_POINT ( 'NONE',  ( 19.82091636218621389, 11.94999999453763628, -14.40073868116559197 ) ) ;
#11604 = CARTESIAN_POINT ( 'NONE',  ( 0.000000000000000000, 80.00000000000001421, -32.50000000000000000 ) ) ;
#11605 = CARTESIAN_POINT ( 'NONE',  ( -32.50000000000000000, 67.99999999999998579, 0.000000000000000000 ) ) ;
#11606 = CARTESIAN_POINT ( 'NONE',  ( 27.16883889988623935, 6.325000002731187898, -19.73931689729374384 ) ) ;
#11607 = CARTESIAN_POINT ( 'NONE',  ( -18.94512977948575738, 13.42499999726881654, -13.76444248337723231 ) ) ;
#11608 = CARTESIAN_POINT ( 'NONE',  ( 28.02196122052058413, 25.74440999907601935, 7.468012846824272799 ) ) ;
#11609 = CARTESIAN_POINT ( 'NONE',  ( 24.49999999999999645, -16.99999999999999289, 0.000000000000000000 ) ) ;
#11610 = CARTESIAN_POINT ( 'NONE',  ( -27.95245687107223986, 30.75743083240935505, 0.04044903255043252877 ) ) ;
#11611 = CARTESIAN_POINT ( 'NONE',  ( -20.08610463437157989, 59.70000000000000284, -27.64615127144129758 ) ) ;
#11612 = CARTESIAN_POINT ( 'NONE',  ( 10.37757302488624767, 11.72500000273118914, 31.93888565452638417 ) ) ;
#11613 = CARTESIAN_POINT ( 'NONE',  ( 14.47279130897151589, 2.824999997268819119, 19.92008829642072953 ) ) ;
#11614 = CARTESIAN_POINT ( 'NONE',  ( -27.95245687107222921, 52.82031249999997868, 2.498001805406602216E-13 ) ) ;
#11615 = ORIENTED_EDGE ( 'NONE', *, *, #33703, .F. ) ;
#11616 = CARTESIAN_POINT ( 'NONE',  ( -10.37757302488624411, 58.72500000273119269, -31.93888565452638417 ) ) ;
#11617 = CARTESIAN_POINT ( 'NONE',  ( 27.16883889988623935, 30.57500000273117990, -19.73931689729374384 ) ) ;
#11618 = ORIENTED_EDGE ( 'NONE', *, *, #23499, .F. ) ;
#11619 = CARTESIAN_POINT ( 'NONE',  ( -7.505752307973343918, 26.03645833333333215, -28.01184896238290989 ) ) ;
#11620 = CARTESIAN_POINT ( 'NONE',  ( 28.00173670424549499, 21.74517333425730925, 7.543491769121417612 ) ) ;
#11621 = CARTESIAN_POINT ( 'NONE',  ( -24.50000000000001066, 18.84999999453762953, 7.960532557706201828 ) ) ;
#11622 = CARTESIAN_POINT ( 'NONE',  ( 23.41746824999999887, 2.624999997268812280, 0.000000000000000000 ) ) ;
#11623 = CARTESIAN_POINT ( 'NONE',  ( -33.58253175000000113, 21.27500000273117209, -10.91162601494193218 ) ) ;
#11624 = CARTESIAN_POINT ( 'NONE',  ( 10.04305231718578817, 31.90000000546239178, -30.90933677959249337 ) ) ;
#11625 = CARTESIAN_POINT ( 'NONE',  ( -32.50000000000000000, 74.10000000000002274, 10.55989012756946366 ) ) ;
#11626 = CARTESIAN_POINT ( 'NONE',  ( 10.04305231718578817, 47.90000000546238113, -30.90933677959249337 ) ) ;
#11627 = CARTESIAN_POINT ( 'NONE',  ( 20.08610463437158344, 37.20000000546237828, 27.64615127144129403 ) ) ;
#11628 = CARTESIAN_POINT ( 'NONE',  ( 15.04653450569292872, 51.96652750092398065, -25.98046417659857710 ) ) ;
#11629 = CARTESIAN_POINT ( 'NONE',  ( -33.58253175000000113, 35.47500000273118559, 10.91162601494193929 ) ) ;
#11630 = CARTESIAN_POINT ( 'NONE',  ( -27.16883889988623935, 55.32500000273120122, 19.73931689729374739 ) ) ;
#11631 = CARTESIAN_POINT ( 'NONE',  ( -7.505752307972844761, 24.60416666666666430, 28.01184896238304134 ) ) ;
#11632 = PRESENTATION_STYLE_ASSIGNMENT (( #14384 ) ) ;
#11633 = CARTESIAN_POINT ( 'NONE',  ( 1.507698388325705758E-15, 9.624999997268808727, -24.62258325217400312 ) ) ;
#11634 = CARTESIAN_POINT ( 'NONE',  ( 26.29305231718579350, 12.79999999999997762, 19.10302069950537529 ) ) ;
#11635 = CARTESIAN_POINT ( 'NONE',  ( -7.570916362186215665, 11.39999999999999325, 23.30088464923126423 ) ) ;
#11636 = CARTESIAN_POINT ( 'NONE',  ( -26.06988505166722803, 40.92670166574268364, 7.025853678916877953 ) ) ;
#11637 = CARTESIAN_POINT ( 'NONE',  ( -27.16883889988623935, 55.32500000273118701, 19.73931689729374739 ) ) ;
#11638 = CARTESIAN_POINT ( 'NONE',  ( 20.75514604977248467, 50.67500000273117422, -28.56700777964554305 ) ) ;
#11639 = CARTESIAN_POINT ( 'NONE',  ( -18.94512977948575738, 7.424999997268811214, -13.76444248337723231 ) ) ;
#11640 = CARTESIAN_POINT ( 'NONE',  ( 15.14183272437242422, 4.049999994537630599, -20.84094480462497856 ) ) ;
#11641 = CARTESIAN_POINT ( 'NONE',  ( 33.58253175000000113, 4.225000002731190030, -10.91162601494193751 ) ) ;
#11642 = CARTESIAN_POINT ( 'NONE',  ( 19.06425588902592239, 42.65663166759063785, 19.11951029504763611 ) ) ;
#11643 = CARTESIAN_POINT ( 'NONE',  ( 9.706506667267825961, 16.99999999999998934, -21.32484505899611449 ) ) ;
#11644 = CARTESIAN_POINT ( 'NONE',  ( 24.50000000000000000, 4.099999999999986322, -7.960532557706203605 ) ) ;
#11645 = UNCERTAINTY_MEASURE_WITH_UNIT (LENGTH_MEASURE( 1.000000000000000082E-05 ), #8558, 'distance_accuracy_value', 'NONE');
#11646 = CARTESIAN_POINT ( 'NONE',  ( 27.16883889988624290, 25.92500000273119554, 19.73931689729373673 ) ) ;
#11647 = CARTESIAN_POINT ( 'NONE',  ( 4.349545668204547685E-15, -58.51673569255127205, 0.000000000000000000 ) ) ;
#11648 = CARTESIAN_POINT ( 'NONE',  ( 0.000000000000000000, -12.99999999999999822, 0.000000000000000000 ) ) ;
#11649 = CARTESIAN_POINT ( 'NONE',  ( 2.489536152421872915E-14, 74.00000000546238255, -32.49999999999999289 ) ) ;
#11650 = CARTESIAN_POINT ( 'NONE',  ( 20.53372385742108008, 60.40586833240935505, 20.47846945139866648 ) ) ;
#11651 = CARTESIAN_POINT ( 'NONE',  ( -20.08610463437157989, 48.20000000546237828, -27.64615127144129758 ) ) ;
#11652 = SURFACE_STYLE_FILL_AREA ( #16984 ) ;
#11653 = AXIS2_PLACEMENT_3D ( 'NONE', #335, #13899, #16315 ) ;
#11654 = CARTESIAN_POINT ( 'NONE',  ( -24.20753774853730889, 25.03385416666666785, 13.97622843553633842 ) ) ;
#11655 = ORIENTED_EDGE ( 'NONE', *, *, #11053, .T. ) ;
#11656 = AXIS2_PLACEMENT_3D ( 'NONE', #20336, #12950, #5052 ) ;
#11657 = CARTESIAN_POINT ( 'NONE',  ( -2.162160676586881955E-15, 76.62500000273118417, -35.31076352940723240 ) ) ;
#11658 = CARTESIAN_POINT ( 'NONE',  ( -26.00068869287340334, 35.34635416666666430, 15.01150461594643382 ) ) ;
#11659 = CARTESIAN_POINT ( 'NONE',  ( 0.000000000000000000, 70.00000000000000000, 0.000000000000000000 ) ) ;
#11660 = ORIENTED_EDGE ( 'NONE', *, *, #33984, .F. ) ;
#11661 = CARTESIAN_POINT ( 'NONE',  ( 20.47846945139902530, 49.53163166759063785, 20.53372385742071771 ) ) ;
#11662 = CARTESIAN_POINT ( 'NONE',  ( 6.277390505771533514E-15, 9.000000005462378994, 34.17252228774368916 ) ) ;
#11663 = CARTESIAN_POINT ( 'NONE',  ( -26.00068869287368756, 59.98177083333332149, -15.01150461594595775 ) ) ;
#11664 = CARTESIAN_POINT ( 'NONE',  ( -17.29030653276320351, 16.99999999999998579, 17.35785989121602668 ) ) ;
#11665 = CARTESIAN_POINT ( 'NONE',  ( -2.162160676586881955E-15, 48.87500000273117706, -35.31076352940723240 ) ) ;
#11666 = CARTESIAN_POINT ( 'NONE',  ( 10.04305231718578817, 51.90000000546238113, -30.90933677959249337 ) ) ;
#11667 = EDGE_CURVE ( 'NONE', #19806, #30412, #5817, .T. ) ;
#11668 = CARTESIAN_POINT ( 'NONE',  ( 2.897257156509938333E-15, 80.50000000000002842, 15.77193336357400710 ) ) ;
#11669 = CARTESIAN_POINT ( 'NONE',  ( -27.16883889988623935, 31.32500000273119412, 19.73931689729374739 ) ) ;
#11670 = CARTESIAN_POINT ( 'NONE',  ( 19.82091636218621389, 12.19999999999998863, -14.40073868116559197 ) ) ;
#11671 = CARTESIAN_POINT ( 'NONE',  ( -33.58253175000000113, 57.37500000273118417, 0.000000000000000000 ) ) ;
#11672 = CARTESIAN_POINT ( 'NONE',  ( 20.08610463437157279, 35.29999999999999716, -27.64615127144129758 ) ) ;
#11673 = CARTESIAN_POINT ( 'NONE',  ( 26.29305231718579350, 34.79999999999999716, 19.10302069950537529 ) ) ;
#11674 = CARTESIAN_POINT ( 'NONE',  ( -23.41746825000000243, 13.52499999726880198, -7.608796670333730638 ) ) ;
#11675 = CARTESIAN_POINT ( 'NONE',  ( 27.16883889988623935, 4.575000002731199444, -19.73931689729374384 ) ) ;
#11676 = CARTESIAN_POINT ( 'NONE',  ( 32.50000000000000000, 13.00000000000001066, -3.980102097228898626E-15 ) ) ;
#11677 = CARTESIAN_POINT ( 'NONE',  ( 4.300734207923761154, 79.97500000273122112, 13.23629886949340495 ) ) ;
#11678 = CARTESIAN_POINT ( 'NONE',  ( 33.58253175000000113, 64.37500000273119838, -4.112674001490185761E-15 ) ) ;
#11679 = AXIS2_PLACEMENT_3D ( 'NONE', #9264, #4126, #27129 ) ;
#11680 = ORIENTED_EDGE ( 'NONE', *, *, #21696, .T. ) ;
#11681 = CARTESIAN_POINT ( 'NONE',  ( 15.14183272437242245, 2.049999994537635484, -20.84094480462497856 ) ) ;
#11682 = CARTESIAN_POINT ( 'NONE',  ( -24.22776226481240514, 12.72173583425731458, 13.94119854578937812 ) ) ;
#11683 = CYLINDRICAL_SURFACE ( 'NONE', #26133, 15.00000000000000000 ) ;
#11684 = CARTESIAN_POINT ( 'NONE',  ( 10.37757302488624056, 48.52500000273117564, -31.93888565452638417 ) ) ;
#11685 = CARTESIAN_POINT ( 'NONE',  ( 6.486482029760649416E-15, 7.875000002731177950, 35.31076352940723240 ) ) ;
#11686 = CARTESIAN_POINT ( 'NONE',  ( -2.162160676586882350E-15, 62.87500000273120548, -35.31076352940722529 ) ) ;
#11687 = CARTESIAN_POINT ( 'NONE',  ( -19.09188309203660694, 48.95312500000000000, 19.09188309203694800 ) ) ;
#11688 = CARTESIAN_POINT ( 'NONE',  ( 14.97647472619947351, 35.92486083425730214, 26.02091320914850314 ) ) ;
#11689 = CARTESIAN_POINT ( 'NONE',  ( 7.468012846824281681, 24.88503499907601935, -28.02196122052058058 ) ) ;
#11690 = CARTESIAN_POINT ( 'NONE',  ( 26.29305231718579350, 69.30000000546236549, 19.10302069950537529 ) ) ;
#11691 = CARTESIAN_POINT ( 'NONE',  ( 1.093617666956751375E-13, 67.50000000000000000, -32.50000000000000711 ) ) ;
#11692 = CARTESIAN_POINT ( 'NONE',  ( 27.95245687107223276, 53.10118083240936215, -0.04044903255042905932 ) ) ;
#11693 = DIRECTION ( 'NONE',  ( -0.000000000000000000, 1.000000000000000000, -0.000000000000000000 ) ) ;
#11694 = CARTESIAN_POINT ( 'NONE',  ( -15.14183272437242778, 17.30000000000000782, 20.84094480462497856 ) ) ;
#11695 = ORIENTED_EDGE ( 'NONE', *, *, #2230, .T. ) ;
#11696 = CARTESIAN_POINT ( 'NONE',  ( 6.486482029760649416E-15, 43.87500000273118417, 35.31076352940723240 ) ) ;
#11697 = CARTESIAN_POINT ( 'NONE',  ( 14.47279130897151944, 3.424999997268799667, -19.92008829642072598 ) ) ;
#11698 = CARTESIAN_POINT ( 'NONE',  ( -32.50000000000000000, 30.50000000546236478, 0.000000000000000000 ) ) ;
#11699 = EDGE_LOOP ( 'NONE', ( #13830, #9501 ) ) ;
#11700 = CIRCLE ( 'NONE', #187, 12.00000000000000178 ) ;
#11701 = CARTESIAN_POINT ( 'NONE',  ( 20.50609665441005092, 30.90624999999999645, 20.50609665440969209 ) ) ;
#11702 = EDGE_LOOP ( 'NONE', ( #17933, #32295, #4024, #12425 ) ) ;
#11703 = VERTEX_POINT ( 'NONE', #31447 ) ;
#11704 = CARTESIAN_POINT ( 'NONE',  ( -10.04305231718578462, 56.40000000000000568, 30.90933677959249337 ) ) ;
#11705 = CARTESIAN_POINT ( 'NONE',  ( 10.37757302488624056, 48.52500000273118985, -31.93888565452638417 ) ) ;
#11706 = CARTESIAN_POINT ( 'NONE',  ( 15.01150461594596308, 53.96614583333333570, -26.00068869287367335 ) ) ;
#11707 = CARTESIAN_POINT ( 'NONE',  ( -32.50000000000000000, 10.60000000546237331, 10.55989012756946366 ) ) ;
#11708 = CARTESIAN_POINT ( 'NONE',  ( -4.223320258572819786E-15, 15.24999999453762278, 24.50000000000000000 ) ) ;
#11709 = CARTESIAN_POINT ( 'NONE',  ( 23.41746824999999887, 13.22499999726881192, -7.608796670333727974 ) ) ;
#11710 = CARTESIAN_POINT ( 'NONE',  ( -20.08610463437156923, 54.30000000000000426, 27.64615127144130113 ) ) ;
#11711 = CARTESIAN_POINT ( 'NONE',  ( 20.75514604977249178, 24.07500000273120122, 28.56700777964553950 ) ) ;
#11712 = LINE ( 'NONE', #27505, #1961 ) ;
#11713 = CARTESIAN_POINT ( 'NONE',  ( 19.06425588902558133, 14.85899333240935505, -19.11951029504797006 ) ) ;
#11714 = CARTESIAN_POINT ( 'NONE',  ( -13.91746824999999887, 72.87500000273119838, 0.000000000000000000 ) ) ;
#11715 = CARTESIAN_POINT ( 'NONE',  ( -26.29305231718579350, 55.80000000000000426, -19.10302069950537884 ) ) ;
#11716 = CARTESIAN_POINT ( 'NONE',  ( -1.778240108872766143E-15, 28.00000000546237544, -32.49999999999999289 ) ) ;
#11717 = CARTESIAN_POINT ( 'NONE',  ( 6.277390505771533514E-15, 6.499999999999998224, 34.17252228774368916 ) ) ;
#11718 = ORIENTED_EDGE ( 'NONE', *, *, #27471, .F. ) ;
#11719 = CARTESIAN_POINT ( 'NONE',  ( -7.236395654485763274, 8.524999997268828622, 22.27133577429736633 ) ) ;
#11720 = CARTESIAN_POINT ( 'NONE',  ( 32.50000000000000000, 71.50000000546235412, -3.980102097228898626E-15 ) ) ;
#11721 = CARTESIAN_POINT ( 'NONE',  ( -19.09188309203660694, 42.07812499999999289, 19.09188309203694800 ) ) ;
#11722 = CARTESIAN_POINT ( 'NONE',  ( -20.75514604977248112, 65.42500000273118133, 28.56700777964554661 ) ) ;
#11723 = CARTESIAN_POINT ( 'NONE',  ( -27.16883889988624290, 29.17500000273119554, -19.73931689729374028 ) ) ;
#11724 = AXIS2_PLACEMENT_3D ( 'NONE', #9792, #1374, #20268 ) ;
#11725 = CARTESIAN_POINT ( 'NONE',  ( 6.486482029760649416E-15, 13.87500000273117529, 35.31076352940723240 ) ) ;
#11726 = CARTESIAN_POINT ( 'NONE',  ( 27.16883889988623935, 10.57500000273120477, -19.73931689729374384 ) ) ;
#11727 = CARTESIAN_POINT ( 'NONE',  ( -27.95245687107223986, 64.57069416759065916, -0.04044903254993292840 ) ) ;
#11728 = CARTESIAN_POINT ( 'NONE',  ( -7.505752307973343918, 50.09895833333332860, -28.01184896238290989 ) ) ;
#11729 = CARTESIAN_POINT ( 'NONE',  ( 5.147494310547434893, 3.051254287009221411, 32.49999999999999289 ) ) ;
#11730 = EDGE_CURVE ( 'NONE', #33131, #25303, #7939, .T. ) ;
#11731 = CARTESIAN_POINT ( 'NONE',  ( 2.688165632520823219E-15, 77.87500000273118417, 14.63369212191046209 ) ) ;
#11732 = CARTESIAN_POINT ( 'NONE',  ( -20.08610463437157989, 49.70000000000000284, -27.64615127144129758 ) ) ;
#11733 = CARTESIAN_POINT ( 'NONE',  ( -19.82091636218621034, 2.549999994537616388, -14.40073868116559552 ) ) ;
#11734 = CARTESIAN_POINT ( 'NONE',  ( -33.58253175000000113, 51.22500000273119269, 10.91162601494193929 ) ) ;
#11735 = ADVANCED_FACE ( 'NONE', ( #24890 ), #28613, .F. ) ;
#11736 = CARTESIAN_POINT ( 'NONE',  ( 18.94512977948575738, 4.424999997268807661, 13.76444248337723408 ) ) ;
#11737 = ORIENTED_EDGE ( 'NONE', *, *, #6084, .T. ) ;
#11738 = CARTESIAN_POINT ( 'NONE',  ( -10.37757302488624411, 60.97500000273119269, -31.93888565452638417 ) ) ;
#11739 = CARTESIAN_POINT ( 'NONE',  ( 0.000000000000000000, 80.00000000000001421, 0.000000000000000000 ) ) ;
#11740 = CARTESIAN_POINT ( 'NONE',  ( 23.41746825000000243, 14.52499999726880020, 7.608796670333735079 ) ) ;
#11741 = CARTESIAN_POINT ( 'NONE',  ( -13.94119854578936923, 34.20611083425730925, -24.22776226481241224 ) ) ;
#11742 = VERTEX_POINT ( 'NONE', #22610 ) ;
#11743 = CARTESIAN_POINT ( 'NONE',  ( 27.16883889988623935, 30.32500000273117990, -19.73931689729374384 ) ) ;
#11744 = CARTESIAN_POINT ( 'NONE',  ( 0.000000000000000000, 0.000000000000000000, 24.50000000000000000 ) ) ;
#11745 = AXIS2_PLACEMENT_3D ( 'NONE', #12313, #33588, #2012 ) ;
#11746 = VERTEX_POINT ( 'NONE', #33063 ) ;
#11747 = CARTESIAN_POINT ( 'NONE',  ( 2.740863092043355209E-13, 48.52343750000000000, 30.02300923189239512 ) ) ;
#11748 = CARTESIAN_POINT ( 'NONE',  ( -33.58253175000000113, 61.27500000273118985, -10.91162601494193218 ) ) ;
#11749 = CARTESIAN_POINT ( 'NONE',  ( -15.00000000000000000, 75.89999999999996305, -4.873795443493594171 ) ) ;
#11750 = CARTESIAN_POINT ( 'NONE',  ( -33.58253175000000113, 73.02500000273120406, -10.91162601494193218 ) ) ;
#11751 = CARTESIAN_POINT ( 'NONE',  ( -20.50609665441004736, 32.62500000000000000, -20.50609665440969565 ) ) ;
#11752 = CARTESIAN_POINT ( 'NONE',  ( -7.570916362186210335, 4.599999999999992539, -23.30088464923126779 ) ) ;
#11753 = DIRECTION ( 'NONE',  ( 0.000000000000000000, -1.000000000000000000, 0.000000000000000000 ) ) ;
#11754 = CARTESIAN_POINT ( 'NONE',  ( -10.37757302488624411, 16.72500000273119269, -31.93888565452638417 ) ) ;
#11755 = CARTESIAN_POINT ( 'NONE',  ( -13.91746824999999532, 74.97500000273116427, 4.522059556121122093 ) ) ;
#11756 = CARTESIAN_POINT ( 'NONE',  ( -20.47846945139866648, 44.07774333240935505, 20.53372385742108008 ) ) ;
#11757 = CARTESIAN_POINT ( 'NONE',  ( -9.270509831248425314, 79.70000000000000284, -12.75976212528059861 ) ) ;
#11758 = CARTESIAN_POINT ( 'NONE',  ( 28.01184896238304134, 58.11979166666665719, 7.505752307972846538 ) ) ;
#11759 = CARTESIAN_POINT ( 'NONE',  ( -7.570916362186215665, 9.149999994537639125, 23.30088464923126423 ) ) ;
#11760 = CARTESIAN_POINT ( 'NONE',  ( 24.50000000000000355, 9.649999994537628467, 7.960532557706212486 ) ) ;
#11761 = CARTESIAN_POINT ( 'NONE',  ( 9.270509831248425314, 78.95000000546239960, 12.75976212528059683 ) ) ;
#11762 = CARTESIAN_POINT ( 'NONE',  ( -13.97622843553632421, 12.14322916666666430, -24.20753774853731599 ) ) ;
#11763 = CARTESIAN_POINT ( 'NONE',  ( -27.16883889988623935, 37.32500000273120122, 19.73931689729374739 ) ) ;
#11764 = CARTESIAN_POINT ( 'NONE',  ( 13.91746825000000065, 73.77500000273116143, 4.522059556121114987 ) ) ;
#11765 = CARTESIAN_POINT ( 'NONE',  ( -33.58253175000000113, 49.27500000273118985, -10.91162601494193218 ) ) ;
#11766 = CARTESIAN_POINT ( 'NONE',  ( -27.16883889988624290, 29.17500000273118133, -19.73931689729374028 ) ) ;
#11767 = CARTESIAN_POINT ( 'NONE',  ( 0.000000000000000000, 80.00000000000001421, -32.50000000000000000 ) ) ;
#11768 = CARTESIAN_POINT ( 'NONE',  ( 26.07999730980490227, 34.05729166666666430, 6.988114217767821046 ) ) ;
#11769 = CARTESIAN_POINT ( 'NONE',  ( -32.50000000000000000, 17.89999999999998437, -10.55989012756945300 ) ) ;
#11770 = STYLED_ITEM ( 'NONE', ( #10657 ), #32129 ) ;
#11771 = EDGE_CURVE ( 'NONE', #30131, #5051, #25203, .T. ) ;
#11772 = CARTESIAN_POINT ( 'NONE',  ( 4.635254915624212657, 80.60000000000000853, 14.26584774442730286 ) ) ;
#11773 =( BOUNDED_CURVE ( )  B_SPLINE_CURVE ( 2, ( #19185, #16943, #6470, #31870, #3067, #3232, #5968, #16281, #26739, #24492, #3557, #27063, #21922 ),
 .UNSPECIFIED., .F., .T. ) 
 B_SPLINE_CURVE_WITH_KNOTS ( ( 3, 2, 2, 2, 2, 2, 3 ),
 ( 0.6944444444444444198, 0.6999999999999999556, 0.7111111111111111382, 0.7222222222222222099, 0.7333333333333332815, 0.7444444444444444642, 0.7500000000000000000 ),
 .UNSPECIFIED. ) 
 CURVE ( )  GEOMETRIC_REPRESENTATION_ITEM ( )  RATIONAL_B_SPLINE_CURVE ( ( 0.9755282581475768211, 0.9755282581475768211, 1.000000000000000000, 0.9510565162951535312, 1.000000000000000000, 0.9510565162951535312, 1.000000000000000000, 0.9510565162951535312, 1.000000000000000000, 0.9510565162951535312, 1.000000000000000000, 0.9755282581475768211, 0.9755282581475768211 ) ) 
 REPRESENTATION_ITEM ( '' )  );
#11774 = CARTESIAN_POINT ( 'NONE',  ( 32.50000000000000711, 64.89999999999997726, 10.55989012756945122 ) ) ;
#11775 = CARTESIAN_POINT ( 'NONE',  ( -14.47279130897151767, 11.32499999726881157, -19.92008829642072598 ) ) ;
#11776 = CARTESIAN_POINT ( 'NONE',  ( 0.04044903255045854962, 29.89805583240935860, 30.02300923189239867 ) ) ;
#11777 = CARTESIAN_POINT ( 'NONE',  ( -14.47279130897151589, 3.824999997268816454, -19.92008829642072598 ) ) ;
#11778 = CARTESIAN_POINT ( 'NONE',  ( 0.04044903255044120238, 36.77305583240936215, 27.95245687107223276 ) ) ;
#11779 = CARTESIAN_POINT ( 'NONE',  ( 20.75514604977248467, 76.67500000273116711, -28.56700777964554305 ) ) ;
#11780 = CARTESIAN_POINT ( 'NONE',  ( 33.58253175000000823, 14.02500000273117209, 10.91162601494192685 ) ) ;
#11781 = CARTESIAN_POINT ( 'NONE',  ( 1.507698388325705758E-15, 5.624999997268818497, -24.62258325217400312 ) ) ;
#11782 = CARTESIAN_POINT ( 'NONE',  ( -19.06425588902591173, 10.00038166759064140, -19.11951029504763611 ) ) ;
#11783 = ORIENTED_EDGE ( 'NONE', *, *, #14919, .T. ) ;
#11784 = CARTESIAN_POINT ( 'NONE',  ( 20.75514604977248467, 58.42500000273119554, -28.56700777964554305 ) ) ;
#11785 = CARTESIAN_POINT ( 'NONE',  ( -20.75514604977248823, 29.07500000273119056, -28.56700777964554305 ) ) ;
#11786 = VERTEX_POINT ( 'NONE', #2876 ) ;
#11787 = CARTESIAN_POINT ( 'NONE',  ( -30.02300923189239512, 25.32031250000000000, 2.654126918244515359E-13 ) ) ;
#11788 = CARTESIAN_POINT ( 'NONE',  ( -28.02196122052045268, 26.61496500092397355, 7.468012846824790607 ) ) ;
#11789 = VECTOR ( 'NONE', #24932, 1000.000000000000000 ) ;
#11790 = CARTESIAN_POINT ( 'NONE',  ( -20.75514604977248112, 1.425000002731191984, 28.56700777964554661 ) ) ;
#11791 = CARTESIAN_POINT ( 'NONE',  ( 24.50000000000000355, 17.64999999453763380, 7.960532557706212486 ) ) ;
#11792 = CARTESIAN_POINT ( 'NONE',  ( -7.236395654485763274, 6.024999997268825958, 22.27133577429736633 ) ) ;
#11793 = CARTESIAN_POINT ( 'NONE',  ( 10.37757302488624056, 20.77500000273119340, -31.93888565452638417 ) ) ;
#11794 = AXIS2_PLACEMENT_3D ( 'NONE', #3405, #19691, #11458 ) ;
#11795 = CARTESIAN_POINT ( 'NONE',  ( 32.50000000000000000, 25.50000000546237544, -3.980102097228898626E-15 ) ) ;
#11796 = CARTESIAN_POINT ( 'NONE',  ( 26.29305231718578995, 75.19999999999998863, -19.10302069950538240 ) ) ;
#11797 = FACE_OUTER_BOUND ( 'NONE', #12636, .T. ) ;
#11798 = CARTESIAN_POINT ( 'NONE',  ( -14.60862552821003213, 74.00000000000002842, 2.946899241987215756 ) ) ;
#11799 = CARTESIAN_POINT ( 'NONE',  ( 25.98046417659858420, 52.82590250092398065, 15.04653450569292872 ) ) ;
#11800 = CARTESIAN_POINT ( 'NONE',  ( 20.75514604977249178, 36.07500000273117990, 28.56700777964553950 ) ) ;
#11801 = CARTESIAN_POINT ( 'NONE',  ( 33.58253175000000113, 58.12500000273116996, -4.112674001490185761E-15 ) ) ;
#11802 = CARTESIAN_POINT ( 'NONE',  ( 2.740863092043355209E-13, 27.89843749999999645, 30.02300923189239867 ) ) ;
#11803 =( NAMED_UNIT ( * ) PLANE_ANGLE_UNIT ( ) SI_UNIT ( $, .RADIAN. ) );
#11804 = CARTESIAN_POINT ( 'NONE',  ( -7.236395654485763274, 10.52499999726880198, 22.27133577429736633 ) ) ;
#11805 = CARTESIAN_POINT ( 'NONE',  ( -10.04305231718579172, 11.59999999999999964, -30.90933677959248982 ) ) ;
#11806 = CARTESIAN_POINT ( 'NONE',  ( -19.82091636218621034, 10.80000000000000426, -14.40073868116559552 ) ) ;
#11807 = CARTESIAN_POINT ( 'NONE',  ( -26.09010956794245217, 41.21315999907602645, -6.950374756619243755 ) ) ;
#11808 = CARTESIAN_POINT ( 'NONE',  ( -33.58253175000000113, 59.12500000273118417, 0.000000000000000000 ) ) ;
#11809 = VECTOR ( 'NONE', #865, 1000.000000000000114 ) ;
#11810 = AXIS2_PLACEMENT_3D ( 'NONE', #3349, #5755, #18807 ) ;
#11811 = CARTESIAN_POINT ( 'NONE',  ( 33.58253175000000113, 44.37500000273119838, -4.112674001490185761E-15 ) ) ;
#11812 = CARTESIAN_POINT ( 'NONE',  ( -23.41746825000000243, 7.724999997268811036, 7.608796670333725309 ) ) ;
#11813 = CARTESIAN_POINT ( 'NONE',  ( 0.000000000000000000, 0.000000000000000000, 24.50000000000000000 ) ) ;
#11814 = CARTESIAN_POINT ( 'NONE',  ( -1.778240108872766143E-15, 46.00000000546238255, -32.49999999999999289 ) ) ;
#11815 = CARTESIAN_POINT ( 'NONE',  ( 7.025853678916403666, 51.82329833425730925, -26.06988505166735237 ) ) ;
#11816 = CARTESIAN_POINT ( 'NONE',  ( -24.50000000000000000, 16.99999999999998579, -3.000384657911015469E-15 ) ) ;
#11817 = DIRECTION ( 'NONE',  ( -0.000000000000000000, -1.000000000000000000, -0.000000000000000000 ) ) ;
#11818 = CARTESIAN_POINT ( 'NONE',  ( 33.58253175000000823, 20.02500000273118275, 10.91162601494192863 ) ) ;
#11819 = CARTESIAN_POINT ( 'NONE',  ( 0.000000000000000000, 80.00000000000001421, 0.000000000000000000 ) ) ;
#11820 = CARTESIAN_POINT ( 'NONE',  ( 1.093617666956751375E-13, 61.50000000000000711, -32.50000000000000711 ) ) ;
#11821 = CARTESIAN_POINT ( 'NONE',  ( -25.98046417659831420, 64.84597249907602645, 15.04653450569339945 ) ) ;
#11822 = CARTESIAN_POINT ( 'NONE',  ( 32.50000000000000711, 45.40000000546237402, 10.55989012756945122 ) ) ;
#11823 = DIRECTION ( 'NONE',  ( -0.000000000000000000, -1.000000000000000000, -0.000000000000000000 ) ) ;
#11824 = CARTESIAN_POINT ( 'NONE',  ( -33.58253175000000113, 31.02500000273118630, -10.91162601494193041 ) ) ;
#11825 = CARTESIAN_POINT ( 'NONE',  ( -26.07999730980490583, 22.02604166666666430, -6.988114217767815717 ) ) ;
#11826 = ORIENTED_EDGE ( 'NONE', *, *, #27766, .F. ) ;
#11827 = CARTESIAN_POINT ( 'NONE',  ( 27.16883889988624290, 77.92500000273118133, 19.73931689729373673 ) ) ;
#11828 = CARTESIAN_POINT ( 'NONE',  ( 15.01150461594596308, 43.65364583333332860, -26.00068869287367335 ) ) ;
#11829 = CARTESIAN_POINT ( 'NONE',  ( 4.445600272181915325E-13, 26.00000000546237189, -32.50000000000000000 ) ) ;
#11830 = VERTEX_POINT ( 'NONE', #32312 ) ;
#11831 = CARTESIAN_POINT ( 'NONE',  ( -20.47846945139902175, 47.81288166759064495, -20.53372385742072481 ) ) ;
#11832 = CARTESIAN_POINT ( 'NONE',  ( 20.08610463437157279, 13.80000000546235839, -27.64615127144129758 ) ) ;
#11833 = CARTESIAN_POINT ( 'NONE',  ( -20.50609665440969209, 59.26562500000000000, 20.50609665441005092 ) ) ;
#11834 = CARTESIAN_POINT ( 'NONE',  ( 5.147494310547434893, 20.55125428154684286, 32.49999999999999289 ) ) ;
#11835 = CARTESIAN_POINT ( 'NONE',  ( 10.37757302488624767, 43.97500000273119269, 31.93888565452638417 ) ) ;
#11836 = CARTESIAN_POINT ( 'NONE',  ( 26.29305231718578995, 47.70000000546237118, -19.10302069950538240 ) ) ;
#11837 = CARTESIAN_POINT ( 'NONE',  ( -8.601468415847515203, 71.67500000273116711, 11.83890561707634959 ) ) ;
#11838 = CARTESIAN_POINT ( 'NONE',  ( -10.37757302488624411, 28.72500000273120335, -31.93888565452638417 ) ) ;
#11839 = CARTESIAN_POINT ( 'NONE',  ( 0.000000000000000000, 80.00000000000001421, -32.50000000000000000 ) ) ;
#11840 = CARTESIAN_POINT ( 'NONE',  ( 33.58253175000000113, 58.47500000273118559, -10.91162601494193751 ) ) ;
#11841 = CARTESIAN_POINT ( 'NONE',  ( -2.092463501923844636E-15, 33.50000000000001421, -34.17252228774368916 ) ) ;
#11842 = CARTESIAN_POINT ( 'NONE',  ( -32.50000000000000000, 36.00000000000000711, 0.000000000000000000 ) ) ;
#11843 = CARTESIAN_POINT ( 'NONE',  ( 1.507698388325705758E-15, 9.124999997268822938, -24.62258325217400312 ) ) ;
#11844 = CARTESIAN_POINT ( 'NONE',  ( -33.58253175000000113, 73.02500000273120406, -10.91162601494193218 ) ) ;
#11845 = DIRECTION ( 'NONE',  ( -0.000000000000000000, -1.000000000000000000, -0.000000000000000000 ) ) ;
#11846 = CARTESIAN_POINT ( 'NONE',  ( 2.688165632520823219E-15, 79.87500000273115575, 14.63369212191046209 ) ) ;
#11847 = CARTESIAN_POINT ( 'NONE',  ( 6.486482029760648627E-15, 63.87500000273119127, 35.31076352940722529 ) ) ;
#11848 = CARTESIAN_POINT ( 'NONE',  ( 2.897257156509938333E-15, 76.75000000546238255, 15.77193336357400710 ) ) ;
#11849 = DIRECTION ( 'NONE',  ( 0.000000000000000000, 0.000000000000000000, -1.000000000000000000 ) ) ;
#11850 = CARTESIAN_POINT ( 'NONE',  ( -15.14183272437242600, 3.049999994537633263, 20.84094480462497856 ) ) ;
#11851 = CARTESIAN_POINT ( 'NONE',  ( 24.18731323226247554, 15.01340250092397888, 14.01125832528285997 ) ) ;
#11852 = FACE_OUTER_BOUND ( 'NONE', #15049, .T. ) ;
#11853 = CARTESIAN_POINT ( 'NONE',  ( -20.75514604977248112, 47.42500000273118843, 28.56700777964554661 ) ) ;
#11854 = CARTESIAN_POINT ( 'NONE',  ( 6.486482029760649416E-15, 3.875000002731187720, 35.31076352940723240 ) ) ;
#11855 = CARTESIAN_POINT ( 'NONE',  ( 27.16883889988623935, 54.57500000273117280, -19.73931689729374384 ) ) ;
#11856 = CARTESIAN_POINT ( 'NONE',  ( -13.97622843553588901, 52.24739583333332860, 24.20753774853756823 ) ) ;
#11857 = CARTESIAN_POINT ( 'NONE',  ( -25.98046417659859486, 40.79465250092398065, -15.04653450569291628 ) ) ;
#11858 = VECTOR ( 'NONE', #25240, 1000.000000000000000 ) ;
#11859 = CARTESIAN_POINT ( 'NONE',  ( 28.00173670424535644, 25.45795166574268364, -7.543491769121920321 ) ) ;
#11860 = CARTESIAN_POINT ( 'NONE',  ( -26.29305231718579350, 66.30000000546236549, -19.10302069950537884 ) ) ;
#11861 = CARTESIAN_POINT ( 'NONE',  ( -13.91746824999999532, 70.97500000273119269, 4.522059556121122093 ) ) ;
#11862 = CARTESIAN_POINT ( 'NONE',  ( -0.04044903255042732459, 52.24180583240936215, -27.95245687107223986 ) ) ;
#11863 = CARTESIAN_POINT ( 'NONE',  ( -5.147494310547423346, 58.44874571845314648, 32.50000000000000000 ) ) ;
#11864 = ADVANCED_FACE ( 'NONE', ( #23983 ), #6406, .T. ) ;
#11865 = CARTESIAN_POINT ( 'NONE',  ( -24.50000000000000711, 4.849999994537633974, 7.960532557706201828 ) ) ;
#11866 = ORIENTED_EDGE ( 'NONE', *, *, #14197, .T. ) ;
#11867 = CARTESIAN_POINT ( 'NONE',  ( 27.16883889988623935, 40.57500000273118701, -19.73931689729374384 ) ) ;
#11868 =( BOUNDED_CURVE ( )  B_SPLINE_CURVE ( 2, ( #33141, #31092, #22514, #17551, #17208, #33495, #27667, #14630, #27841, #25088, #32965, #19950, #1738 ),
 .UNSPECIFIED., .F., .T. ) 
 B_SPLINE_CURVE_WITH_KNOTS ( ( 3, 2, 2, 2, 2, 2, 3 ),
 ( 0.2884615384615384914, 0.2897435897435897689, 0.2923076923076923239, 0.2948717948717948789, 0.2974358974358974339, 0.2999999999999999889, 0.3012820512820512664 ),
 .UNSPECIFIED. ) 
 CURVE ( )  GEOMETRIC_REPRESENTATION_ITEM ( )  RATIONAL_B_SPLINE_CURVE ( ( 0.9755282581475768211, 0.9755282581475772652, 1.000000000000000000, 0.9510565162951535312, 1.000000000000000000, 0.9510565162951535312, 1.000000000000000000, 0.9510565162951535312, 1.000000000000000000, 0.9510565162951535312, 1.000000000000000000, 0.9755282581475768211, 0.9755282581475768211 ) ) 
 REPRESENTATION_ITEM ( '' )  );
#11869 = CARTESIAN_POINT ( 'NONE',  ( 18.94512977948576093, 3.324999997268818230, -13.76444248337722875 ) ) ;
#11870 = CARTESIAN_POINT ( 'NONE',  ( 26.29305231718579350, 31.30000000546239036, 19.10302069950537529 ) ) ;
#11871 = EDGE_LOOP ( 'NONE', ( #26472, #2089, #32504, #29306 ) ) ;
#11872 = ADVANCED_FACE ( 'NONE', ( #10935 ), #11548, .F. ) ;
#11873 = EDGE_CURVE ( 'NONE', #12231, #16950, #16880, .T. ) ;
#11874 = CARTESIAN_POINT ( 'NONE',  ( -2.584737979205441561E-13, 36.49218750000000000, -30.02300923189239512 ) ) ;
#11875 = VERTEX_POINT ( 'NONE', #10429 ) ;
#11876 = CARTESIAN_POINT ( 'NONE',  ( -19.82091636218621389, 12.94999999453763628, 14.40073868116558842 ) ) ;
#11877 = CARTESIAN_POINT ( 'NONE',  ( -20.75514604977248823, 48.82500000273117280, -28.56700777964554305 ) ) ;
#11878 = CARTESIAN_POINT ( 'NONE',  ( 26.00068869287340334, 61.12760416666665719, -15.01150461594642316 ) ) ;
#11879 = CARTESIAN_POINT ( 'NONE',  ( -26.29305231718579350, 14.30000000546238681, -19.10302069950537884 ) ) ;
#11880 = EDGE_CURVE ( 'NONE', #31338, #7013, #21908, .T. ) ;
#11881 = CARTESIAN_POINT ( 'NONE',  ( -32.50000000000000000, 8.100000000000006750, 10.55989012756946366 ) ) ;
#11882 = CONICAL_SURFACE ( 'NONE', #26672, 15.31642273298461276, 0.2613323016132377830 ) ;
#11883 = CARTESIAN_POINT ( 'NONE',  ( 7.236395654485760609, 13.52499999726880553, -22.27133577429736633 ) ) ;
#11884 = CARTESIAN_POINT ( 'NONE',  ( -26.29305231718578995, 56.20000000000000284, 19.10302069950538595 ) ) ;
#11885 = DIRECTION ( 'NONE',  ( -0.000000000000000000, 1.000000000000000000, -0.000000000000000000 ) ) ;
#11886 = CARTESIAN_POINT ( 'NONE',  ( 27.16883889988623935, 14.57500000273120833, -19.73931689729374384 ) ) ;
#11887 = CARTESIAN_POINT ( 'NONE',  ( -6.950374756619247307, 19.72878499907601935, 26.09010956794245217 ) ) ;
#11888 = CARTESIAN_POINT ( 'NONE',  ( -11.25946833292375793, 72.67500000273119554, -8.180482586598733619 ) ) ;
#11889 = FACE_OUTER_BOUND ( 'NONE', #33394, .T. ) ;
#11890 = CARTESIAN_POINT ( 'NONE',  ( 5.147494310547434893, 14.55125428154684997, 32.49999999999999289 ) ) ;
#11891 = VECTOR ( 'NONE', #6387, 1000.000000000000000 ) ;
#11892 = CARTESIAN_POINT ( 'NONE',  ( 6.277390505771533514E-15, 2.500000000000008882, 34.17252228774368916 ) ) ;
#11893 = VERTEX_POINT ( 'NONE', #282 ) ;
#11894 = CARTESIAN_POINT ( 'NONE',  ( -18.94512977948575738, 9.924999997268812990, -13.76444248337723231 ) ) ;
#11895 = FACE_OUTER_BOUND ( 'NONE', #32462, .T. ) ;
#11896 = CARTESIAN_POINT ( 'NONE',  ( 19.09188309203661049, 36.92187499999999289, -19.09188309203694445 ) ) ;
#11897 = CARTESIAN_POINT ( 'NONE',  ( -33.58253175000000113, 65.02500000273118985, -10.91162601494193218 ) ) ;
#11898 = CARTESIAN_POINT ( 'NONE',  ( 33.58253175000000113, 26.37500000273117351, -4.112674001490185761E-15 ) ) ;
#11899 = CARTESIAN_POINT ( 'NONE',  ( 27.16883889988623935, 16.57500000273119767, -19.73931689729374384 ) ) ;
#11900 = CARTESIAN_POINT ( 'NONE',  ( 27.16883889988624290, 10.17500000273119376, 19.73931689729373673 ) ) ;
#11901 = CARTESIAN_POINT ( 'NONE',  ( -14.97647472619946285, 13.58111083425730925, -26.02091320914851025 ) ) ;
#11902 = CARTESIAN_POINT ( 'NONE',  ( 30.02300923189239512, 57.97656249999997868, -2.619432448724977703E-13 ) ) ;
#11903 = CARTESIAN_POINT ( 'NONE',  ( 11.25946833292375793, 76.17500000273119554, 8.180482586598731842 ) ) ;
#11904 = CARTESIAN_POINT ( 'NONE',  ( 32.50000000000000000, 45.10000000000000853, -10.55989012756945833 ) ) ;
#11905 = CARTESIAN_POINT ( 'NONE',  ( -3.880418787951136039, 2.301254276084479411, -24.50000000000000000 ) ) ;
#11906 = CARTESIAN_POINT ( 'NONE',  ( 20.75514604977248467, 50.42500000273118843, -28.56700777964554305 ) ) ;
#11907 = CARTESIAN_POINT ( 'NONE',  ( -18.94512977948575738, 5.424999997268809437, -13.76444248337723231 ) ) ;
#11908 = EDGE_LOOP ( 'NONE', ( #3628, #17938, #17206, #33834 ) ) ;
#11909 = CARTESIAN_POINT ( 'NONE',  ( -10.37757302488623701, 59.77500000273121117, 31.93888565452638417 ) ) ;
#11910 = DIRECTION ( 'NONE',  ( -1.224646799147353454E-16, 1.000000000000000000, -0.000000000000000000 ) ) ;
#11911 = CARTESIAN_POINT ( 'NONE',  ( 7.236395654485760609, 11.02499999726880375, -22.27133577429736633 ) ) ;
#11912 = CARTESIAN_POINT ( 'NONE',  ( 19.06425588902592239, 28.90663166759063785, 19.11951029504763611 ) ) ;
#11913 = ORIENTED_EDGE ( 'NONE', *, *, #8508, .F. ) ;
#11914 = AXIS2_PLACEMENT_3D ( 'NONE', #26073, #13375, #18533 ) ;
#11915 = CARTESIAN_POINT ( 'NONE',  ( 10.37757302488624767, 27.72500000273118914, 31.93888565452638417 ) ) ;
#11916 = CARTESIAN_POINT ( 'NONE',  ( 5.779280353836490358E-15, 76.49999999999998579, 32.49999999999999289 ) ) ;
#11917 = EDGE_LOOP ( 'NONE', ( #7278, #31584 ) ) ;
#11918 = CARTESIAN_POINT ( 'NONE',  ( 28.01184896238304134, 61.55729166666666430, 7.505752307972846538 ) ) ;
#11919 = CARTESIAN_POINT ( 'NONE',  ( -33.58253175000000113, 59.27500000273119696, -10.91162601494193218 ) ) ;
#11920 = CARTESIAN_POINT ( 'NONE',  ( -1.778240108872766143E-15, 29.50000000000000711, -32.49999999999999289 ) ) ;
#11921 = CARTESIAN_POINT ( 'NONE',  ( -20.75514604977248112, 67.42500000273118133, 28.56700777964554661 ) ) ;
#11922 = CARTESIAN_POINT ( 'NONE',  ( 26.00068869287367335, 27.32552083333332860, 15.01150461594596308 ) ) ;
#11923 = ADVANCED_BREP_SHAPE_REPRESENTATION ( '', ( #32241, #1376 ), #16210 ) ;
#11924 = CARTESIAN_POINT ( 'NONE',  ( -15.14183272437241889, 10.70000000000001172, -20.84094480462497856 ) ) ;
#11925 = CARTESIAN_POINT ( 'NONE',  ( 6.486482029760649416E-15, 5.875000002731167292, 35.31076352940723240 ) ) ;
#11926 = EDGE_CURVE ( 'NONE', #29752, #6637, #33318, .T. ) ;
#11927 = CARTESIAN_POINT ( 'NONE',  ( 20.75514604977249178, 7.825000002731194115, 28.56700777964553950 ) ) ;
#11928 = CARTESIAN_POINT ( 'NONE',  ( -8.601468415847515203, 71.17500000273116711, 11.83890561707634959 ) ) ;
#11929 = CARTESIAN_POINT ( 'NONE',  ( -14.97647472619899389, 47.37201416574269786, 26.02091320914878025 ) ) ;
#11930 = CARTESIAN_POINT ( 'NONE',  ( 15.00000000000000000, 81.00000000000001421, -1.836970198721029589E-15 ) ) ;
#11931 = CARTESIAN_POINT ( 'NONE',  ( 26.00068869287367690, 54.82552083333332149, 15.01150461594596486 ) ) ;
#11932 = CARTESIAN_POINT ( 'NONE',  ( 10.04305231718579705, 61.10000000546239818, 30.90933677959248982 ) ) ;
#11933 = CARTESIAN_POINT ( 'NONE',  ( 24.50000000000000000, 5.749999994537624559, 0.000000000000000000 ) ) ;
#11934 = CARTESIAN_POINT ( 'NONE',  ( -12.13525491562420910, 78.45000000546237118, 8.816778784387098611 ) ) ;
#11935 = CARTESIAN_POINT ( 'NONE',  ( 24.20753774853756113, 13.57552083333332682, 13.97622843553589789 ) ) ;
#11936 = CARTESIAN_POINT ( 'NONE',  ( -20.75514604977248823, 36.82500000273117990, -28.56700777964554305 ) ) ;
#11937 = CARTESIAN_POINT ( 'NONE',  ( 8.601468415847520532, 73.57500000273117280, 11.83890561707634781 ) ) ;
#11938 = CARTESIAN_POINT ( 'NONE',  ( 33.58253175000000113, 44.47500000273119269, -10.91162601494193751 ) ) ;
#11939 = CARTESIAN_POINT ( 'NONE',  ( 20.75514604977248467, 26.67500000273118133, -28.56700777964554305 ) ) ;
#11940 = CARTESIAN_POINT ( 'NONE',  ( 10.04305231718579705, 40.59999999999999432, 30.90933677959248982 ) ) ;
#11941 = CARTESIAN_POINT ( 'NONE',  ( -33.58253175000000113, 79.37500000273118417, 0.000000000000000000 ) ) ;
#11942 = CARTESIAN_POINT ( 'NONE',  ( 2.375766604868044141, 81.44874571845316780, -14.99999999999999822 ) ) ;
#11943 = CARTESIAN_POINT ( 'NONE',  ( 26.29305231718578995, 69.20000000000000284, -19.10302069950538240 ) ) ;
#11944 = CARTESIAN_POINT ( 'NONE',  ( 23.41746824999999887, 8.724999997268806595, -7.608796670333727974 ) ) ;
#11945 = CARTESIAN_POINT ( 'NONE',  ( 26.02091320914876960, 22.45013916574269075, 14.97647472619900455 ) ) ;
#11946 = CARTESIAN_POINT ( 'NONE',  ( -4.523095164977116484E-15, 4.624999997268820273, 24.62258325217400312 ) ) ;
#11947 = CARTESIAN_POINT ( 'NONE',  ( 24.18731323226221974, 39.06472249907601935, -14.01125832528328985 ) ) ;
#11948 = CARTESIAN_POINT ( 'NONE',  ( 20.75514604977249178, 13.82500000273117813, 28.56700777964553950 ) ) ;
#11949 = CARTESIAN_POINT ( 'NONE',  ( -4.523095164977116484E-15, 14.62499999726882649, 24.62258325217400312 ) ) ;
#11950 = CARTESIAN_POINT ( 'NONE',  ( 26.07999730980477437, 64.70833333333334281, -6.988114217768290004 ) ) ;
#11951 = ORIENTED_EDGE ( 'NONE', *, *, #8784, .F. ) ;
#11952 = CARTESIAN_POINT ( 'NONE',  ( -33.58253175000000113, 51.22500000273119269, 10.91162601494193929 ) ) ;
#11953 = CARTESIAN_POINT ( 'NONE',  ( 27.16883889988624290, 24.17500000273119198, 19.73931689729373673 ) ) ;
#11954 = ORIENTED_EDGE ( 'NONE', *, *, #618, .T. ) ;
#11955 = CARTESIAN_POINT ( 'NONE',  ( -28.01184896238304134, 28.90104166666666785, -7.505752307972844761 ) ) ;
#11956 = CARTESIAN_POINT ( 'NONE',  ( 7.543491769121427382, 34.63579833425730925, -28.00173670424548433 ) ) ;
#11957 = CARTESIAN_POINT ( 'NONE',  ( -24.50000000000000000, 2.899999999999995470, -7.960532557706207157 ) ) ;
#11958 = CARTESIAN_POINT ( 'NONE',  ( -15.14183272437242600, 15.04999999453763238, 20.84094480462497856 ) ) ;
#11959 = CARTESIAN_POINT ( 'NONE',  ( 14.47279130897151767, 6.924999997268805885, -19.92008829642072598 ) ) ;
#11960 = CARTESIAN_POINT ( 'NONE',  ( -27.16883889988623935, 21.57500000273118701, 19.73931689729374739 ) ) ;
#11961 = CARTESIAN_POINT ( 'NONE',  ( -32.50000000000000000, 22.60000000546236976, 10.55989012756946366 ) ) ;
#11962 = CARTESIAN_POINT ( 'NONE',  ( 20.08610463437158344, 70.70000000000000284, 27.64615127144129403 ) ) ;
#11963 = LINE ( 'NONE', #4073, #7206 ) ;
#11964 = CARTESIAN_POINT ( 'NONE',  ( 2.532662468604912398, 74.00000000000004263, 13.81508367526550884 ) ) ;
#11965 = CARTESIAN_POINT ( 'NONE',  ( 28.02196122052045268, 55.83371500092398065, -7.468012846824774620 ) ) ;
#11966 = CARTESIAN_POINT ( 'NONE',  ( 33.58253175000000823, 34.27500000273116854, 10.91162601494192863 ) ) ;
#11967 = CARTESIAN_POINT ( 'NONE',  ( 27.16883889988624290, 53.92500000273118843, 19.73931689729373673 ) ) ;
#11968 = CARTESIAN_POINT ( 'NONE',  ( 15.01150461594596486, 26.46614583333332504, -26.00068869287367690 ) ) ;
#11969 =( BOUNDED_CURVE ( )  B_SPLINE_CURVE ( 2, ( #18776, #392, #11046, #8624, #21513, #28887, #29545, #26322, #29051, #31961, #16368, #26822, #26658 ),
 .UNSPECIFIED., .F., .T. ) 
 B_SPLINE_CURVE_WITH_KNOTS ( ( 3, 2, 2, 2, 2, 2, 3 ),
 ( 0.3653846153846153633, 0.3666666666666666408, 0.3692307692307692513, 0.3717948717948718063, 0.3743589743589743613, 0.3769230769230769162, 0.3782051282051281937 ),
 .UNSPECIFIED. ) 
 CURVE ( )  GEOMETRIC_REPRESENTATION_ITEM ( )  RATIONAL_B_SPLINE_CURVE ( ( 0.9755282581475768211, 0.9755282581475768211, 1.000000000000000000, 0.9510565162951535312, 1.000000000000000000, 0.9510565162951535312, 1.000000000000000000, 0.9510565162951535312, 1.000000000000000000, 0.9510565162951535312, 1.000000000000000000, 0.9755282581475768211, 0.9755282581475768211 ) ) 
 REPRESENTATION_ITEM ( '' )  );
#11970 = EDGE_CURVE ( 'NONE', #22014, #12120, #28720, .T. ) ;
#11971 = CARTESIAN_POINT ( 'NONE',  ( 23.41746825000000243, 9.224999997268820806, -7.608796670333727974 ) ) ;
#11972 = CARTESIAN_POINT ( 'NONE',  ( 10.04305231718579705, 16.60000000000000497, 30.90933677959248982 ) ) ;
#11973 = CARTESIAN_POINT ( 'NONE',  ( 2.445080149700053643E-15, 76.50000000000001421, 15.00000000000000000 ) ) ;
#11974 = CARTESIAN_POINT ( 'NONE',  ( 24.22776226481265383, 43.07513916574269786, 13.94119854578893580 ) ) ;
#11975 =( BOUNDED_CURVE ( )  B_SPLINE_CURVE ( 2, ( #2277, #30410, #17912, #30757, #28020, #7247, #25276, #19963, #14982, #20306, #6910, #15159, #10010 ),
 .UNSPECIFIED., .F., .T. ) 
 B_SPLINE_CURVE_WITH_KNOTS ( ( 3, 2, 2, 2, 2, 2, 3 ),
 ( 0.4551282051282051211, 0.4564102564102563986, 0.4589743589743589536, 0.4615384615384615641, 0.4641025641025641191, 0.4666666666666666741, 0.4679487179487179516 ),
 .UNSPECIFIED. ) 
 CURVE ( )  GEOMETRIC_REPRESENTATION_ITEM ( )  RATIONAL_B_SPLINE_CURVE ( ( 0.9755282581475768211, 0.9755282581475768211, 1.000000000000000000, 0.9510565162951535312, 1.000000000000000000, 0.9510565162951535312, 1.000000000000000000, 0.9510565162951535312, 1.000000000000000000, 0.9510565162951535312, 1.000000000000000000, 0.9755282581475768211, 0.9755282581475768211 ) ) 
 REPRESENTATION_ITEM ( '' )  );
#11976 = CARTESIAN_POINT ( 'NONE',  ( -2.162160676586881955E-15, 58.62500000273118417, -35.31076352940723240 ) ) ;
#11977 = CARTESIAN_POINT ( 'NONE',  ( -2.162160676586882350E-15, 46.87500000273118417, -35.31076352940722529 ) ) ;
#11978 = DIRECTION ( 'NONE',  ( -1.224646799147353454E-16, 1.000000000000000000, -0.000000000000000000 ) ) ;
#11979 = DIRECTION ( 'NONE',  ( 0.000000000000000000, 1.000000000000000000, 0.000000000000000000 ) ) ;
#11980 = CARTESIAN_POINT ( 'NONE',  ( -26.29305231718578995, 50.19999999999999574, 19.10302069950538595 ) ) ;
#11981 = CARTESIAN_POINT ( 'NONE',  ( 13.94119854578937812, 46.23736083425730925, 24.22776226481240514 ) ) ;
#11982 = CARTESIAN_POINT ( 'NONE',  ( 19.82091636218621389, 4.200000000000009059, -14.40073868116559197 ) ) ;
#11983 = CARTESIAN_POINT ( 'NONE',  ( 20.75514604977248467, 24.42500000273119554, -28.56700777964554305 ) ) ;
#11984 = CARTESIAN_POINT ( 'NONE',  ( -9.270509831248423538, 77.95000000546239960, -12.75976212528059861 ) ) ;
#11985 = CARTESIAN_POINT ( 'NONE',  ( 26.29305231718579350, 41.30000000546238681, 19.10302069950537529 ) ) ;
#11986 = CARTESIAN_POINT ( 'NONE',  ( 30.02300923189239867, 63.41368083240934794, -0.04044903255044467877 ) ) ;
#11987 = CARTESIAN_POINT ( 'NONE',  ( 32.50000000000000000, 39.50000000546237544, -3.980102097228898626E-15 ) ) ;
#11988 = CARTESIAN_POINT ( 'NONE',  ( -26.29305231718579350, 60.30000000546237260, -19.10302069950537884 ) ) ;
#11989 = CARTESIAN_POINT ( 'NONE',  ( 6.486482029760648627E-15, 35.62500000273118417, 35.31076352940722529 ) ) ;
#11990 = CARTESIAN_POINT ( 'NONE',  ( -27.16883889988623935, 65.57500000273120122, 19.73931689729374739 ) ) ;
#11991 = CARTESIAN_POINT ( 'NONE',  ( 19.09188309203694800, 34.34374999999999289, 19.09188309203660694 ) ) ;
#11992 = VERTEX_POINT ( 'NONE', #7246 ) ;
#11993 = CARTESIAN_POINT ( 'NONE',  ( 20.75514604977249178, 65.82500000273115859, 28.56700777964553950 ) ) ;
#11994 = CARTESIAN_POINT ( 'NONE',  ( 2.740863092043355209E-13, 38.21093750000000000, 30.02300923189239512 ) ) ;
#11995 = LINE ( 'NONE', #1178, #15741 ) ;
#11996 = ORIENTED_EDGE ( 'NONE', *, *, #6694, .F. ) ;
#11997 = CARTESIAN_POINT ( 'NONE',  ( 28.02196122052045268, 52.39621500092398065, -7.468012846824774620 ) ) ;
#11998 = CARTESIAN_POINT ( 'NONE',  ( -26.09010956794232428, 50.67746500092398065, 6.950374756619732253 ) ) ;
#11999 = CARTESIAN_POINT ( 'NONE',  ( -32.50000000000000000, 8.600000005462376862, 10.55989012756946366 ) ) ;
#12000 = CARTESIAN_POINT ( 'NONE',  ( 2.740863092043355209E-13, 65.71093749999997158, 30.02300923189239512 ) ) ;
#12001 = CARTESIAN_POINT ( 'NONE',  ( -10.04305231718578462, 64.90000000546235981, 30.90933677959249337 ) ) ;
#12002 = CARTESIAN_POINT ( 'NONE',  ( -10.37757302488624411, 38.97500000273118559, -31.93888565452638417 ) ) ;
#12003 = CARTESIAN_POINT ( 'NONE',  ( 10.04305231718578817, 43.90000000546237402, -30.90933677959249337 ) ) ;
#12004 = CARTESIAN_POINT ( 'NONE',  ( 8.601468415847516980, 74.67500000273120975, -11.83890561707634781 ) ) ;
#12005 = CARTESIAN_POINT ( 'NONE',  ( -10.37757302488624411, 26.72500000273120335, -31.93888565452638417 ) ) ;
#12006 = CARTESIAN_POINT ( 'NONE',  ( -10.04305231718579172, 23.60000000000000853, -30.90933677959248982 ) ) ;
#12007 = CARTESIAN_POINT ( 'NONE',  ( 20.75514604977249178, 58.07500000273117990, 28.56700777964553950 ) ) ;
#12008 = EDGE_CURVE ( 'NONE', #6801, #29733, #14470, .T. ) ;
#12009 = CARTESIAN_POINT ( 'NONE',  ( -26.29305231718578995, 38.19999999999999574, 19.10302069950538595 ) ) ;
#12010 = ADVANCED_FACE ( 'NONE', ( #12055 ), #19962, .F. ) ;
#12011 = CARTESIAN_POINT ( 'NONE',  ( -32.50000000000000000, 32.10000000000000142, 10.55989012756946366 ) ) ;
#12012 = CARTESIAN_POINT ( 'NONE',  ( -23.41746825000000243, 15.52499999726882507, -7.608796670333730638 ) ) ;
#12013 = CARTESIAN_POINT ( 'NONE',  ( -10.37757302488624411, 76.72500000273119269, -31.93888565452638417 ) ) ;
#12014 = CARTESIAN_POINT ( 'NONE',  ( -32.50000000000000000, 70.40000000546237402, -10.55989012756945300 ) ) ;
#12015 = CARTESIAN_POINT ( 'NONE',  ( 13.91746824999999887, 76.37500000273116996, -1.704398294459741270E-15 ) ) ;
#12016 = CARTESIAN_POINT ( 'NONE',  ( -10.37757302488623701, 67.77500000273117564, 31.93888565452638417 ) ) ;
#12017 = CARTESIAN_POINT ( 'NONE',  ( 15.00000000000000000, 77.35000000546234844, -4.873795443493596835 ) ) ;
#12018 = FACE_OUTER_BOUND ( 'NONE', #4469, .T. ) ;
#12019 = CARTESIAN_POINT ( 'NONE',  ( -24.50000000000001066, 4.849999994537633974, 7.960532557706201828 ) ) ;
#12020 = CARTESIAN_POINT ( 'NONE',  ( -0.04044903254992426173, 22.46131916759064850, 27.95245687107223276 ) ) ;
#12021 = CARTESIAN_POINT ( 'NONE',  ( 20.08610463437158344, 46.70000000000000284, 27.64615127144129403 ) ) ;
#12022 = CARTESIAN_POINT ( 'NONE',  ( -33.58253175000000113, 43.02500000273118275, -10.91162601494193218 ) ) ;
#12023 = CARTESIAN_POINT ( 'NONE',  ( 33.58253175000000823, 4.275000002731189852, 10.91162601494192863 ) ) ;
#12024 = CARTESIAN_POINT ( 'NONE',  ( -33.58253175000000113, 55.27500000273121117, -10.91162601494193041 ) ) ;
#12025 = CARTESIAN_POINT ( 'NONE',  ( 24.20753774853756113, 54.82552083333332149, 13.97622843553589789 ) ) ;
#12026 = CARTESIAN_POINT ( 'NONE',  ( 20.53372385742072481, 45.23475666759063785, -20.47846945139902175 ) ) ;
#12027 = CARTESIAN_POINT ( 'NONE',  ( 20.53372385742108008, 36.34336833240934794, 20.47846945139866648 ) ) ;
#12028 = CARTESIAN_POINT ( 'NONE',  ( -2.092463501923844636E-15, 58.00000000546235412, -34.17252228774368916 ) ) ;
#12029 = EDGE_CURVE ( 'NONE', #30412, #17976, #22525, .T. ) ;
#12030 = CARTESIAN_POINT ( 'NONE',  ( 13.91746824999999887, 80.37500000273118417, -1.704398294459741270E-15 ) ) ;
#12031 = CARTESIAN_POINT ( 'NONE',  ( -26.09010956794245217, 68.71315999907601224, -6.950374756619243755 ) ) ;
#12032 = CARTESIAN_POINT ( 'NONE',  ( 4.635254915624212657, 78.60000000000000853, 14.26584774442730286 ) ) ;
#12033 = CARTESIAN_POINT ( 'NONE',  ( 20.75514604977248467, 40.67500000273116711, -28.56700777964554305 ) ) ;
#12034 = CARTESIAN_POINT ( 'NONE',  ( -18.94512977948575738, 1.924999997268805885, -13.76444248337723231 ) ) ;
#12035 = VERTEX_POINT ( 'NONE', #12228 ) ;
#12036 = CARTESIAN_POINT ( 'NONE',  ( -2.092463501923844636E-15, 30.00000000546236478, -34.17252228774368916 ) ) ;
#12037 = VERTEX_POINT ( 'NONE', #27508 ) ;
#12038 = CARTESIAN_POINT ( 'NONE',  ( -28.01184896238290278, 35.48958333333332860, 7.505752307973363457 ) ) ;
#12039 = CARTESIAN_POINT ( 'NONE',  ( -20.08610463437157989, 60.20000000546237828, -27.64615127144129758 ) ) ;
#12040 = ORIENTED_EDGE ( 'NONE', *, *, #11053, .F. ) ;
#12041 = CARTESIAN_POINT ( 'NONE',  ( -20.08610463437156923, 56.29999999999999716, 27.64615127144130113 ) ) ;
#12042 = CARTESIAN_POINT ( 'NONE',  ( 27.16883889988623935, 48.32500000273117990, -19.73931689729374384 ) ) ;
#12043 = CARTESIAN_POINT ( 'NONE',  ( 7.236395654485760609, 17.02499999726880731, -22.27133577429736633 ) ) ;
#12044 = FACE_OUTER_BOUND ( 'NONE', #1266, .T. ) ;
#12045 = APPLICATION_CONTEXT ( 'automotive_design' ) ;
#12046 = CARTESIAN_POINT ( 'NONE',  ( -32.50000000000000000, 10.50000000546236123, 0.000000000000000000 ) ) ;
#12047 = CARTESIAN_POINT ( 'NONE',  ( -33.58253175000000113, 65.22500000273117848, 10.91162601494193929 ) ) ;
#12048 = CARTESIAN_POINT ( 'NONE',  ( -23.41746824999999887, 14.12499999726882294, -2.867812753649727150E-15 ) ) ;
#12049 = CARTESIAN_POINT ( 'NONE',  ( 10.04305231718578817, 53.40000000000000568, -30.90933677959249337 ) ) ;
#12050 = DIRECTION ( 'NONE',  ( -1.224646799147353454E-16, 1.000000000000000000, -0.000000000000000000 ) ) ;
#12051 = CARTESIAN_POINT ( 'NONE',  ( -10.37757302488624411, 18.97500000273119625, -31.93888565452638417 ) ) ;
#12052 = CARTESIAN_POINT ( 'NONE',  ( 12.13525491562421088, 76.80000000000001137, 8.816778784387095058 ) ) ;
#12053 = CARTESIAN_POINT ( 'NONE',  ( -0.04044903255042732459, 24.74180583240935505, -27.95245687107223986 ) ) ;
#12054 = CARTESIAN_POINT ( 'NONE',  ( 13.91746825000000065, 77.77500000273117564, 4.522059556121114987 ) ) ;
#12055 = FACE_OUTER_BOUND ( 'NONE', #6066, .T. ) ;
#12056 = CARTESIAN_POINT ( 'NONE',  ( -32.50000000000000000, 21.99999999999999289, 0.000000000000000000 ) ) ;
#12057 = CARTESIAN_POINT ( 'NONE',  ( 20.08610463437158344, 4.699999999999995737, 27.64615127144129403 ) ) ;
#12058 = VERTEX_POINT ( 'NONE', #24927 ) ;
#12059 = CARTESIAN_POINT ( 'NONE',  ( 7.236395654485755280, 8.724999997268806595, 22.27133577429736988 ) ) ;
#12060 = LINE ( 'NONE', #27859, #24943 ) ;
#12061 = CARTESIAN_POINT ( 'NONE',  ( 6.988114217767829928, 50.38541666666666430, -26.07999730980489872 ) ) ;
#12062 = CARTESIAN_POINT ( 'NONE',  ( 20.75514604977248467, 62.42500000273118133, -28.56700777964554305 ) ) ;
#12063 = CARTESIAN_POINT ( 'NONE',  ( -10.37757302488624411, 24.97500000273118914, -31.93888565452638417 ) ) ;
#12064 = CARTESIAN_POINT ( 'NONE',  ( -33.58253175000000113, 11.27500000273118630, -10.91162601494193218 ) ) ;
#12065 = CARTESIAN_POINT ( 'NONE',  ( -10.37757302488624411, 2.975000002731182036, -31.93888565452638417 ) ) ;
#12066 = CARTESIAN_POINT ( 'NONE',  ( 14.97647472619947351, 15.29986083425731280, 26.02091320914850314 ) ) ;
#12067 = EDGE_CURVE ( 'NONE', #679, #4618, #17292, .T. ) ;
#12068 = CARTESIAN_POINT ( 'NONE',  ( 20.50609665441005092, 61.84374999999998579, 20.50609665440969209 ) ) ;
#12069 =( BOUNDED_CURVE ( )  B_SPLINE_CURVE ( 2, ( #27054, #26728, #21755, #9026, #24482, #3716, #29614 ),
 .UNSPECIFIED., .F., .F. ) 
 B_SPLINE_CURVE_WITH_KNOTS ( ( 3, 2, 2, 3 ),
 ( 0.9722222222222222099, 0.9777777777777777457, 0.9888888888888889284, 1.000000000000000000 ),
 .UNSPECIFIED. ) 
 CURVE ( )  GEOMETRIC_REPRESENTATION_ITEM ( )  RATIONAL_B_SPLINE_CURVE ( ( 0.9755282581475768211, 0.9755282581475768211, 1.000000000000000000, 0.9510565162951535312, 1.000000000000000000, 0.9510565162951535312, 1.000000000000000000 ) ) 
 REPRESENTATION_ITEM ( '' )  );
#12070 = CARTESIAN_POINT ( 'NONE',  ( 32.50000000000000000, 45.00000000000000000, -3.980102097228898626E-15 ) ) ;
#12071 = CARTESIAN_POINT ( 'NONE',  ( 10.37757302488624056, 52.52500000273118985, -31.93888565452638417 ) ) ;
#12072 = CARTESIAN_POINT ( 'NONE',  ( -18.94512977948575738, 1.424999997268805441, -13.76444248337723231 ) ) ;
#12073 = EDGE_CURVE ( 'NONE', #31792, #23152, #32217, .T. ) ;
#12074 = CARTESIAN_POINT ( 'NONE',  ( 10.04305231718578817, 21.90000000546238468, -30.90933677959249337 ) ) ;
#12075 = ORIENTED_EDGE ( 'NONE', *, *, #28655, .F. ) ;
#12076 = CARTESIAN_POINT ( 'NONE',  ( -33.58253175000000113, 59.37500000273119838, 0.000000000000000000 ) ) ;
#12077 = CARTESIAN_POINT ( 'NONE',  ( 10.04305231718578817, 17.39999999999999858, -30.90933677959249337 ) ) ;
#12078 = CARTESIAN_POINT ( 'NONE',  ( 14.47279130897151767, 14.92499999726881299, -19.92008829642072598 ) ) ;
#12079 = CARTESIAN_POINT ( 'NONE',  ( -7.025853678916393008, 29.47954833425730570, 26.06988505166735592 ) ) ;
#12080 = ORIENTED_EDGE ( 'NONE', *, *, #26284, .F. ) ;
#12081 = CARTESIAN_POINT ( 'NONE',  ( -20.75514604977248112, 27.42500000273118488, 28.56700777964554661 ) ) ;
#12082 = CARTESIAN_POINT ( 'NONE',  ( 3.880418787951153803, 5.551254281546845526, 24.49999999999999645 ) ) ;
#12083 = ORIENTED_EDGE ( 'NONE', *, *, #4225, .F. ) ;
#12084 = CARTESIAN_POINT ( 'NONE',  ( -28.01184896238304134, 63.27604166666667140, -7.505752307972844761 ) ) ;
#12085 = CARTESIAN_POINT ( 'NONE',  ( -33.58253175000000113, 61.47500000273117848, 10.91162601494193929 ) ) ;
#12086 = CARTESIAN_POINT ( 'NONE',  ( -9.270509831248419985, 76.30000000000003979, 12.75976212528060039 ) ) ;
#12087 = CARTESIAN_POINT ( 'NONE',  ( 27.16883889988624290, 67.92500000273119554, 19.73931689729373673 ) ) ;
#12088 = CARTESIAN_POINT ( 'NONE',  ( 2.740863092043355209E-13, 38.21093750000000000, 30.02300923189239512 ) ) ;
#12089 = CARTESIAN_POINT ( 'NONE',  ( -4.732186688966233175E-15, 15.50000000000000533, 25.76082449383753925 ) ) ;
#12090 = CARTESIAN_POINT ( 'NONE',  ( -33.58253175000000113, 5.375000002731167292, 0.000000000000000000 ) ) ;
#12091 = CARTESIAN_POINT ( 'NONE',  ( -20.75514604977248823, 8.825000002731190563, -28.56700777964554305 ) ) ;
#12092 = CARTESIAN_POINT ( 'NONE',  ( -26.29305231718578995, 0.7000000054623867207, 19.10302069950538595 ) ) ;
#12093 = CARTESIAN_POINT ( 'NONE',  ( 25.98046417659831775, 49.37722249907602645, -15.04653450569338879 ) ) ;
#12094 = CARTESIAN_POINT ( 'NONE',  ( -4.635254915624208216, 76.40000000000001990, 14.26584774442730463 ) ) ;
#12095 = CARTESIAN_POINT ( 'NONE',  ( 26.00068869287341045, 57.69010416666666430, -15.01150461594642493 ) ) ;
#12096 = CARTESIAN_POINT ( 'NONE',  ( -7.570916362186215665, 15.14999999453761603, 23.30088464923126423 ) ) ;
#12097 = CARTESIAN_POINT ( 'NONE',  ( 5.147494310547426899, 61.94874572391551482, -32.50000000000000000 ) ) ;
#12098 = CARTESIAN_POINT ( 'NONE',  ( -15.14183272437242600, 9.049999994537618164, 20.84094480462497856 ) ) ;
#12099 = CARTESIAN_POINT ( 'NONE',  ( 26.49999999999999645, -1.999999999999995337, 3.245314017740485765E-15 ) ) ;
#12100 = CARTESIAN_POINT ( 'NONE',  ( -19.09188309203660694, 18.01562499999999645, 19.09188309203694800 ) ) ;
#12101 = CARTESIAN_POINT ( 'NONE',  ( -10.37757302488624411, 38.72500000273118559, -31.93888565452638417 ) ) ;
#12102 = CARTESIAN_POINT ( 'NONE',  ( 8.601468415847520532, 75.57500000273117280, 11.83890561707634781 ) ) ;
#12103 = CARTESIAN_POINT ( 'NONE',  ( -20.75514604977248823, 43.07500000273118701, -28.56700777964554305 ) ) ;
#12104 = CARTESIAN_POINT ( 'NONE',  ( -33.58253175000000113, 31.27500000273117919, -10.91162601494193041 ) ) ;
#12105 = CARTESIAN_POINT ( 'NONE',  ( 26.29305231718578995, 41.20000000000001705, -19.10302069950538240 ) ) ;
#12106 = CARTESIAN_POINT ( 'NONE',  ( -26.29305231718579350, 8.300000005462383257, -19.10302069950537884 ) ) ;
#12107 = CARTESIAN_POINT ( 'NONE',  ( 26.29305231718579350, 32.79999999999999716, 19.10302069950537529 ) ) ;
#12108 = CARTESIAN_POINT ( 'NONE',  ( -20.08610463437156923, 68.30000000000001137, 27.64615127144130113 ) ) ;
#12109 = CARTESIAN_POINT ( 'NONE',  ( -4.523095164977117273E-15, 10.12499999726882116, 24.62258325217400312 ) ) ;
#12110 = CARTESIAN_POINT ( 'NONE',  ( 15.04653450569339945, 26.17409749907601935, 25.98046417659831775 ) ) ;
#12111 = CARTESIAN_POINT ( 'NONE',  ( 23.41746825000000243, 1.224999997268811480, -7.608796670333727974 ) ) ;
#12112 = CARTESIAN_POINT ( 'NONE',  ( -19.11951029504797006, 34.62461833240934794, -19.06425588902558133 ) ) ;
#12113 = SURFACE_STYLE_FILL_AREA ( #20022 ) ;
#12114 = CARTESIAN_POINT ( 'NONE',  ( 27.16883889988624290, 11.92500000273116711, 19.73931689729373673 ) ) ;
#12115 = CARTESIAN_POINT ( 'NONE',  ( 23.41746825000000243, 15.02499999726881086, 7.608796670333735079 ) ) ;
#12116 = CARTESIAN_POINT ( 'NONE',  ( -6.988114217767819270, 62.41666666666666430, 26.07999730980490583 ) ) ;
#12117 = ORIENTED_EDGE ( 'NONE', *, *, #11270, .F. ) ;
#12118 = CARTESIAN_POINT ( 'NONE',  ( 10.37757302488624056, 52.52500000273117564, -31.93888565452638417 ) ) ;
#12119 = CARTESIAN_POINT ( 'NONE',  ( 20.75514604977249178, 20.07500000273118346, 28.56700777964553950 ) ) ;
#12120 = VERTEX_POINT ( 'NONE', #27679 ) ;
#12121 = CARTESIAN_POINT ( 'NONE',  ( -28.01184896238290278, 32.05208333333332860, 7.505752307973363457 ) ) ;
#12122 = CARTESIAN_POINT ( 'NONE',  ( 26.02091320914851025, 35.06548583425731636, -14.97647472619946463 ) ) ;
#12123 = CIRCLE ( 'NONE', #32933, 2.000000000000000000 ) ;
#12124 = LINE ( 'NONE', #2168, #7963 ) ;
#12125 = CARTESIAN_POINT ( 'NONE',  ( 1.577395562988744260E-15, 14.24999999453762989, -25.76082449383753925 ) ) ;
#12126 = CARTESIAN_POINT ( 'NONE',  ( -23.41746825000000598, 13.72499999726882258, 7.608796670333726198 ) ) ;
#12127 = CARTESIAN_POINT ( 'NONE',  ( 27.16883889988623935, 24.57500000273119056, -19.73931689729374384 ) ) ;
#12128 = CARTESIAN_POINT ( 'NONE',  ( -26.29305231718579350, 24.30000000546236905, -19.10302069950537884 ) ) ;
#12129 = CARTESIAN_POINT ( 'NONE',  ( 20.08610463437157279, 69.29999999999996874, -27.64615127144129758 ) ) ;
#12130 = CARTESIAN_POINT ( 'NONE',  ( 5.147494310547426899, 47.94874572391553613, -32.50000000000000000 ) ) ;
#12131 = CARTESIAN_POINT ( 'NONE',  ( -6.433434964406110623, 74.00000000000001421, 12.87341652790383861 ) ) ;
#12132 = CARTESIAN_POINT ( 'NONE',  ( 28.00173670424549499, 52.68267333425730214, 7.543491769121417612 ) ) ;
#12133 = CARTESIAN_POINT ( 'NONE',  ( -10.37757302488624411, 36.97500000273118559, -31.93888565452638417 ) ) ;
#12134 = CYLINDRICAL_SURFACE ( 'NONE', #18535, 32.50000000000000000 ) ;
#12135 = CARTESIAN_POINT ( 'NONE',  ( 7.505752307973351023, 27.75520833333332860, 28.01184896238290278 ) ) ;
#12136 =( NAMED_UNIT ( * ) PLANE_ANGLE_UNIT ( ) SI_UNIT ( $, .RADIAN. ) );
#12137 = CARTESIAN_POINT ( 'NONE',  ( 23.41746825000000243, 13.02499999726881619, 7.608796670333735079 ) ) ;
#12138 = CARTESIAN_POINT ( 'NONE',  ( -20.08610463437157989, 17.69999999999999218, -27.64615127144129758 ) ) ;
#12139 = LINE ( 'NONE', #33418, #19801 ) ;
#12140 = CARTESIAN_POINT ( 'NONE',  ( 26.06988505166722803, 46.08295166574269075, -7.025853678916862854 ) ) ;
#12141 = CARTESIAN_POINT ( 'NONE',  ( 27.16883889988623935, 56.32500000273118701, -19.73931689729374384 ) ) ;
#12142 = CARTESIAN_POINT ( 'NONE',  ( -10.37757302488623701, 59.77500000273121117, 31.93888565452638417 ) ) ;
#12143 = CARTESIAN_POINT ( 'NONE',  ( 27.16883889988624290, 46.17500000273119554, 19.73931689729373673 ) ) ;
#12144 = CARTESIAN_POINT ( 'NONE',  ( 32.50000000000000000, 44.99999999999998579, -3.980102097228898626E-15 ) ) ;
#12145 = CARTESIAN_POINT ( 'NONE',  ( 1.076200423132605543E-16, 52.00000000000000711, -46.18802153517007980 ) ) ;
#12146 = LINE ( 'NONE', #14564, #28923 ) ;
#12147 = CARTESIAN_POINT ( 'NONE',  ( 26.09010956794232428, 52.39621500092398065, -6.950374756619718042 ) ) ;
#12148 = CARTESIAN_POINT ( 'NONE',  ( 23.38096321367099151, 16.99999999999997868, 1.514611460525974396 ) ) ;
#12149 = CARTESIAN_POINT ( 'NONE',  ( -32.50000000000000000, 42.09999999999997300, 10.55989012756946366 ) ) ;
#12150 = CARTESIAN_POINT ( 'NONE',  ( 10.37757302488624767, 19.72500000273118204, 31.93888565452638417 ) ) ;
#12151 = CARTESIAN_POINT ( 'NONE',  ( -5.147494310547478413, 62.94874572391552192, 32.49999999999998579 ) ) ;
#12152 = CARTESIAN_POINT ( 'NONE',  ( -15.00000000000000000, 78.35000000546237686, 4.873795443493597723 ) ) ;
#12153 = DIRECTION ( 'NONE',  ( 0.000000000000000000, 0.000000000000000000, -1.000000000000000000 ) ) ;
#12154 = CARTESIAN_POINT ( 'NONE',  ( 26.02091320914876960, 63.70013916574268364, 14.97647472619900455 ) ) ;
#12155 = CARTESIAN_POINT ( 'NONE',  ( -32.50000000000000000, 44.40000000546238823, -10.55989012756945478 ) ) ;
#12156 = ADVANCED_FACE ( 'NONE', ( #11889 ), #33153, .F. ) ;
#12157 = CARTESIAN_POINT ( 'NONE',  ( 5.779280353836490358E-15, 12.49999999999999112, 32.49999999999999289 ) ) ;
#12158 = CARTESIAN_POINT ( 'NONE',  ( -20.75514604977248823, 30.82500000273119412, -28.56700777964554305 ) ) ;
#12159 = CARTESIAN_POINT ( 'NONE',  ( -20.75514604977248823, 65.07500000273118701, -28.56700777964554305 ) ) ;
#12160 = CARTESIAN_POINT ( 'NONE',  ( 19.09188309203661049, 33.48437500000000000, -19.09188309203694445 ) ) ;
#12161 = EDGE_CURVE ( 'NONE', #24826, #6369, #14981, .T. ) ;
#12162 = ORIENTED_EDGE ( 'NONE', *, *, #22557, .T. ) ;
#12163 = CARTESIAN_POINT ( 'NONE',  ( 10.37757302488624767, 69.72500000273117848, 31.93888565452638417 ) ) ;
#12164 = CARTESIAN_POINT ( 'NONE',  ( -28.01184896238304134, 35.77604166666666430, -7.505752307972844761 ) ) ;
#12165 = LINE ( 'NONE', #33091, #16529 ) ;
#12166 = VERTEX_POINT ( 'NONE', #32645 ) ;
#12167 = CARTESIAN_POINT ( 'NONE',  ( -20.47846945139902175, 54.68788166759063785, -20.53372385742072481 ) ) ;
#12168 = CARTESIAN_POINT ( 'NONE',  ( 19.11951029504763611, 58.98475666759065206, -19.06425588902591173 ) ) ;
#12169 = CARTESIAN_POINT ( 'NONE',  ( 33.58253175000000113, 12.22500000273118381, -10.91162601494193751 ) ) ;
#12170 =( BOUNDED_CURVE ( )  B_SPLINE_CURVE ( 2, ( #30631, #14355, #4219, #6461, #25502, #1290, #1982, #27905, #12457, #4387, #14861, #28578, #28916 ),
 .UNSPECIFIED., .F., .T. ) 
 B_SPLINE_CURVE_WITH_KNOTS ( ( 3, 2, 2, 2, 2, 2, 3 ),
 ( 0.6944444444444444198, 0.6999999999999999556, 0.7111111111111111382, 0.7222222222222222099, 0.7333333333333332815, 0.7444444444444444642, 0.7500000000000000000 ),
 .UNSPECIFIED. ) 
 CURVE ( )  GEOMETRIC_REPRESENTATION_ITEM ( )  RATIONAL_B_SPLINE_CURVE ( ( 0.9755282581475768211, 0.9755282581475768211, 1.000000000000000000, 0.9510565162951535312, 1.000000000000000000, 0.9510565162951535312, 1.000000000000000000, 0.9510565162951535312, 1.000000000000000000, 0.9510565162951535312, 1.000000000000000000, 0.9755282581475768211, 0.9755282581475768211 ) ) 
 REPRESENTATION_ITEM ( '' )  );
#12171 = CARTESIAN_POINT ( 'NONE',  ( 28.00173670424535644, 15.14545166574268897, -7.543491769121920321 ) ) ;
#12172 = CARTESIAN_POINT ( 'NONE',  ( -32.50000000000000000, 46.09999999999999432, 10.55989012756946366 ) ) ;
#12173 = CARTESIAN_POINT ( 'NONE',  ( -20.75514604977248112, 39.67500000273118133, 28.56700777964554661 ) ) ;
#12174 = CARTESIAN_POINT ( 'NONE',  ( -2.092463501923844636E-15, 42.00000000546236834, -34.17252228774368916 ) ) ;
#12175 =( BOUNDED_CURVE ( )  B_SPLINE_CURVE ( 2, ( #4046, #12625, #2150, #17783, #22409, #28070, #32857, #10056, #9878, #30460, #24979, #1801, #4726 ),
 .UNSPECIFIED., .F., .F. ) 
 B_SPLINE_CURVE_WITH_KNOTS ( ( 3, 2, 2, 2, 2, 2, 3 ),
 ( 0.8397435897435897578, 0.8410256410256410353, 0.8435897435897435903, 0.8461538461538461453, 0.8487179487179487003, 0.8512820512820512553, 0.8525641025641025328 ),
 .UNSPECIFIED. ) 
 CURVE ( )  GEOMETRIC_REPRESENTATION_ITEM ( )  RATIONAL_B_SPLINE_CURVE ( ( 0.9755282581475768211, 0.9755282581475768211, 1.000000000000000000, 0.9510565162951535312, 1.000000000000000000, 0.9510565162951535312, 1.000000000000000000, 0.9510565162951535312, 1.000000000000000000, 0.9510565162951535312, 1.000000000000000000, 0.9755282581475768211, 0.9755282581475768211 ) ) 
 REPRESENTATION_ITEM ( '' )  );
#12176 = CARTESIAN_POINT ( 'NONE',  ( 8.601468415847516980, 72.67500000273120975, -11.83890561707634781 ) ) ;
#12177 = CARTESIAN_POINT ( 'NONE',  ( -27.16883889988623935, 29.32500000273119412, 19.73931689729374739 ) ) ;
#12178 = CARTESIAN_POINT ( 'NONE',  ( -19.09188309203694445, 67.00000000000000000, -19.09188309203661049 ) ) ;
#12179 = CARTESIAN_POINT ( 'NONE',  ( -10.37757302488623701, 55.77500000273119696, 31.93888565452638417 ) ) ;
#12180 = APPLICATION_PROTOCOL_DEFINITION ( 'draft international standard', 'automotive_design', 1998, #6790 ) ;
#12181 = CARTESIAN_POINT ( 'NONE',  ( 32.50000000000000000, 34.99999999999999289, -3.980102097228898626E-15 ) ) ;
#12182 = CARTESIAN_POINT ( 'NONE',  ( -20.08610463437156923, 36.29999999999997584, 27.64615127144130113 ) ) ;
#12183 = CARTESIAN_POINT ( 'NONE',  ( 15.14183272437242245, 2.299999999999985612, -20.84094480462497856 ) ) ;
#12184 = CARTESIAN_POINT ( 'NONE',  ( 27.16883889988624290, 75.92500000273119554, 19.73931689729373673 ) ) ;
#12185 = CARTESIAN_POINT ( 'NONE',  ( -10.64935084019668743, 66.99999999999997158, 30.92824909085704377 ) ) ;
#12186 = CARTESIAN_POINT ( 'NONE',  ( -26.29305231718579350, 37.79999999999999716, -19.10302069950537884 ) ) ;
#12187 = CARTESIAN_POINT ( 'NONE',  ( 33.58253175000000113, 66.47500000273119269, -10.91162601494193574 ) ) ;
#12188 = CARTESIAN_POINT ( 'NONE',  ( 9.270509831248423538, 79.55000000546240813, -12.75976212528059861 ) ) ;
#12189 = EDGE_LOOP ( 'NONE', ( #23336, #4365 ) ) ;
#12190 = CARTESIAN_POINT ( 'NONE',  ( -10.37757302488623701, 17.52500000273118985, 31.93888565452638417 ) ) ;
#12191 = CARTESIAN_POINT ( 'NONE',  ( -19.82091636218621389, 12.94999999453763628, 14.40073868116558842 ) ) ;
#12192 = CARTESIAN_POINT ( 'NONE',  ( 7.025853678916403666, 24.32329833425730214, -26.06988505166735237 ) ) ;
#12193 = CARTESIAN_POINT ( 'NONE',  ( 7.570916362186213000, 8.149999994537637349, -23.30088464923126423 ) ) ;
#12194 = VECTOR ( 'NONE', #22625, 1000.000000000000000 ) ;
#12195 = CARTESIAN_POINT ( 'NONE',  ( -33.58253175000000113, 41.12500000273118417, 0.000000000000000000 ) ) ;
#12196 = CARTESIAN_POINT ( 'NONE',  ( -33.58253175000000113, 3.475000002731185589, 10.91162601494193929 ) ) ;
#12197 = CARTESIAN_POINT ( 'NONE',  ( 20.75514604977249178, 56.07500000273117990, 28.56700777964553950 ) ) ;
#12198 = CARTESIAN_POINT ( 'NONE',  ( 20.53372385742072481, 48.67225666759065206, -20.47846945139902175 ) ) ;
#12199 = CARTESIAN_POINT ( 'NONE',  ( -7.468012846824272799, 40.35378499907601935, 28.02196122052058413 ) ) ;
#12200 = CARTESIAN_POINT ( 'NONE',  ( -10.04305231718578462, 62.90000000546238113, 30.90933677959249337 ) ) ;
#12201 = EDGE_CURVE ( 'NONE', #564, #1581, #24121, .T. ) ;
#12202 = CARTESIAN_POINT ( 'NONE',  ( 4.300734207923757602, 72.27500000273117564, -13.23629886949340673 ) ) ;
#12203 = CARTESIAN_POINT ( 'NONE',  ( 26.09010956794244507, 63.55690999907603356, 6.950374756619249084 ) ) ;
#12204 = CARTESIAN_POINT ( 'NONE',  ( 11.54700538379251817, 96.00000000000002842, 19.99999999999999645 ) ) ;
#12205 = CARTESIAN_POINT ( 'NONE',  ( 10.04305231718578817, 77.90000000546237402, -30.90933677959249337 ) ) ;
#12206 = CARTESIAN_POINT ( 'NONE',  ( 30.02300923189239512, 16.72656249999999645, -2.619432448724977703E-13 ) ) ;
#12207 = CARTESIAN_POINT ( 'NONE',  ( -20.75514604977248823, 43.07500000273118701, -28.56700777964554305 ) ) ;
#12208 = CARTESIAN_POINT ( 'NONE',  ( 1.507698388325705758E-15, 7.624999997268813168, -24.62258325217400312 ) ) ;
#12209 = VERTEX_POINT ( 'NONE', #10516 ) ;
#12210 = CARTESIAN_POINT ( 'NONE',  ( 10.37757302488624767, 71.97500000273119269, 31.93888565452638417 ) ) ;
#12211 = CARTESIAN_POINT ( 'NONE',  ( 26.29305231718578995, 29.70000000546237118, -19.10302069950538240 ) ) ;
#12212 = ORIENTED_EDGE ( 'NONE', *, *, #30528, .T. ) ;
#12213 = CARTESIAN_POINT ( 'NONE',  ( -20.50609665440969209, 31.76562499999999289, 20.50609665441005092 ) ) ;
#12214 = CARTESIAN_POINT ( 'NONE',  ( -10.04305231718579172, 66.10000000546237686, -30.90933677959248982 ) ) ;
#12215 = ORIENTED_EDGE ( 'NONE', *, *, #12601, .F. ) ;
#12216 = CIRCLE ( 'NONE', #19362, 12.11000150615021909 ) ;
#12217 = CARTESIAN_POINT ( 'NONE',  ( -10.37757302488623701, 45.52500000273118985, 31.93888565452638417 ) ) ;
#12218 = CARTESIAN_POINT ( 'NONE',  ( -32.50000000000000000, 2.400000005462369135, -10.55989012756945478 ) ) ;
#12219 = AXIS2_PLACEMENT_3D ( 'NONE', #21330, #24068, #31771 ) ;
#12220 = CARTESIAN_POINT ( 'NONE',  ( -2.162160676586882350E-15, 64.62500000273121259, -35.31076352940722529 ) ) ;
#12221 = CARTESIAN_POINT ( 'NONE',  ( -7.505752307973343918, 15.72395833333332860, -28.01184896238290989 ) ) ;
#12222 = CARTESIAN_POINT ( 'NONE',  ( 32.50000000000000000, 50.99999999999999289, -3.980102097228898626E-15 ) ) ;
#12223 = CARTESIAN_POINT ( 'NONE',  ( 0.000000000000000000, 2.020667218593133100E-15, -16.50000000000000000 ) ) ;
#12224 = CARTESIAN_POINT ( 'NONE',  ( 33.58253175000000113, 16.37500000273117706, -4.112674001490185761E-15 ) ) ;
#12225 = CARTESIAN_POINT ( 'NONE',  ( 0.000000000000000000, -22.99999999999999289, 0.000000000000000000 ) ) ;
#12226 = CARTESIAN_POINT ( 'NONE',  ( 19.06425588902558133, 21.73399333240935505, -19.11951029504797006 ) ) ;
#12227 = CARTESIAN_POINT ( 'NONE',  ( 4.300734207923761154, 77.47500000273119269, 13.23629886949340495 ) ) ;
#12228 = CARTESIAN_POINT ( 'NONE',  ( -13.91746824999999887, 70.87500000273119838, 0.000000000000000000 ) ) ;
#12229 = DIRECTION ( 'NONE',  ( -1.000000000000000000, 0.000000000000000000, 0.000000000000000000 ) ) ;
#12230 = CARTESIAN_POINT ( 'NONE',  ( 10.04305231718578817, 3.400000000000000355, -30.90933677959249337 ) ) ;
#12231 = VERTEX_POINT ( 'NONE', #28191 ) ;
#12232 = CARTESIAN_POINT ( 'NONE',  ( 7.236395654485760609, 13.52499999726880553, -22.27133577429736633 ) ) ;
#12233 = CARTESIAN_POINT ( 'NONE',  ( 1.469576158976824144E-15, 96.00000000000002842, 12.00000000000000000 ) ) ;
#12234 = CARTESIAN_POINT ( 'NONE',  ( 13.97622843553589966, 47.09114583333332860, -24.20753774853756113 ) ) ;
#12235 = CARTESIAN_POINT ( 'NONE',  ( 33.58253175000000113, 58.22500000273116427, -10.91162601494193751 ) ) ;
#12236 = CARTESIAN_POINT ( 'NONE',  ( 20.75514604977249178, 22.07500000273117990, 28.56700777964553950 ) ) ;
#12237 = CARTESIAN_POINT ( 'NONE',  ( 33.58253175000000113, 10.37500000273118594, -4.112674001490185761E-15 ) ) ;
#12238 = CARTESIAN_POINT ( 'NONE',  ( 33.58253175000000823, 2.275000002731194293, 10.91162601494192685 ) ) ;
#12239 = CARTESIAN_POINT ( 'NONE',  ( 15.04653450569292872, 21.02902750092397710, -25.98046417659857710 ) ) ;
#12240 = CARTESIAN_POINT ( 'NONE',  ( -2.584737979205441561E-13, 60.55468749999999289, -30.02300923189239512 ) ) ;
#12241 = CARTESIAN_POINT ( 'NONE',  ( 6.486482029760649416E-15, 1.625000002731185944, 35.31076352940723240 ) ) ;
#12242 = CARTESIAN_POINT ( 'NONE',  ( 8.601468415847516980, 72.67500000273118133, -11.83890561707634603 ) ) ;
#12243 = CARTESIAN_POINT ( 'NONE',  ( 26.29305231718579350, 40.79999999999999005, 19.10302069950537529 ) ) ;
#12244 = CARTESIAN_POINT ( 'NONE',  ( 27.16883889988624290, 47.92500000273120264, 19.73931689729373673 ) ) ;
#12245 = PRODUCT_DEFINITION ( 'UNKNOWN', '', #5506, #5835 ) ;
#12246 = CARTESIAN_POINT ( 'NONE',  ( -23.41746825000000598, 1.724999997268824581, 7.608796670333726198 ) ) ;
#12247 = DIRECTION ( 'NONE',  ( 1.000000000000000000, 0.000000000000000000, 0.000000000000000000 ) ) ;
#12248 = EDGE_LOOP ( 'NONE', ( #3270, #5223, #16778, #16744 ) ) ;
#12249 = CARTESIAN_POINT ( 'NONE',  ( -20.75514604977248112, 57.67500000273118133, 28.56700777964554661 ) ) ;
#12250 = CARTESIAN_POINT ( 'NONE',  ( -33.58253175000000113, 79.25000000273118417, 0.000000000000000000 ) ) ;
#12251 = CARTESIAN_POINT ( 'NONE',  ( 23.41746825000000243, 12.72499999726882436, -7.608796670333727974 ) ) ;
#12252 = CARTESIAN_POINT ( 'NONE',  ( -0.04044903254992426173, 32.77381916759064495, 27.95245687107223276 ) ) ;
#12253 = VERTEX_POINT ( 'NONE', #196 ) ;
#12254 = CARTESIAN_POINT ( 'NONE',  ( 6.486482029760649416E-15, 27.62500000273118062, 35.31076352940723240 ) ) ;
#12255 = CARTESIAN_POINT ( 'NONE',  ( -10.04305231718578462, 34.90000000546239534, 30.90933677959249337 ) ) ;
#12256 = VERTEX_POINT ( 'NONE', #28526 ) ;
#12257 = CARTESIAN_POINT ( 'NONE',  ( -32.50000000000000000, 36.60000000546239818, 10.55989012756946366 ) ) ;
#12258 = CARTESIAN_POINT ( 'NONE',  ( 20.75514604977248467, 70.42500000273119554, -28.56700777964554305 ) ) ;
#12259 = CARTESIAN_POINT ( 'NONE',  ( -28.01184896238304134, 39.21354166666666430, -7.505752307972844761 ) ) ;
#12260 = CARTESIAN_POINT ( 'NONE',  ( 7.570916362186213000, 10.39999999999999325, -23.30088464923126423 ) ) ;
#12261 = DIRECTION ( 'NONE',  ( -0.000000000000000000, 1.000000000000000000, -0.000000000000000000 ) ) ;
#12262 = CARTESIAN_POINT ( 'NONE',  ( 33.58253175000000823, 10.02500000273118275, 10.91162601494192863 ) ) ;
#12263 = CARTESIAN_POINT ( 'NONE',  ( -1.778240108872766143E-15, 29.50000000000000711, -32.49999999999999289 ) ) ;
#12264 = CARTESIAN_POINT ( 'NONE',  ( -15.04653450569338524, 51.95534749907602645, -25.98046417659831775 ) ) ;
#12265 = CARTESIAN_POINT ( 'NONE',  ( 32.50000000000000711, 36.89999999999999858, 10.55989012756945122 ) ) ;
#12266 = CIRCLE ( 'NONE', #19941, 33.00000000000000000 ) ;
#12267 = CARTESIAN_POINT ( 'NONE',  ( -15.01150461594642316, 56.83072916666665719, -26.00068869287341045 ) ) ;
#12268 = CARTESIAN_POINT ( 'NONE',  ( -15.14183272437242778, 15.04999999453763238, 20.84094480462497856 ) ) ;
#12269 = AXIS2_PLACEMENT_3D ( 'NONE', #21212, #18303, #10735 ) ;
#12270 = CARTESIAN_POINT ( 'NONE',  ( 0.000000000000000000, 96.00000000000002842, 0.000000000000000000 ) ) ;
#12271 = CARTESIAN_POINT ( 'NONE',  ( 19.82091636218621389, 3.949999994537628289, -14.40073868116559197 ) ) ;
#12272 = CARTESIAN_POINT ( 'NONE',  ( 15.00000000000000000, 75.35000000546239107, -4.873795443493596835 ) ) ;
#12273 = CARTESIAN_POINT ( 'NONE',  ( 19.09188309203694800, 27.46875000000000000, 19.09188309203660694 ) ) ;
#12274 =( BOUNDED_CURVE ( )  B_SPLINE_CURVE ( 2, ( #29775, #16430, #22073, #32685, #1280, #9017, #8519, #24475, #27383, #21747, #11759, #9180, #19664 ),
 .UNSPECIFIED., .F., .T. ) 
 B_SPLINE_CURVE_WITH_KNOTS ( ( 3, 2, 2, 2, 2, 2, 3 ),
 ( 0.3611111111111111049, 0.3666666666666666408, 0.3777777777777777679, 0.3888888888888888951, 0.4000000000000000222, 0.4111111111111110938, 0.4166666666666666852 ),
 .UNSPECIFIED. ) 
 CURVE ( )  GEOMETRIC_REPRESENTATION_ITEM ( )  RATIONAL_B_SPLINE_CURVE ( ( 0.9755282581475768211, 0.9755282581475768211, 1.000000000000000000, 0.9510565162951535312, 1.000000000000000000, 0.9510565162951535312, 1.000000000000000000, 0.9510565162951535312, 1.000000000000000000, 0.9510565162951535312, 1.000000000000000000, 0.9755282581475765991, 0.9755282581475767101 ) ) 
 REPRESENTATION_ITEM ( '' )  );
#12275 = CARTESIAN_POINT ( 'NONE',  ( -20.75514604977248823, 38.82500000273120122, -28.56700777964554305 ) ) ;
#12276 = CARTESIAN_POINT ( 'NONE',  ( -27.16883889988624290, 78.92500000273118133, -19.73931689729374028 ) ) ;
#12277 = CARTESIAN_POINT ( 'NONE',  ( 6.486482029760649416E-15, 43.87500000273118417, 35.31076352940723240 ) ) ;
#12278 = CARTESIAN_POINT ( 'NONE',  ( -20.75514604977248112, 23.67500000273118843, 28.56700777964554661 ) ) ;
#12279 = CARTESIAN_POINT ( 'NONE',  ( -24.50000000000000000, 16.64999999453763735, -7.960532557706207157 ) ) ;
#12280 = CARTESIAN_POINT ( 'NONE',  ( -1.778240108872766143E-15, 17.50000000000000000, -32.49999999999999289 ) ) ;
#12281 = DIRECTION ( 'NONE',  ( -1.000000000000000000, -1.416100796715761110E-16, 0.000000000000000000 ) ) ;
#12282 = CARTESIAN_POINT ( 'NONE',  ( 10.04305231718578817, 63.39999999999999858, -30.90933677959249337 ) ) ;
#12283 = CARTESIAN_POINT ( 'NONE',  ( 7.236395654485755280, 12.22499999726881015, 22.27133577429736988 ) ) ;
#12284 = CARTESIAN_POINT ( 'NONE',  ( 20.47846945139867003, 28.60899333240935150, -20.53372385742107653 ) ) ;
#12285 = CARTESIAN_POINT ( 'NONE',  ( 23.41746824999999887, 5.124999997268814056, 0.000000000000000000 ) ) ;
#12286 = CARTESIAN_POINT ( 'NONE',  ( -6.950374756619247307, 33.47878499907601935, 26.09010956794245217 ) ) ;
#12287 = COLOUR_RGB ( '', 0.40784314, 0.44705882, 0.49803922) ;
#12288 = DIRECTION ( 'NONE',  ( 0.000000000000000000, 1.000000000000000000, 0.000000000000000000 ) ) ;
#12289 = CARTESIAN_POINT ( 'NONE',  ( 20.75514604977248467, 12.42500000273119376, -28.56700777964554305 ) ) ;
#12290 = CARTESIAN_POINT ( 'NONE',  ( -23.41746825000000243, 10.02499999726882507, -7.608796670333730638 ) ) ;
#12291 = CARTESIAN_POINT ( 'NONE',  ( -26.07999730980477437, 66.42708333333332860, 6.988114217768305103 ) ) ;
#12292 = ADVANCED_FACE ( 'NONE', ( #5021 ), #20633, .F. ) ;
#12293 = VERTEX_POINT ( 'NONE', #10009 ) ;
#12294 = CARTESIAN_POINT ( 'NONE',  ( 27.16883889988624290, 49.92500000273118843, 19.73931689729373673 ) ) ;
#12295 = CARTESIAN_POINT ( 'NONE',  ( -2.162160676586881955E-15, 20.87500000273119127, -35.31076352940723240 ) ) ;
#12296 = ORIENTED_EDGE ( 'NONE', *, *, #6732, .F. ) ;
#12297 = CARTESIAN_POINT ( 'NONE',  ( 7.505752307973351023, 34.63020833333332860, 28.01184896238290278 ) ) ;
#12298 = CARTESIAN_POINT ( 'NONE',  ( 7.468012846824777284, 32.63059000092395934, 28.02196122052045268 ) ) ;
#12299 = DIRECTION ( 'NONE',  ( 0.000000000000000000, 0.000000000000000000, 1.000000000000000000 ) ) ;
#12300 = CARTESIAN_POINT ( 'NONE',  ( -1.778240108872766143E-15, 18.00000000546237544, -32.49999999999999289 ) ) ;
#12301 = CARTESIAN_POINT ( 'NONE',  ( 23.41746825000000243, 5.024999997268808194, 7.608796670333735079 ) ) ;
#12302 = EDGE_CURVE ( 'NONE', #28216, #21432, #4165, .T. ) ;
#12303 = CARTESIAN_POINT ( 'NONE',  ( -14.47279130897152122, 13.92499999726881654, 19.92008829642072243 ) ) ;
#12304 = CARTESIAN_POINT ( 'NONE',  ( -33.58253175000000113, 19.47500000273117493, 10.91162601494193929 ) ) ;
#12305 = CARTESIAN_POINT ( 'NONE',  ( -10.04305231718578462, 24.90000000546238468, 30.90933677959249337 ) ) ;
#12306 = CARTESIAN_POINT ( 'NONE',  ( 26.29305231718579350, 64.79999999999999716, 19.10302069950537529 ) ) ;
#12307 = DIRECTION ( 'NONE',  ( 0.000000000000000000, -0.000000000000000000, -1.000000000000000000 ) ) ;
#12308 = CARTESIAN_POINT ( 'NONE',  ( -10.13840065261075551, 73.99999999999994316, 10.46602128917086993 ) ) ;
#12309 = CARTESIAN_POINT ( 'NONE',  ( 15.01150461594596308, 12.71614583333333037, -26.00068869287367335 ) ) ;
#12310 = CARTESIAN_POINT ( 'NONE',  ( 10.37757302488624767, 35.97500000273118559, 31.93888565452638417 ) ) ;
#12311 = CARTESIAN_POINT ( 'NONE',  ( 5.147494310547426899, 43.94874572391553613, -32.50000000000000000 ) ) ;
#12312 = CARTESIAN_POINT ( 'NONE',  ( 15.01150461594643382, 27.61197916666666430, 26.00068869287340334 ) ) ;
#12313 = CARTESIAN_POINT ( 'NONE',  ( 0.000000000000000000, 0.000000000000000000, 0.000000000000000000 ) ) ;
#12314 = CARTESIAN_POINT ( 'NONE',  ( -14.47279130897152122, 16.42499999726882365, 19.92008829642072243 ) ) ;
#12315 =( BOUNDED_CURVE ( )  B_SPLINE_CURVE ( 2, ( #9867, #30969, #7468, #25140, #1616, #1788, #28400, #12265, #33192, #7972, #23599, #7802, #28903 ),
 .UNSPECIFIED., .F., .F. ) 
 B_SPLINE_CURVE_WITH_KNOTS ( ( 3, 2, 2, 2, 2, 2, 3 ),
 ( 0.5448717948717948234, 0.5461538461538461009, 0.5487179487179487669, 0.5512820512820513219, 0.5538461538461538769, 0.5564102564102564319, 0.5576923076923077094 ),
 .UNSPECIFIED. ) 
 CURVE ( )  GEOMETRIC_REPRESENTATION_ITEM ( )  RATIONAL_B_SPLINE_CURVE ( ( 0.9755282581475768211, 0.9755282581475768211, 1.000000000000000000, 0.9510565162951535312, 1.000000000000000000, 0.9510565162951535312, 1.000000000000000000, 0.9510565162951535312, 1.000000000000000000, 0.9510565162951535312, 1.000000000000000000, 0.9755282581475768211, 0.9755282581475768211 ) ) 
 REPRESENTATION_ITEM ( '' )  );
#12316 = CARTESIAN_POINT ( 'NONE',  ( -20.08610463437157989, 9.700000000000013500, -27.64615127144129758 ) ) ;
#12317 = STYLED_ITEM ( 'NONE', ( #6341 ), #32241 ) ;
#12318 = CARTESIAN_POINT ( 'NONE',  ( 20.08610463437158344, 9.200000005462387165, 27.64615127144129403 ) ) ;
#12319 = CARTESIAN_POINT ( 'NONE',  ( -27.95245687107223986, 54.81993083240935505, 0.04044903255043252877 ) ) ;
#12320 = CARTESIAN_POINT ( 'NONE',  ( -10.37757302488624411, 54.72500000273117138, -31.93888565452638417 ) ) ;
#12321 = CARTESIAN_POINT ( 'NONE',  ( -27.16883889988624290, 59.17500000273119554, -19.73931689729374028 ) ) ;
#12322 = CARTESIAN_POINT ( 'NONE',  ( 10.37757302488624056, 38.77500000273118275, -31.93888565452638417 ) ) ;
#12323 = CARTESIAN_POINT ( 'NONE',  ( 8.327598234202002696E-15, -91.00000000000000000, 0.000000000000000000 ) ) ;
#12324 = DIRECTION ( 'NONE',  ( -0.000000000000000000, -1.000000000000000000, -0.000000000000000000 ) ) ;
#12325 = PLANE ( 'NONE',  #26750 ) ;
#12326 = CARTESIAN_POINT ( 'NONE',  ( -27.95245687107223986, 47.38319416759065206, -0.04044903254993292840 ) ) ;
#12327 = CARTESIAN_POINT ( 'NONE',  ( -15.14183272437242778, 5.049999994537627934, 20.84094480462497856 ) ) ;
#12328 = FACE_OUTER_BOUND ( 'NONE', #25409, .T. ) ;
#12329 = CARTESIAN_POINT ( 'NONE',  ( -27.16883889988623935, 21.32500000273117280, 19.73931689729374739 ) ) ;
#12330 = LINE ( 'NONE', #14401, #17155 ) ;
#12331 = CARTESIAN_POINT ( 'NONE',  ( -40.00000000000000711, 66.99999999999998579, 23.09401076758504345 ) ) ;
#12332 = CARTESIAN_POINT ( 'NONE',  ( -32.50000000000000000, 78.40000000546234560, -10.55989012756945300 ) ) ;
#12333 = CARTESIAN_POINT ( 'NONE',  ( 28.02196122052058413, 66.99440999907601224, 7.468012846824272799 ) ) ;
#12334 = CARTESIAN_POINT ( 'NONE',  ( -10.04305231718578462, 44.90000000546238823, 30.90933677959249337 ) ) ;
#12335 = CARTESIAN_POINT ( 'NONE',  ( 4.635254915624212657, 70.85000000546237686, 14.26584774442730286 ) ) ;
#12336 = CARTESIAN_POINT ( 'NONE',  ( -10.37757302488624411, 34.72500000273118559, -31.93888565452638417 ) ) ;
#12337 = CARTESIAN_POINT ( 'NONE',  ( -6.988114217768288228, 36.34895833333333570, -26.07999730980477437 ) ) ;
#12338 = VERTEX_POINT ( 'NONE', #25623 ) ;
#12339 = CARTESIAN_POINT ( 'NONE',  ( -27.16883889988623935, 71.32500000273118701, 19.73931689729374739 ) ) ;
#12340 = CARTESIAN_POINT ( 'NONE',  ( 28.01184896238304134, 40.93229166666666430, 7.505752307972846538 ) ) ;
#12341 = MECHANICAL_DESIGN_GEOMETRIC_PRESENTATION_REPRESENTATION (  '', ( #29870 ), #15674 ) ;
#12342 = DIRECTION ( 'NONE',  ( 1.000000000000000000, 0.000000000000000000, 0.000000000000000000 ) ) ;
#12343 = ORIENTED_EDGE ( 'NONE', *, *, #25091, .F. ) ;
#12344 = CARTESIAN_POINT ( 'NONE',  ( -26.02091320914849959, 57.40923583425731636, 14.97647472619947528 ) ) ;
#12345 = CARTESIAN_POINT ( 'NONE',  ( 14.01125832528286352, 58.84152750092397355, -24.18731323226246843 ) ) ;
#12346 = CARTESIAN_POINT ( 'NONE',  ( 20.75514604977249178, 13.82500000273117813, 28.56700777964553950 ) ) ;
#12347 = CARTESIAN_POINT ( 'NONE',  ( 28.00173670424535644, 18.58295166574268364, -7.543491769121920321 ) ) ;
#12348 = CARTESIAN_POINT ( 'NONE',  ( -4.223320258572821363E-15, 78.75000000546236834, 15.00000000000000355 ) ) ;
#12349 = CARTESIAN_POINT ( 'NONE',  ( 6.486482029760649416E-15, 39.87500000273119127, 35.31076352940723240 ) ) ;
#12350 = CARTESIAN_POINT ( 'NONE',  ( 32.50000000000000711, 45.40000000546237402, 10.55989012756945122 ) ) ;
#12351 = CARTESIAN_POINT ( 'NONE',  ( -4.635254915624211769, 77.60000000000000853, -14.26584774442730286 ) ) ;
#12352 = CARTESIAN_POINT ( 'NONE',  ( -27.16883889988623935, 27.32500000273119412, 19.73931689729374739 ) ) ;
#12353 = CARTESIAN_POINT ( 'NONE',  ( 19.82091636218621389, 13.94999999453763806, -14.40073868116559197 ) ) ;
#12354 = CARTESIAN_POINT ( 'NONE',  ( 33.58253175000000823, 54.27500000273118275, 10.91162601494192863 ) ) ;
#12355 = CARTESIAN_POINT ( 'NONE',  ( 20.08610463437157279, 27.29999999999997939, -27.64615127144129758 ) ) ;
#12356 = CARTESIAN_POINT ( 'NONE',  ( 10.04305231718578817, 31.39999999999998437, -30.90933677959249337 ) ) ;
#12357 = CARTESIAN_POINT ( 'NONE',  ( 14.47279130897151589, 16.32499999726882933, 19.92008829642072953 ) ) ;
#12358 = EDGE_CURVE ( 'NONE', #30053, #4440, #20994, .T. ) ;
#12359 = CARTESIAN_POINT ( 'NONE',  ( 27.16883889988623935, 78.32500000273118701, -19.73931689729374384 ) ) ;
#12360 = CARTESIAN_POINT ( 'NONE',  ( 26.29305231718579350, 62.80000000000001137, 19.10302069950537529 ) ) ;
#12361 = CARTESIAN_POINT ( 'NONE',  ( -26.29305231718578995, 20.70000000546237828, 19.10302069950538595 ) ) ;
#12362 = CARTESIAN_POINT ( 'NONE',  ( -33.58253175000000113, 65.47500000273117848, 10.91162601494193929 ) ) ;
#12363 = CARTESIAN_POINT ( 'NONE',  ( -15.00000000000000000, 78.25000000546239676, 0.000000000000000000 ) ) ;
#12364 = CARTESIAN_POINT ( 'NONE',  ( 0.000000000000000000, 80.00000000000001421, -32.50000000000000000 ) ) ;
#12365 = CARTESIAN_POINT ( 'NONE',  ( -33.58253175000000113, 17.22500000273118559, 10.91162601494193929 ) ) ;
#12366 = CARTESIAN_POINT ( 'NONE',  ( 24.50000000000000355, 11.64999999453762314, 7.960532557706212486 ) ) ;
#12367 = CARTESIAN_POINT ( 'NONE',  ( -19.06425588902591173, 16.87538166759064140, -19.11951029504763611 ) ) ;
#12368 = CARTESIAN_POINT ( 'NONE',  ( 26.29305231718578995, 47.19999999999998863, -19.10302069950538240 ) ) ;
#12369 = CARTESIAN_POINT ( 'NONE',  ( -20.75514604977248112, 41.42500000273118133, 28.56700777964554661 ) ) ;
#12370 = CARTESIAN_POINT ( 'NONE',  ( -33.58253175000000113, 7.475000002731190030, 10.91162601494193929 ) ) ;
#12371 = CARTESIAN_POINT ( 'NONE',  ( -33.58253175000000113, 57.27500000273120406, -10.91162601494193041 ) ) ;
#12372 = CARTESIAN_POINT ( 'NONE',  ( -25.98046417659859486, 51.10715250092397355, -15.04653450569291628 ) ) ;
#12373 = CARTESIAN_POINT ( 'NONE',  ( -34.92499999999992610, 3.673940397442066278E-15, -30.00000000000004974 ) ) ;
#12374 = CARTESIAN_POINT ( 'NONE',  ( 28.00173670424535644, 35.77045166574266943, -7.543491769121920321 ) ) ;
#12375 = CARTESIAN_POINT ( 'NONE',  ( 32.50000000000000000, 59.50000000546238965, -3.980102097228898626E-15 ) ) ;
#12376 = CARTESIAN_POINT ( 'NONE',  ( -4.300734207923759378, 72.47500000273116427, -13.23629886949340495 ) ) ;
#12377 = VECTOR ( 'NONE', #15114, 1000.000000000000000 ) ;
#12378 = CARTESIAN_POINT ( 'NONE',  ( -19.11951029504797006, 62.12461833240934794, -19.06425588902558133 ) ) ;
#12379 =( BOUNDED_CURVE ( )  B_SPLINE_CURVE ( 2, ( #7986, #18473, #31325, #12802, #15208, #33737, #33558, #23274, #31496, #20359, #10058, #23094, #5074, #23612, #10234, #25839, #2842, #2680, #13139, #15559, #12626, #20715, #10398, #5417, #15896, #26184, #7300, #26352, #7483, #20538, #31156, #26012, #2504, #17963, #30982, #12972, #7648, #7816, #81, #28412, #33908, #4902, #15730, #2151, #10568, #28243, #15383, #33383, #21047, #17784, #22926, #30805, #9879, #4727, #18134, #23446, #25672, #20877, #18306, #5248, #28750, #18974, #26522, #18644, #16560, #11238, #421, #8653, #3348, #21714, #23952, #19138, #27013, #23785, #24119, #29575, #11077, #21543, #3015, #756, #6076, #32160, #21380, #31825, #10908, #13981, #18806, #29082, #252, #29419, #16066, #31991, #5921, #3510, #16398, #13487, #13818, #24285, #24443, #8487, #5754, #5586, #13311, #10737, #26851, #31659, #3185, #21214, #29251, #8155, #8317, #16235, #26689, #13654, #586, #17613, #20363, #7487, #7304, #15042, #25675, #30810, #20719, #17788, #33563, #31160, #2331, #7652, #2156, #26016, #7133, #23278, #2684, #4731, #25507, #28248, #20881, #28755, #20193, #28416, #10402, #28075, #18310, #12461, #10238, #23099, #12976, #15212, #12630, #10062, #13143, #20542, #1986, #30636, #18138, #22931, #12806, #28582, #5252, #5078, #33387, #4906, #15734, #30987, #15564, #17967, #9884, #2509, #26188, #15387, #9711, #25843, #23451, #33743, #33912, #31330, #7821, #33208, #4564, #13823, #24292, #10741, #31829, #31663, #5421, #16071, #19143, #24124, #2846, #23789, #11244, #21721, #13491, #23956, #32166, #18477, #10912, #13659, #21219, #23616, #8492, #3019, #29581, #8659, #28921, #31996, #3516, #3189, #18648, #21384, #85, #426, #11081, #6083, #16566, #26857, #7992, #27020, #8158, #13316, #8322, #29086, #26693, #18811, #29255, #5758, #10572, #16238, #21051, #18979, #31500, #5590, #16403, #256, #3353, #15901, #26527, #26356, #763, #590, #21550, #29424, #5926, #24776, #27525, #29749, #9157, #11568, #19640, #30252, #11404, #14488, #14155, #6255, #9497, #27695, #32494, #25118, #9317, #4185, #22541, #19979, #24945, #27190, #24612, #1593, #12071, #3846, #14321, #32990, #8823, #1254, #4013, #1086, #13987, #32826, #22048, #30083, #14658, #11734, #16899, #27870, #1428, #8994, #22215, #24449, #32662, #11906, #30425, #6924, #17235, #32331, #17407, #19474, #3682, #6589, #17066, #22378, #29924, #6426, #19804, #6755, #925, #27361, #21881, #19307, #16734, #4869, #30948, #15175, #23063, #12934, #12244, #25469, #7445, #2295, #23240, #10026, #25640, #17929, #20154, #31287, #18094, #20681, #28380, #22722, #2119, #17749, #12592, #20499, #33523, #15349, #25803, #1764, #33871, #12767, #28209, #33700, #20842, #5038, #9847, #10201, #14999, #7614, #23410, #1946, #12422, #22892, #31121, #28541, #15523, #10364, #25975, #2468, #30599, #4695, #7781, #18267, #33170, #4352, #9674, #14828, #25294, #7094, #17578, #28038, #4524, #33349, #20324, #30774, #7264, #13778, #23746, #16361, #8119, #3147, #15694, #28715, #31458, #26145, #13104, #5548, #5380, #29045, #24246, #13619, #18606, #386, #11203, #29384, #211, #23577, #717, #7951, #5720, #16029, #8448, #10698, #21179, #2804, #32579, #21674, #26816, #26652, #10531, #26484, #16198, #9078, #43, #18939, #2641, #10871, #5211, #31621, #24084, #2979, #18438, #31955, #21008, #13447, #28882, #15859, #23914, #3312, #21346, #552, #26315, #13271, #31787, #8278, #18770, #29214, #11038, #21506, #5884, #11989, #15087, #20068, #32746, #19724, #7181, #22632, #17494, #22458, #12336, #27442, #9588, #22977, #25034, #1343, #6513, #32908, #25555, #28123, #14408, #27956, #33436, #33085, #14574, #17320, #19560, #4438, #24862, #9757, #14914, #30170, #2035, #9407, #25380, #6674, #17156, #27614, #30512, #6841, #27783, #4269, #30008, #14743, #16985, #1859, #3934, #11824, #7011, #12158, #30342, #25205, #4611, #22301, #4100, #22806, #33263, #20242, #1682, #30683, #17662, #9239, #12510, #1514, #19890, #26236, #7353, #20763, #23327, #31207, #15612, #7698, #23497, #18184, #17838, #28970, #23145, #20925, #33791, #23665, #25886, #2381, #18015, #13363, #10284, #12676, #30860, #25721, #28627, #31374, #5466, #28293, #128, #4781, #26064, #15948, #12852, #7865, #5125, #33610, #13189, #2896, #2557, #20410, #13024, #18356, #7531, #33955, #28801, #15259, #9933, #10110, #2201, #20589, #31035, #10449, #28461, #4953, #5298, #26403, #15780, #15433, #2725, #31542, #8038, #10619, #21098, #18524, #23837, #24332, #3728, #5802, #16118, #21268, #13701, #6299, #8869, #29133, #8703, #14199, #13867, #29302, #32040, #302, #636, #21767, #19353, #19186, #10955, #16775, #24166, #29624, #21430, #472, #31871, #3397, #21595, #8540, #19024, #10790, #29465, #31711, #6127, #8203, #8368, #27064, #13538, #18693, #29795, #5635, #18854, #26898, #32210, #16611, #5969, #11126, #807, #26571, #16446, #16282, #11288, #3558, #3068, #14031, #26740, #24001, #27235, #24493, #966, #11447, #3233, #21923, #32373, #14530, #30297, #7137, #25334, #30128, #19517, #4568, #4396, #14870, #17277, #14363, #32866, #9542, #29965, #20197, #27913, #9038, #9714, #9197, #24820, #22417, #6798, #27738, #19682, #11780, #14702, #11948, #33038, #1812, #6631, #1638, #4057, #24654, #25160, #22260, #19845, #32702, #1127, #17453, #6472, #12289, #32538, #30640, #17618, #4228, #12114, #28079, #11612, #22762, #6968, #22586, #16944, #1474, #24991, #22094, #33215, #17110, #27402, #20023, #3891, #27569, #1298, #9363, #30469, #10242, #26192, #31163, #7655, #25679, #18314, #23621, #12633, #23103, #2159, #33567, #18482, #28421, #17793, #1990, #26022, #4735, #18142, #2512, #10577, #12980, #15216, #20884, #31333, #7825, #28585, #15390, #33746, #10065, #12809, #23281, #25510, #4910, #23454, #20545, #5082, #28760, #20722, #89, #15568, #5255, #15737, #15046, #25846, #30990, #2336, #21055, #12465, #7490, #33916, #17970, #2687, #13147, #10405, #31505, #7997, #9890, #28926, #22935, #33391, #20367, #30816, #7308, #28252, #6088, #5763, #8327, #16570, #768, #29586, #13827, #29259, #11085, #21885, #27025, #10916, #260, #24453, #18652, #16409, #16242, #19148, #21388, #31833, #13495, #8828, #18816, #8162, #26361, #26862 ),
 .UNSPECIFIED., .F., .F. ) 
 B_SPLINE_CURVE_WITH_KNOTS ( ( 3, 2, 2, 2, 2, 2, 2, 2, 2, 2, 2, 2, 2, 2, 2, 2, 2, 2, 2, 2, 2, 2, 2, 2, 2, 2, 2, 2, 2, 2, 2, 2, 2, 2, 2, 2, 2, 2, 2, 2, 2, 2, 2, 2, 2, 2, 2, 2, 2, 2, 2, 2, 2, 2, 2, 2, 2, 2, 2, 2, 2, 2, 2, 2, 2, 2, 2, 2, 2, 2, 2, 2, 2, 2, 2, 2, 2, 2, 2, 2, 2, 2, 2, 2, 2, 2, 2, 2, 2, 2, 2, 2, 2, 2, 2, 2, 2, 2, 2, 2, 2, 2, 2, 2, 2, 2, 2, 2, 2, 2, 2, 2, 2, 2, 2, 2, 2, 2, 2, 2, 2, 2, 2, 2, 2, 2, 2, 2, 2, 2, 2, 2, 2, 2, 2, 2, 2, 2, 2, 2, 2, 2, 2, 2, 2, 2, 2, 2, 2, 2, 2, 2, 2, 2, 2, 2, 2, 2, 2, 2, 2, 2, 2, 2, 2, 2, 2, 2, 2, 2, 2, 2, 2, 2, 2, 2, 2, 2, 2, 2, 2, 2, 2, 2, 2, 2, 2, 2, 2, 2, 2, 2, 2, 2, 2, 2, 2, 2, 2, 2, 2, 2, 2, 2, 2, 2, 2, 2, 2, 2, 2, 2, 2, 2, 2, 2, 2, 2, 2, 2, 2, 2, 2, 2, 2, 2, 2, 2, 2, 2, 2, 2, 2, 2, 2, 2, 2, 2, 2, 2, 2, 2, 2, 2, 2, 2, 2, 2, 2, 2, 2, 2, 2, 2, 2, 2, 2, 2, 2, 2, 2, 2, 2, 2, 2, 2, 2, 2, 2, 2, 2, 2, 2, 2, 2, 2, 2, 2, 2, 2, 2, 2, 2, 2, 2, 2, 2, 2, 2, 2, 2, 2, 2, 2, 2, 2, 2, 2, 2, 2, 2, 2, 2, 2, 2, 2, 2, 2, 2, 2, 2, 2, 2, 2, 2, 2, 2, 2, 2, 2, 2, 2, 2, 2, 2, 2, 2, 2, 2, 2, 2, 2, 2, 2, 2, 2, 2, 2, 2, 2, 2, 2, 2, 2, 2, 2, 2, 2, 2, 2, 2, 2, 2, 2, 2, 2, 2, 2, 2, 2, 2, 2, 2, 2, 2, 2, 2, 2, 2, 2, 2, 2, 2, 2, 2, 2, 2, 2, 2, 2, 2, 2, 2, 2, 2, 2, 2, 2, 2, 2, 3 ),
 ( 0.000000000000000000, 0.002564102564102564100, 0.005128205128205128201, 0.007692307692307692735, 0.01025641025641025640, 0.01282051282051282007, 0.01538461538461538547, 0.01794871794871794740, 0.02051282051282051280, 0.02307692307692307820, 0.02564102564102564014, 0.02820512820512820554, 0.03076923076923077094, 0.03333333333333333287, 0.03589743589743589480, 0.03846153846153846367, 0.04102564102564102561, 0.04358974358974358754, 0.04615384615384615641, 0.04871794871794871834, 0.05128205128205128027, 0.05384615384615384914, 0.05641025641025641107, 0.05897435897435897301, 0.06153846153846154188, 0.06410256410256409687, 0.06666666666666666574, 0.06923076923076923461, 0.07179487179487178961, 0.07435897435897435848, 0.07692307692307692735, 0.07948717948717948234, 0.08205128205128205121, 0.08461538461538462008, 0.08717948717948717507, 0.08974358974358974395, 0.09230769230769231282, 0.09487179487179486781, 0.09743589743589743668, 0.1000000000000000056, 0.1025641025641025605, 0.1051282051282051294, 0.1076923076923076983, 0.1102564102564102533, 0.1128205128205128221, 0.1153846153846153910, 0.1179487179487179460, 0.1205128205128205149, 0.1230769230769230838, 0.1256410256410256387, 0.1282051282051281937, 0.1307692307692307765, 0.1333333333333333315, 0.1358974358974358865, 0.1384615384615384692, 0.1410256410256410242, 0.1435897435897435792, 0.1461538461538461620, 0.1487179487179487170, 0.1512820512820512719, 0.1538461538461538547, 0.1564102564102564097, 0.1589743589743589647, 0.1615384615384615474, 0.1641025641025641024, 0.1666666666666666574, 0.1692307692307692402, 0.1717948717948717952, 0.1743589743589743501, 0.1769230769230769329, 0.1794871794871794879, 0.1820512820512820429, 0.1846153846153846256, 0.1871794871794871806, 0.1897435897435897356, 0.1923076923076923184, 0.1948717948717948734, 0.1974358974358974284, 0.2000000000000000111, 0.2025641025641025661, 0.2051282051282051211, 0.2076923076923077038, 0.2102564102564102588, 0.2128205128205128138, 0.2153846153846153966, 0.2179487179487179516, 0.2205128205128205066, 0.2230769230769230893, 0.2256410256410256443, 0.2282051282051281993, 0.2307692307692307820, 0.2333333333333333370, 0.2358974358974358920, 0.2384615384615384748, 0.2410256410256410298, 0.2435897435897435848, 0.2461538461538461675, 0.2487179487179487225, 0.2512820512820512775, 0.2538461538461538325, 0.2564102564102563875, 0.2589743589743589980, 0.2615384615384615530, 0.2641025641025641080, 0.2666666666666666630, 0.2692307692307692180, 0.2717948717948717730, 0.2743589743589743835, 0.2769230769230769384, 0.2794871794871794934, 0.2820512820512820484, 0.2846153846153846034, 0.2871794871794871584, 0.2897435897435897689, 0.2923076923076923239, 0.2948717948717948789, 0.2974358974358974339, 0.2999999999999999889, 0.3025641025641025439, 0.3051282051282051544, 0.3076923076923077094, 0.3102564102564102644, 0.3128205128205128194, 0.3153846153846153744, 0.3179487179487179294, 0.3205128205128205399, 0.3230769230769230949, 0.3256410256410256499, 0.3282051282051282048, 0.3307692307692307598, 0.3333333333333333148, 0.3358974358974358698, 0.3384615384615384803, 0.3410256410256410353, 0.3435897435897435903, 0.3461538461538461453, 0.3487179487179487003, 0.3512820512820512553, 0.3538461538461538658, 0.3564102564102564208, 0.3589743589743589758, 0.3615384615384615308, 0.3641025641025640858, 0.3666666666666666408, 0.3692307692307692513, 0.3717948717948718063, 0.3743589743589743613, 0.3769230769230769162, 0.3794871794871794712, 0.3820512820512820262, 0.3846153846153846367, 0.3871794871794871917, 0.3897435897435897467, 0.3923076923076923017, 0.3948717948717948567, 0.3974358974358974117, 0.4000000000000000222, 0.4025641025641025772, 0.4051282051282051322, 0.4076923076923076872, 0.4102564102564102422, 0.4128205128205127972, 0.4153846153846154077, 0.4179487179487179627, 0.4205128205128205177, 0.4230769230769230727, 0.4256410256410256276, 0.4282051282051281826, 0.4307692307692307931, 0.4333333333333333481, 0.4358974358974359031, 0.4384615384615384581, 0.4410256410256410131, 0.4435897435897435681, 0.4461538461538461786, 0.4487179487179487336, 0.4512820512820512886, 0.4538461538461538436, 0.4564102564102563986, 0.4589743589743589536, 0.4615384615384615641, 0.4641025641025641191, 0.4666666666666666741, 0.4692307692307692291, 0.4717948717948717841, 0.4743589743589743390, 0.4769230769230769496, 0.4794871794871795045, 0.4820512820512820595, 0.4846153846153846145, 0.4871794871794871695, 0.4897435897435897245, 0.4923076923076923350, 0.4948717948717948900, 0.4974358974358974450, 0.5000000000000000000, 0.5025641025641025550, 0.5051282051282051100, 0.5076923076923076650, 0.5102564102564102200, 0.5128205128205127750, 0.5153846153846153300, 0.5179487179487179960, 0.5205128205128205510, 0.5230769230769231060, 0.5256410256410256610, 0.5282051282051282159, 0.5307692307692307709, 0.5333333333333333259, 0.5358974358974358809, 0.5384615384615384359, 0.5410256410256409909, 0.5435897435897435459, 0.5461538461538461009, 0.5487179487179487669, 0.5512820512820513219, 0.5538461538461538769, 0.5564102564102564319, 0.5589743589743589869, 0.5615384615384615419, 0.5641025641025640969, 0.5666666666666666519, 0.5692307692307692069, 0.5717948717948717618, 0.5743589743589743168, 0.5769230769230768718, 0.5794871794871795379, 0.5820512820512820928, 0.5846153846153846478, 0.5871794871794872028, 0.5897435897435897578, 0.5923076923076923128, 0.5948717948717948678, 0.5974358974358974228, 0.5999999999999999778, 0.6025641025641025328, 0.6051282051282050878, 0.6076923076923076428, 0.6102564102564103088, 0.6128205128205128638, 0.6153846153846154188, 0.6179487179487179738, 0.6205128205128205288, 0.6230769230769230838, 0.6256410256410256387, 0.6282051282051281937, 0.6307692307692307487, 0.6333333333333333037, 0.6358974358974358587, 0.6384615384615384137, 0.6410256410256410797, 0.6435897435897436347, 0.6461538461538461897, 0.6487179487179487447, 0.6512820512820512997, 0.6538461538461538547, 0.6564102564102564097, 0.6589743589743589647, 0.6615384615384615197, 0.6641025641025640747, 0.6666666666666666297, 0.6692307692307691847, 0.6717948717948717396, 0.6743589743589744057, 0.6769230769230769607, 0.6794871794871795156, 0.6820512820512820706, 0.6846153846153846256, 0.6871794871794871806, 0.6897435897435897356, 0.6923076923076922906, 0.6948717948717948456, 0.6974358974358974006, 0.6999999999999999556, 0.7025641025641025106, 0.7051282051282051766, 0.7076923076923077316, 0.7102564102564102866, 0.7128205128205128416, 0.7153846153846153966, 0.7179487179487179516, 0.7205128205128205066, 0.7230769230769230616, 0.7256410256410256165, 0.7282051282051281715, 0.7307692307692307265, 0.7333333333333332815, 0.7358974358974359475, 0.7384615384615385025, 0.7410256410256410575, 0.7435897435897436125, 0.7461538461538461675, 0.7487179487179487225, 0.7512820512820512775, 0.7538461538461538325, 0.7564102564102563875, 0.7589743589743589425, 0.7615384615384614975, 0.7641025641025640525, 0.7666666666666667185, 0.7692307692307692735, 0.7717948717948718285, 0.7743589743589743835, 0.7769230769230769384, 0.7794871794871794934, 0.7820512820512820484, 0.7846153846153846034, 0.7871794871794871584, 0.7897435897435897134, 0.7923076923076922684, 0.7948717948717948234, 0.7974358974358974894, 0.8000000000000000444, 0.8025641025641025994, 0.8051282051282051544, 0.8076923076923077094, 0.8102564102564102644, 0.8128205128205128194, 0.8153846153846153744, 0.8179487179487179294, 0.8205128205128204844, 0.8230769230769230393, 0.8256410256410255943, 0.8282051282051282604, 0.8307692307692308153, 0.8333333333333333703, 0.8358974358974359253, 0.8384615384615384803, 0.8410256410256410353, 0.8435897435897435903, 0.8461538461538461453, 0.8487179487179487003, 0.8512820512820512553, 0.8538461538461538103, 0.8564102564102563653, 0.8589743589743589203, 0.8615384615384615863, 0.8641025641025641413, 0.8666666666666666963, 0.8692307692307692513, 0.8717948717948718063, 0.8743589743589743613, 0.8769230769230769162, 0.8794871794871794712, 0.8820512820512820262, 0.8846153846153845812, 0.8871794871794871362, 0.8897435897435896912, 0.8923076923076923572, 0.8948717948717949122, 0.8974358974358974672, 0.9000000000000000222, 0.9025641025641025772, 0.9051282051282051322, 0.9076923076923076872, 0.9102564102564102422, 0.9128205128205127972, 0.9153846153846153522, 0.9179487179487179072, 0.9205128205128204621, 0.9230769230769231282, 0.9256410256410256832, 0.9282051282051282382, 0.9307692307692307931, 0.9333333333333333481, 0.9358974358974359031, 0.9384615384615384581, 0.9410256410256410131, 0.9435897435897435681, 0.9461538461538461231, 0.9487179487179486781, 0.9512820512820512331, 0.9538461538461538991, 0.9564102564102564541, 0.9589743589743590091, 0.9615384615384615641, 0.9641025641025641191, 0.9666666666666666741, 0.9692307692307692291, 0.9717948717948717841, 0.9743589743589743390, 0.9769230769230768940, 0.9794871794871794490, 0.9820512820512820040, 0.9846153846153846700, 0.9871794871794872250, 0.9897435897435897800, 0.9923076923076923350, 0.9948717948717948900, 0.9974358974358974450, 1.000000000000000000 ),
 .UNSPECIFIED. ) 
 CURVE ( )  GEOMETRIC_REPRESENTATION_ITEM ( )  RATIONAL_B_SPLINE_CURVE ( ( 1.000000000000000000, 0.9510565162951535312, 1.000000000000000000, 0.9510565162951535312, 1.000000000000000000, 0.9510565162951535312, 1.000000000000000000, 0.9510565162951535312, 1.000000000000000000, 0.9510565162951535312, 1.000000000000000000, 0.9510565162951535312, 1.000000000000000000, 0.9510565162951535312, 1.000000000000000000, 0.9510565162951535312, 1.000000000000000000, 0.9510565162951535312, 1.000000000000000000, 0.9510565162951535312, 1.000000000000000000, 0.9510565162951535312, 1.000000000000000000, 0.9510565162951535312, 1.000000000000000000, 0.9510565162951535312, 1.000000000000000000, 0.9510565162951535312, 1.000000000000000000, 0.9510565162951535312, 1.000000000000000000, 0.9510565162951535312, 1.000000000000000000, 0.9510565162951535312, 1.000000000000000000, 0.9510565162951535312, 1.000000000000000000, 0.9510565162951535312, 1.000000000000000000, 0.9510565162951535312, 1.000000000000000000, 0.9510565162951535312, 1.000000000000000000, 0.9510565162951535312, 1.000000000000000000, 0.9510565162951535312, 1.000000000000000000, 0.9510565162951535312, 1.000000000000000000, 0.9510565162951535312, 1.000000000000000000, 0.9510565162951535312, 1.000000000000000000, 0.9510565162951535312, 1.000000000000000000, 0.9510565162951535312, 1.000000000000000000, 0.9510565162951535312, 1.000000000000000000, 0.9510565162951535312, 1.000000000000000000, 0.9510565162951535312, 1.000000000000000000, 0.9510565162951535312, 1.000000000000000000, 0.9510565162951535312, 1.000000000000000000, 0.9510565162951535312, 1.000000000000000000, 0.9510565162951535312, 1.000000000000000000, 0.9510565162951535312, 1.000000000000000000, 0.9510565162951535312, 1.000000000000000000, 0.9510565162951535312, 1.000000000000000000, 0.9510565162951535312, 1.000000000000000000, 0.9510565162951535312, 1.000000000000000000, 0.9510565162951535312, 1.000000000000000000, 0.9510565162951535312, 1.000000000000000000, 0.9510565162951535312, 1.000000000000000000, 0.9510565162951535312, 1.000000000000000000, 0.9510565162951535312, 1.000000000000000000, 0.9510565162951535312, 1.000000000000000000, 0.9510565162951535312, 1.000000000000000000, 0.9510565162951535312, 1.000000000000000000, 0.9510565162951535312, 1.000000000000000000, 0.9510565162951535312, 1.000000000000000000, 0.9510565162951535312, 1.000000000000000000, 0.9510565162951535312, 1.000000000000000000, 0.9510565162951535312, 1.000000000000000000, 0.9510565162951535312, 1.000000000000000000, 0.9510565162951535312, 1.000000000000000000, 0.9510565162951535312, 1.000000000000000000, 0.9510565162951535312, 1.000000000000000000, 0.9510565162951535312, 1.000000000000000000, 0.9510565162951535312, 1.000000000000000000, 0.9510565162951535312, 1.000000000000000000, 0.9510565162951535312, 1.000000000000000000, 0.9510565162951535312, 1.000000000000000000, 0.9510565162951535312, 1.000000000000000000, 0.9510565162951535312, 1.000000000000000000, 0.9510565162951535312, 1.000000000000000000, 0.9510565162951535312, 1.000000000000000000, 0.9510565162951535312, 1.000000000000000000, 0.9510565162951535312, 1.000000000000000000, 0.9510565162951535312, 1.000000000000000000, 0.9510565162951535312, 1.000000000000000000, 0.9510565162951535312, 1.000000000000000000, 0.9510565162951535312, 1.000000000000000000, 0.9510565162951535312, 1.000000000000000000, 0.9510565162951535312, 1.000000000000000000, 0.9510565162951535312, 1.000000000000000000, 0.9510565162951535312, 1.000000000000000000, 0.9510565162951535312, 1.000000000000000000, 0.9510565162951535312, 1.000000000000000000, 0.9510565162951535312, 1.000000000000000000, 0.9510565162951535312, 1.000000000000000000, 0.9510565162951535312, 1.000000000000000000, 0.9510565162951535312, 1.000000000000000000, 0.9510565162951535312, 1.000000000000000000, 0.9510565162951535312, 1.000000000000000000, 0.9510565162951535312, 1.000000000000000000, 0.9510565162951535312, 1.000000000000000000, 0.9510565162951535312, 1.000000000000000000, 0.9510565162951535312, 1.000000000000000000, 0.9510565162951535312, 1.000000000000000000, 0.9510565162951535312, 1.000000000000000000, 0.9510565162951535312, 1.000000000000000000, 0.9510565162951535312, 1.000000000000000000, 0.9510565162951535312, 1.000000000000000000, 0.9510565162951535312, 1.000000000000000000, 0.9510565162951535312, 1.000000000000000000, 0.9510565162951535312, 1.000000000000000000, 0.9510565162951535312, 1.000000000000000000, 0.9510565162951535312, 1.000000000000000000, 0.9510565162951535312, 1.000000000000000000, 0.9510565162951535312, 1.000000000000000000, 0.9510565162951535312, 1.000000000000000000, 0.9510565162951535312, 1.000000000000000000, 0.9510565162951535312, 1.000000000000000000, 0.9510565162951535312, 1.000000000000000000, 0.9510565162951535312, 1.000000000000000000, 0.9510565162951535312, 1.000000000000000000, 0.9510565162951535312, 1.000000000000000000, 0.9510565162951535312, 1.000000000000000000, 0.9510565162951535312, 1.000000000000000000, 0.9510565162951535312, 1.000000000000000000, 0.9510565162951535312, 1.000000000000000000, 0.9510565162951535312, 1.000000000000000000, 0.9510565162951535312, 1.000000000000000000, 0.9510565162951535312, 1.000000000000000000, 0.9510565162951535312, 1.000000000000000000, 0.9510565162951535312, 1.000000000000000000, 0.9510565162951535312, 1.000000000000000000, 0.9510565162951535312, 1.000000000000000000, 0.9510565162951535312, 1.000000000000000000, 0.9510565162951535312, 1.000000000000000000, 0.9510565162951535312, 1.000000000000000000, 0.9510565162951535312, 1.000000000000000000, 0.9510565162951535312, 1.000000000000000000, 0.9510565162951535312, 1.000000000000000000, 0.9510565162951535312, 1.000000000000000000, 0.9510565162951535312, 1.000000000000000000, 0.9510565162951535312, 1.000000000000000000, 0.9510565162951535312, 1.000000000000000000, 0.9510565162951535312, 1.000000000000000000, 0.9510565162951535312, 1.000000000000000000, 0.9510565162951535312, 1.000000000000000000, 0.9510565162951535312, 1.000000000000000000, 0.9510565162951535312, 1.000000000000000000, 0.9510565162951535312, 1.000000000000000000, 0.9510565162951535312, 1.000000000000000000, 0.9510565162951535312, 1.000000000000000000, 0.9510565162951535312, 1.000000000000000000, 0.9510565162951535312, 1.000000000000000000, 0.9510565162951535312, 1.000000000000000000, 0.9510565162951535312, 1.000000000000000000, 0.9510565162951535312, 1.000000000000000000, 0.9510565162951535312, 1.000000000000000000, 0.9510565162951535312, 1.000000000000000000, 0.9510565162951535312, 1.000000000000000000, 0.9510565162951535312, 1.000000000000000000, 0.9510565162951535312, 1.000000000000000000, 0.9510565162951535312, 1.000000000000000000, 0.9510565162951535312, 1.000000000000000000, 0.9510565162951535312, 1.000000000000000000, 0.9510565162951535312, 1.000000000000000000, 0.9510565162951535312, 1.000000000000000000, 0.9510565162951535312, 1.000000000000000000, 0.9510565162951535312, 1.000000000000000000, 0.9510565162951535312, 1.000000000000000000, 0.9510565162951535312, 1.000000000000000000, 0.9510565162951535312, 1.000000000000000000, 0.9510565162951535312, 1.000000000000000000, 0.9510565162951535312, 1.000000000000000000, 0.9510565162951535312, 1.000000000000000000, 0.9510565162951535312, 1.000000000000000000, 0.9510565162951535312, 1.000000000000000000, 0.9510565162951535312, 1.000000000000000000, 0.9510565162951535312, 1.000000000000000000, 0.9510565162951535312, 1.000000000000000000, 0.9510565162951535312, 1.000000000000000000, 0.9510565162951535312, 1.000000000000000000, 0.9510565162951535312, 1.000000000000000000, 0.9510565162951535312, 1.000000000000000000, 0.9510565162951535312, 1.000000000000000000, 0.9510565162951535312, 1.000000000000000000, 0.9510565162951535312, 1.000000000000000000, 0.9510565162951535312, 1.000000000000000000, 0.9510565162951535312, 1.000000000000000000, 0.9510565162951535312, 1.000000000000000000, 0.9510565162951535312, 1.000000000000000000, 0.9510565162951535312, 1.000000000000000000, 0.9510565162951535312, 1.000000000000000000, 0.9510565162951535312, 1.000000000000000000, 0.9510565162951535312, 1.000000000000000000, 0.9510565162951535312, 1.000000000000000000, 0.9510565162951535312, 1.000000000000000000, 0.9510565162951535312, 1.000000000000000000, 0.9510565162951535312, 1.000000000000000000, 0.9510565162951535312, 1.000000000000000000, 0.9510565162951535312, 1.000000000000000000, 0.9510565162951535312, 1.000000000000000000, 0.9510565162951535312, 1.000000000000000000, 0.9510565162951535312, 1.000000000000000000, 0.9510565162951535312, 1.000000000000000000, 0.9510565162951535312, 1.000000000000000000, 0.9510565162951535312, 1.000000000000000000, 0.9510565162951535312, 1.000000000000000000, 0.9510565162951535312, 1.000000000000000000, 0.9510565162951535312, 1.000000000000000000, 0.9510565162951535312, 1.000000000000000000, 0.9510565162951535312, 1.000000000000000000, 0.9510565162951535312, 1.000000000000000000, 0.9510565162951535312, 1.000000000000000000, 0.9510565162951535312, 1.000000000000000000, 0.9510565162951535312, 1.000000000000000000, 0.9510565162951535312, 1.000000000000000000, 0.9510565162951535312, 1.000000000000000000, 0.9510565162951535312, 1.000000000000000000, 0.9510565162951535312, 1.000000000000000000, 0.9510565162951535312, 1.000000000000000000, 0.9510565162951535312, 1.000000000000000000, 0.9510565162951535312, 1.000000000000000000, 0.9510565162951535312, 1.000000000000000000, 0.9510565162951535312, 1.000000000000000000, 0.9510565162951535312, 1.000000000000000000, 0.9510565162951535312, 1.000000000000000000, 0.9510565162951535312, 1.000000000000000000, 0.9510565162951535312, 1.000000000000000000, 0.9510565162951535312, 1.000000000000000000, 0.9510565162951535312, 1.000000000000000000, 0.9510565162951535312, 1.000000000000000000, 0.9510565162951535312, 1.000000000000000000, 0.9510565162951535312, 1.000000000000000000, 0.9510565162951535312, 1.000000000000000000, 0.9510565162951535312, 1.000000000000000000, 0.9510565162951535312, 1.000000000000000000, 0.9510565162951535312, 1.000000000000000000, 0.9510565162951535312, 1.000000000000000000, 0.9510565162951535312, 1.000000000000000000, 0.9510565162951535312, 1.000000000000000000, 0.9510565162951535312, 1.000000000000000000, 0.9510565162951535312, 1.000000000000000000, 0.9510565162951535312, 1.000000000000000000, 0.9510565162951535312, 1.000000000000000000, 0.9510565162951535312, 1.000000000000000000, 0.9510565162951535312, 1.000000000000000000, 0.9510565162951535312, 1.000000000000000000, 0.9510565162951535312, 1.000000000000000000, 0.9510565162951535312, 1.000000000000000000, 0.9510565162951535312, 1.000000000000000000, 0.9510565162951535312, 1.000000000000000000, 0.9510565162951535312, 1.000000000000000000, 0.9510565162951535312, 1.000000000000000000, 0.9510565162951535312, 1.000000000000000000, 0.9510565162951535312, 1.000000000000000000, 0.9510565162951535312, 1.000000000000000000, 0.9510565162951535312, 1.000000000000000000, 0.9510565162951535312, 1.000000000000000000, 0.9510565162951535312, 1.000000000000000000, 0.9510565162951535312, 1.000000000000000000, 0.9510565162951535312, 1.000000000000000000, 0.9510565162951535312, 1.000000000000000000, 0.9510565162951535312, 1.000000000000000000, 0.9510565162951535312, 1.000000000000000000, 0.9510565162951535312, 1.000000000000000000, 0.9510565162951535312, 1.000000000000000000, 0.9510565162951535312, 1.000000000000000000, 0.9510565162951535312, 1.000000000000000000, 0.9510565162951535312, 1.000000000000000000, 0.9510565162951535312, 1.000000000000000000, 0.9510565162951535312, 1.000000000000000000, 0.9510565162951535312, 1.000000000000000000, 0.9510565162951535312, 1.000000000000000000, 0.9510565162951535312, 1.000000000000000000, 0.9510565162951535312, 1.000000000000000000, 0.9510565162951535312, 1.000000000000000000, 0.9510565162951535312, 1.000000000000000000, 0.9510565162951535312, 1.000000000000000000, 0.9510565162951535312, 1.000000000000000000, 0.9510565162951535312, 1.000000000000000000, 0.9510565162951535312, 1.000000000000000000, 0.9510565162951535312, 1.000000000000000000, 0.9510565162951535312, 1.000000000000000000, 0.9510565162951535312, 1.000000000000000000, 0.9510565162951535312, 1.000000000000000000, 0.9510565162951535312, 1.000000000000000000, 0.9510565162951535312, 1.000000000000000000, 0.9510565162951535312, 1.000000000000000000, 0.9510565162951535312, 1.000000000000000000, 0.9510565162951535312, 1.000000000000000000, 0.9510565162951535312, 1.000000000000000000, 0.9510565162951535312, 1.000000000000000000, 0.9510565162951535312, 1.000000000000000000, 0.9510565162951535312, 1.000000000000000000, 0.9510565162951535312, 1.000000000000000000, 0.9510565162951535312, 1.000000000000000000, 0.9510565162951535312, 1.000000000000000000, 0.9510565162951535312, 1.000000000000000000, 0.9510565162951535312, 1.000000000000000000, 0.9510565162951535312, 1.000000000000000000, 0.9510565162951535312, 1.000000000000000000, 0.9510565162951535312, 1.000000000000000000, 0.9510565162951535312, 1.000000000000000000, 0.9510565162951535312, 1.000000000000000000, 0.9510565162951535312, 1.000000000000000000, 0.9510565162951535312, 1.000000000000000000, 0.9510565162951535312, 1.000000000000000000, 0.9510565162951535312, 1.000000000000000000, 0.9510565162951535312, 1.000000000000000000, 0.9510565162951535312, 1.000000000000000000, 0.9510565162951535312, 1.000000000000000000, 0.9510565162951535312, 1.000000000000000000, 0.9510565162951535312, 1.000000000000000000, 0.9510565162951535312, 1.000000000000000000, 0.9510565162951535312, 1.000000000000000000, 0.9510565162951535312, 1.000000000000000000, 0.9510565162951535312, 1.000000000000000000, 0.9510565162951535312, 1.000000000000000000, 0.9510565162951535312, 1.000000000000000000, 0.9510565162951535312, 1.000000000000000000, 0.9510565162951535312, 1.000000000000000000, 0.9510565162951535312, 1.000000000000000000, 0.9510565162951535312, 1.000000000000000000, 0.9510565162951535312, 1.000000000000000000, 0.9510565162951535312, 1.000000000000000000, 0.9510565162951535312, 1.000000000000000000, 0.9510565162951535312, 1.000000000000000000, 0.9510565162951535312, 1.000000000000000000, 0.9510565162951535312, 1.000000000000000000, 0.9510565162951535312, 1.000000000000000000, 0.9510565162951535312, 1.000000000000000000, 0.9510565162951535312, 1.000000000000000000, 0.9510565162951535312, 1.000000000000000000, 0.9510565162951535312, 1.000000000000000000, 0.9510565162951535312, 1.000000000000000000, 0.9510565162951535312, 1.000000000000000000, 0.9510565162951535312, 1.000000000000000000, 0.9510565162951535312, 1.000000000000000000, 0.9510565162951535312, 1.000000000000000000, 0.9510565162951535312, 1.000000000000000000, 0.9510565162951535312, 1.000000000000000000, 0.9510565162951535312, 1.000000000000000000, 0.9510565162951535312, 1.000000000000000000, 0.9510565162951535312, 1.000000000000000000, 0.9510565162951535312, 1.000000000000000000, 0.9510565162951535312, 1.000000000000000000, 0.9510565162951535312, 1.000000000000000000, 0.9510565162951535312, 1.000000000000000000, 0.9510565162951535312, 1.000000000000000000, 0.9510565162951535312, 1.000000000000000000, 0.9510565162951535312, 1.000000000000000000, 0.9510565162951535312, 1.000000000000000000, 0.9510565162951535312, 1.000000000000000000, 0.9510565162951535312, 1.000000000000000000, 0.9510565162951535312, 1.000000000000000000, 0.9510565162951535312, 1.000000000000000000, 0.9510565162951535312, 1.000000000000000000, 0.9510565162951535312, 1.000000000000000000, 0.9510565162951535312, 1.000000000000000000, 0.9510565162951535312, 1.000000000000000000, 0.9510565162951535312, 1.000000000000000000, 0.9510565162951535312, 1.000000000000000000, 0.9510565162951535312, 1.000000000000000000, 0.9510565162951535312, 1.000000000000000000, 0.9510565162951535312, 1.000000000000000000, 0.9510565162951535312, 1.000000000000000000, 0.9510565162951535312, 1.000000000000000000, 0.9510565162951535312, 1.000000000000000000, 0.9510565162951535312, 1.000000000000000000, 0.9510565162951535312, 1.000000000000000000, 0.9510565162951535312, 1.000000000000000000, 0.9510565162951535312, 1.000000000000000000, 0.9510565162951535312, 1.000000000000000000, 0.9510565162951535312, 1.000000000000000000, 0.9510565162951535312, 1.000000000000000000, 0.9510565162951535312, 1.000000000000000000, 0.9510565162951535312, 1.000000000000000000, 0.9510565162951535312, 1.000000000000000000, 0.9510565162951535312, 1.000000000000000000, 0.9510565162951535312, 1.000000000000000000, 0.9510565162951535312, 1.000000000000000000, 0.9510565162951535312, 1.000000000000000000, 0.9510565162951535312, 1.000000000000000000, 0.9510565162951535312, 1.000000000000000000, 0.9510565162951535312, 1.000000000000000000, 0.9510565162951535312, 1.000000000000000000, 0.9510565162951535312, 1.000000000000000000, 0.9510565162951535312, 1.000000000000000000, 0.9510565162951535312, 1.000000000000000000, 0.9510565162951535312, 1.000000000000000000, 0.9510565162951535312, 1.000000000000000000, 0.9510565162951535312, 1.000000000000000000, 0.9510565162951535312, 1.000000000000000000, 0.9510565162951535312, 1.000000000000000000, 0.9510565162951535312, 1.000000000000000000, 0.9510565162951535312, 1.000000000000000000, 0.9510565162951535312, 1.000000000000000000, 0.9510565162951535312, 1.000000000000000000, 0.9510565162951535312, 1.000000000000000000, 0.9510565162951535312, 1.000000000000000000, 0.9510565162951535312, 1.000000000000000000, 0.9510565162951535312, 1.000000000000000000, 0.9510565162951535312, 1.000000000000000000, 0.9510565162951535312, 1.000000000000000000, 0.9510565162951535312, 1.000000000000000000 ) ) 
 REPRESENTATION_ITEM ( '' )  );
#12380 = CARTESIAN_POINT ( 'NONE',  ( 1.507698388325705758E-15, 1.624999997268798735, -24.62258325217400312 ) ) ;
#12381 = CARTESIAN_POINT ( 'NONE',  ( 32.50000000000000000, 75.50000000546236834, -3.980102097228898626E-15 ) ) ;
#12382 = CARTESIAN_POINT ( 'NONE',  ( -7.505752307973343918, 15.72395833333332860, -28.01184896238290989 ) ) ;
#12383 = CARTESIAN_POINT ( 'NONE',  ( -20.75514604977248823, 35.07500000273120833, -28.56700777964554305 ) ) ;
#12384 = CARTESIAN_POINT ( 'NONE',  ( -7.236395654485763274, 8.524999997268828622, 22.27133577429736633 ) ) ;
#12385 = ORIENTED_EDGE ( 'NONE', *, *, #30248, .F. ) ;
#12386 = CARTESIAN_POINT ( 'NONE',  ( -10.37757302488624411, 74.97500000273119269, -31.93888565452638417 ) ) ;
#12387 = CARTESIAN_POINT ( 'NONE',  ( 10.04305231718579705, 25.10000000546237686, 30.90933677959248982 ) ) ;
#12388 = CARTESIAN_POINT ( 'NONE',  ( 15.01150461594596308, 40.21614583333332860, -26.00068869287367335 ) ) ;
#12389 = CARTESIAN_POINT ( 'NONE',  ( -32.50000000000000000, 64.40000000546238823, -10.55989012756945478 ) ) ;
#12390 = ORIENTED_EDGE ( 'NONE', *, *, #15026, .F. ) ;
#12391 = CARTESIAN_POINT ( 'NONE',  ( -20.08610463437156923, 10.80000000546236372, 27.64615127144130113 ) ) ;
#12392 = CARTESIAN_POINT ( 'NONE',  ( -27.16883889988623935, 49.32500000273118701, 19.73931689729374739 ) ) ;
#12393 = CARTESIAN_POINT ( 'NONE',  ( -14.47279130897151589, 17.32499999726882933, -19.92008829642072598 ) ) ;
#12394 = CARTESIAN_POINT ( 'NONE',  ( -32.50000000000000000, 6.500000005462358565, 0.000000000000000000 ) ) ;
#12395 = CARTESIAN_POINT ( 'NONE',  ( -8.891200544363830713E-16, 77.50000000000001421, -15.00000000000000000 ) ) ;
#12396 = CARTESIAN_POINT ( 'NONE',  ( -2.584737979205442066E-13, 15.86718749999999822, -30.02300923189239867 ) ) ;
#12397 = CARTESIAN_POINT ( 'NONE',  ( 20.08610463437157279, 53.29999999999999716, -27.64615127144129758 ) ) ;
#12398 = EDGE_CURVE ( 'NONE', #25816, #15950, #32111, .T. ) ;
#12399 = CARTESIAN_POINT ( 'NONE',  ( -14.47279130897151589, 1.324999997268808238, -19.92008829642072598 ) ) ;
#12400 = CARTESIAN_POINT ( 'NONE',  ( 33.58253175000000823, 20.27500000273117564, 10.91162601494192863 ) ) ;
#12401 = CARTESIAN_POINT ( 'NONE',  ( -24.50000000000000000, 6.899999999999985256, -7.960532557706207157 ) ) ;
#12402 = CARTESIAN_POINT ( 'NONE',  ( -24.22776226481266448, 24.16888916574269075, -13.94119854578892514 ) ) ;
#12403 = CARTESIAN_POINT ( 'NONE',  ( -4.300734207923759378, 78.97500000273119269, -13.23629886949340495 ) ) ;
#12404 = DIRECTION ( 'NONE',  ( -0.000000000000000000, -1.000000000000000000, -0.000000000000000000 ) ) ;
#12405 = CARTESIAN_POINT ( 'NONE',  ( 26.29305231718579350, 53.30000000546236549, 19.10302069950537529 ) ) ;
#12406 = ADVANCED_FACE ( 'NONE', ( #15158 ), #2790, .T. ) ;
#12407 = CARTESIAN_POINT ( 'NONE',  ( 10.04305231718579705, 4.599999999999992539, 30.90933677959248982 ) ) ;
#12408 = EDGE_LOOP ( 'NONE', ( #20853, #14331 ) ) ;
#12409 = CARTESIAN_POINT ( 'NONE',  ( 7.236395654485755280, 10.72499999726880837, 22.27133577429736988 ) ) ;
#12410 = CARTESIAN_POINT ( 'NONE',  ( 13.91746824999999532, 71.97500000273120691, -4.522059556121118540 ) ) ;
#12411 = CARTESIAN_POINT ( 'NONE',  ( -13.97622843553632421, 49.95572916666665009, -24.20753774853731599 ) ) ;
#12412 = CARTESIAN_POINT ( 'NONE',  ( 10.37757302488624056, 62.52500000273118985, -31.93888565452638417 ) ) ;
#12413 = CARTESIAN_POINT ( 'NONE',  ( -33.58253175000000113, 21.27500000273117209, -10.91162601494193218 ) ) ;
#12414 = CARTESIAN_POINT ( 'NONE',  ( 6.486482029760649416E-15, 11.87500000273118062, 35.31076352940723240 ) ) ;
#12415 = CARTESIAN_POINT ( 'NONE',  ( 24.20753774853756113, 30.76302083333332860, 13.97622843553589789 ) ) ;
#12416 = CARTESIAN_POINT ( 'NONE',  ( -10.37757302488623701, 3.775000002731176973, 31.93888565452638417 ) ) ;
#12417 = CARTESIAN_POINT ( 'NONE',  ( -25.98046417659859486, 23.60715250092398421, -15.04653450569291628 ) ) ;
#12418 = CARTESIAN_POINT ( 'NONE',  ( -15.01150461594595775, 59.12239583333333570, 26.00068869287368756 ) ) ;
#12419 = CARTESIAN_POINT ( 'NONE',  ( -32.50000000000000000, 78.40000000546233139, -10.55989012756945478 ) ) ;
#12420 = LINE ( 'NONE', #27868, #8933 ) ;
#12421 = CARTESIAN_POINT ( 'NONE',  ( 6.277390505771533514E-15, 40.50000000000000711, 34.17252228774368916 ) ) ;
#12422 = CARTESIAN_POINT ( 'NONE',  ( 10.37757302488624056, 44.52500000273118275, -31.93888565452638417 ) ) ;
#12423 = CARTESIAN_POINT ( 'NONE',  ( -23.41746825000000598, 3.724999997268819918, 7.608796670333726198 ) ) ;
#12424 = CARTESIAN_POINT ( 'NONE',  ( -1.089172066684569321E-14, 78.49999999999998579, 15.00000000000000000 ) ) ;
#12425 = ORIENTED_EDGE ( 'NONE', *, *, #19964, .F. ) ;
#12426 = CARTESIAN_POINT ( 'NONE',  ( -2.162160676586881955E-15, 58.87500000273117706, -35.31076352940723240 ) ) ;
#12427 = LINE ( 'NONE', #28721, #12984 ) ;
#12428 = CARTESIAN_POINT ( 'NONE',  ( -14.47279130897152122, 13.92499999726881654, 19.92008829642072243 ) ) ;
#12429 = CARTESIAN_POINT ( 'NONE',  ( -26.06988505166735237, 30.33892333425730925, -7.025853678916388567 ) ) ;
#12430 = CARTESIAN_POINT ( 'NONE',  ( -10.37757302488623701, 77.77500000273118985, 31.93888565452638417 ) ) ;
#12431 = ORIENTED_EDGE ( 'NONE', *, *, #18609, .F. ) ;
#12432 = CARTESIAN_POINT ( 'NONE',  ( 27.16883889988624290, 31.92500000273119909, 19.73931689729373673 ) ) ;
#12434 = CARTESIAN_POINT ( 'NONE',  ( -28.01184896238304134, 15.15104166666666252, -7.505752307972844761 ) ) ;
#12433 = CIRCLE ( 'NONE', #30490, 12.00000000000000000 ) ;
#12435 = VERTEX_POINT ( 'NONE', #28364 ) ;
#12436 = DIRECTION ( 'NONE',  ( -0.000000000000000000, -1.000000000000000000, -0.000000000000000000 ) ) ;
#12437 = CARTESIAN_POINT ( 'NONE',  ( 6.486482029760649416E-15, 65.62500000273116996, 35.31076352940723240 ) ) ;
#12438 = CARTESIAN_POINT ( 'NONE',  ( -26.00068869287368756, 35.91927083333332860, -15.01150461594595775 ) ) ;
#12439 = AXIS2_PLACEMENT_3D ( 'NONE', #21472, #24211, #32418 ) ;
#12440 = CARTESIAN_POINT ( 'NONE',  ( -24.50000000000001066, 13.09999999999999432, 7.960532557706201828 ) ) ;
#12441 = CARTESIAN_POINT ( 'NONE',  ( 23.41746824999999887, 5.224999997268801266, -7.608796670333727974 ) ) ;
#12442 = CARTESIAN_POINT ( 'NONE',  ( -10.37757302488623701, 9.525000002731182747, 31.93888565452638417 ) ) ;
#12443 = CARTESIAN_POINT ( 'NONE',  ( 3.445340210940985210E-14, 7.249999994537621895, 24.50000000000000000 ) ) ;
#12444 = CARTESIAN_POINT ( 'NONE',  ( -28.02196122052058413, 51.52565999907602645, -7.468012846824272799 ) ) ;
#12445 = CARTESIAN_POINT ( 'NONE',  ( -9.270509831248421762, 72.30000000000002558, 12.75976212528060039 ) ) ;
#12446 = CARTESIAN_POINT ( 'NONE',  ( 4.635254915624209993, 81.39999999999997726, -14.26584774442730463 ) ) ;
#12447 = CARTESIAN_POINT ( 'NONE',  ( -20.08610463437156923, 70.30000000000001137, 27.64615127144130113 ) ) ;
#12448 = CARTESIAN_POINT ( 'NONE',  ( -4.635254915624211769, 73.85000000546237686, -14.26584774442730286 ) ) ;
#12449 = CARTESIAN_POINT ( 'NONE',  ( 24.50000000000000355, 11.84999999453761710, -7.960532557706203605 ) ) ;
#12450 = CARTESIAN_POINT ( 'NONE',  ( -15.00000000000000000, 76.35000000546234844, 4.873795443493597723 ) ) ;
#12451 = CARTESIAN_POINT ( 'NONE',  ( 24.20753774853731244, 19.87760416666666430, -13.97622843553632599 ) ) ;
#12452 = CARTESIAN_POINT ( 'NONE',  ( -33.58253175000000113, 33.22500000273117138, 10.91162601494193929 ) ) ;
#12453 = CARTESIAN_POINT ( 'NONE',  ( 27.16883889988623935, 78.32500000273120122, -19.73931689729374384 ) ) ;
#12454 = CARTESIAN_POINT ( 'NONE',  ( 27.16883889988623935, 42.57500000273119412, -19.73931689729374384 ) ) ;
#12455 = CARTESIAN_POINT ( 'NONE',  ( -2.162160676586882350E-15, 18.87500000273119483, -35.31076352940722529 ) ) ;
#12456 = LINE ( 'NONE', #17441, #18469 ) ;
#12457 = CARTESIAN_POINT ( 'NONE',  ( -19.82091636218621389, 14.94999999453763806, 14.40073868116558842 ) ) ;
#12458 = DIRECTION ( 'NONE',  ( -0.000000000000000000, 1.000000000000000000, -0.000000000000000000 ) ) ;
#12459 = CARTESIAN_POINT ( 'NONE',  ( -26.29305231718579350, 61.80000000000000426, -19.10302069950537884 ) ) ;
#12460 = CARTESIAN_POINT ( 'NONE',  ( 23.41746824999999887, 14.72499999726882081, -7.608796670333727974 ) ) ;
#12461 = CARTESIAN_POINT ( 'NONE',  ( -20.75514604977248823, 64.82500000273120122, -28.56700777964554305 ) ) ;
#12462 = CARTESIAN_POINT ( 'NONE',  ( -18.94512977948576093, 2.324999997268817342, 13.76444248337722698 ) ) ;
#12463 = CARTESIAN_POINT ( 'NONE',  ( -26.09010956794245217, 37.77565999907600514, -6.950374756619243755 ) ) ;
#12464 = EDGE_CURVE ( 'NONE', #5395, #25303, #8762, .T. ) ;
#12465 = CARTESIAN_POINT ( 'NONE',  ( -27.16883889988623935, 5.325000002731172799, 19.73931689729374739 ) ) ;
#12466 = CARTESIAN_POINT ( 'NONE',  ( 7.236395654485760609, 13.52499999726880553, -22.27133577429736633 ) ) ;
#12467 = CARTESIAN_POINT ( 'NONE',  ( -24.20753774853730889, 62.84635416666667851, 13.97622843553633842 ) ) ;
#12468 = ORIENTED_EDGE ( 'NONE', *, *, #4225, .T. ) ;
#12469 = CARTESIAN_POINT ( 'NONE',  ( -27.16883889988624290, 48.92500000273118843, -19.73931689729374028 ) ) ;
#12470 = CARTESIAN_POINT ( 'NONE',  ( 10.37757302488624767, 21.97500000273118559, 31.93888565452638417 ) ) ;
#12471 = ORIENTED_EDGE ( 'NONE', *, *, #30528, .F. ) ;
#12472 = CARTESIAN_POINT ( 'NONE',  ( -20.50609665441004736, 36.06250000000000000, -20.50609665440969565 ) ) ;
#12473 = CARTESIAN_POINT ( 'NONE',  ( -20.47846945139902175, 30.62538166759064495, -20.53372385742072481 ) ) ;
#12474 = DIRECTION ( 'NONE',  ( 0.000000000000000000, 1.000000000000000000, 0.000000000000000000 ) ) ;
#12475 = LINE ( 'NONE', #4746, #8520 ) ;
#12476 = CARTESIAN_POINT ( 'NONE',  ( 14.47279130897151767, 3.424999997268800112, -19.92008829642072598 ) ) ;
#12477 = CARTESIAN_POINT ( 'NONE',  ( 1.507698388325705758E-15, 11.12499999726881761, -24.62258325217400312 ) ) ;
#12478 = CARTESIAN_POINT ( 'NONE',  ( 20.75514604977248467, 16.67500000273117777, -28.56700777964554305 ) ) ;
#12479 = CARTESIAN_POINT ( 'NONE',  ( -20.08610463437157989, 24.20000000546238184, -27.64615127144129758 ) ) ;
#12480 =( BOUNDED_CURVE ( )  B_SPLINE_CURVE ( 2, ( #20449, #18049, #4478, #15129, #4818, #7048, #7393, #22044, #25591, #28493, #19636, #6423, #1082 ),
 .UNSPECIFIED., .F., .T. ) 
 B_SPLINE_CURVE_WITH_KNOTS ( ( 3, 2, 2, 2, 2, 2, 3 ),
 ( 0.8611111111111111605, 0.8666666666666666963, 0.8777777777777777679, 0.8888888888888888395, 0.9000000000000000222, 0.9111111111111110938, 0.9166666666666667407 ),
 .UNSPECIFIED. ) 
 CURVE ( )  GEOMETRIC_REPRESENTATION_ITEM ( )  RATIONAL_B_SPLINE_CURVE ( ( 0.9755282581475768211, 0.9755282581475770431, 1.000000000000000000, 0.9510565162951535312, 1.000000000000000000, 0.9510565162951535312, 1.000000000000000000, 0.9510565162951535312, 1.000000000000000000, 0.9510565162951535312, 1.000000000000000000, 0.9755282581475765991, 0.9755282581475768211 ) ) 
 REPRESENTATION_ITEM ( '' )  );
#12481 = CARTESIAN_POINT ( 'NONE',  ( 20.08610463437158344, 64.70000000000001705, 27.64615127144129403 ) ) ;
#12482 = CARTESIAN_POINT ( 'NONE',  ( -2.571758278209442450E-15, -1.999999999999998224, 0.000000000000000000 ) ) ;
#12483 = CARTESIAN_POINT ( 'NONE',  ( -20.52662985655310379, 67.00000000000000000, -26.66963712870534664 ) ) ;
#12484 = CARTESIAN_POINT ( 'NONE',  ( 7.505752307973351023, 14.00520833333333215, 28.01184896238290278 ) ) ;
#12485 = CARTESIAN_POINT ( 'NONE',  ( -20.75514604977248823, 27.07500000273119412, -28.56700777964554305 ) ) ;
#12486 = CARTESIAN_POINT ( 'NONE',  ( 32.50000000000000000, 43.60000000546237686, -10.55989012756945833 ) ) ;
#12487 = CARTESIAN_POINT ( 'NONE',  ( 7.505752307972854531, 29.76041666666666430, -28.01184896238303423 ) ) ;
#12488 = SURFACE_STYLE_FILL_AREA ( #14051 ) ;
#12489 = CARTESIAN_POINT ( 'NONE',  ( 14.47279130897151767, 15.42499999726882898, -19.92008829642072598 ) ) ;
#12490 = CARTESIAN_POINT ( 'NONE',  ( -20.08610463437156923, 6.300000000000004263, 27.64615127144130113 ) ) ;
#12491 = CARTESIAN_POINT ( 'NONE',  ( 15.14183272437241889, 15.69999999999999929, 20.84094480462498211 ) ) ;
#12492 = CARTESIAN_POINT ( 'NONE',  ( -14.01125832528328985, 48.51784749907601935, -24.18731323226223040 ) ) ;
#12493 = CARTESIAN_POINT ( 'NONE',  ( -33.58253175000000113, 49.02500000273116854, -10.91162601494193218 ) ) ;
#12494 = CARTESIAN_POINT ( 'NONE',  ( -10.37757302488624411, 64.97500000273119269, -31.93888565452638417 ) ) ;
#12495 = CARTESIAN_POINT ( 'NONE',  ( -20.75514604977248112, 39.67500000273118133, 28.56700777964554661 ) ) ;
#12496 = CARTESIAN_POINT ( 'NONE',  ( -18.94512977948575738, 15.42499999726881832, -13.76444248337723231 ) ) ;
#12497 = EDGE_CURVE ( 'NONE', #23152, #28001, #2590, .T. ) ;
#12498 = CARTESIAN_POINT ( 'NONE',  ( -6.988114217767819270, 17.72916666666666430, 26.07999730980490583 ) ) ;
#12499 = CARTESIAN_POINT ( 'NONE',  ( 33.58253175000000113, 2.225000002731166937, -10.91162601494193751 ) ) ;
#12500 = CARTESIAN_POINT ( 'NONE',  ( 10.04305231718578817, 63.90000000546238113, -30.90933677959249337 ) ) ;
#12501 = CARTESIAN_POINT ( 'NONE',  ( -20.08610463437157989, 77.70000000000003126, -27.64615127144129758 ) ) ;
#12502 = CARTESIAN_POINT ( 'NONE',  ( -27.16883889988624290, 22.92500000273119198, -19.73931689729374028 ) ) ;
#12503 = CARTESIAN_POINT ( 'NONE',  ( -32.50000000000000000, 62.60000000546238397, 10.55989012756946366 ) ) ;
#12504 = CARTESIAN_POINT ( 'NONE',  ( 10.04305231718578817, 55.90000000546240244, -30.90933677959249337 ) ) ;
#12505 = ADVANCED_FACE ( 'NONE', ( #13053 ), #19973, .T. ) ;
#12506 = DIRECTION ( 'NONE',  ( 0.000000000000000000, 0.000000000000000000, -1.000000000000000000 ) ) ;
#12507 = CARTESIAN_POINT ( 'NONE',  ( -7.543491769121917656, 65.84857666574268364, -28.00173670424536354 ) ) ;
#12508 = CARTESIAN_POINT ( 'NONE',  ( -26.29305231718578995, 38.70000000546237828, 19.10302069950538595 ) ) ;
#12509 = DIRECTION ( 'NONE',  ( -1.000000000000000000, 0.000000000000000000, 0.000000000000000000 ) ) ;
#12510 = CARTESIAN_POINT ( 'NONE',  ( -10.37757302488623701, 29.52500000273117209, 31.93888565452638417 ) ) ;
#12511 = CARTESIAN_POINT ( 'NONE',  ( 19.09188309203694800, 37.78124999999999289, 19.09188309203660694 ) ) ;
#12512 = ADVANCED_FACE ( 'NONE', ( #30592 ), #8908, .T. ) ;
#12513 = ORIENTED_EDGE ( 'NONE', *, *, #28656, .T. ) ;
#12514 = CARTESIAN_POINT ( 'NONE',  ( 27.16883889988624290, 69.92500000273120975, 19.73931689729373673 ) ) ;
#12515 = CARTESIAN_POINT ( 'NONE',  ( -30.02300923189239512, 35.63281249999998579, 2.654126918244515359E-13 ) ) ;
#12516 = CARTESIAN_POINT ( 'NONE',  ( -32.50000000000000000, 16.50000000546236834, 0.000000000000000000 ) ) ;
#12517 = ORIENTED_EDGE ( 'NONE', *, *, #1891, .T. ) ;
#12518 = CARTESIAN_POINT ( 'NONE',  ( 0.04044903254992426173, 61.99256916759065206, -30.02300923189239867 ) ) ;
#12519 = CARTESIAN_POINT ( 'NONE',  ( -19.06425588902591173, 58.12538166759063785, -19.11951029504763611 ) ) ;
#12520 = CARTESIAN_POINT ( 'NONE',  ( -27.16883889988623935, 11.32500000273119234, 19.73931689729374739 ) ) ;
#12521 = CARTESIAN_POINT ( 'NONE',  ( -20.47846945139866648, 20.01524333240935505, 20.53372385742108008 ) ) ;
#12522 = FACE_OUTER_BOUND ( 'NONE', #12408, .T. ) ;
#12523 = CARTESIAN_POINT ( 'NONE',  ( 6.486482029760649416E-15, 31.87500000273119127, 35.31076352940723240 ) ) ;
#12524 = CARTESIAN_POINT ( 'NONE',  ( -32.50000000000000000, 44.60000000546237686, 10.55989012756946366 ) ) ;
#12525 = CARTESIAN_POINT ( 'NONE',  ( -12.13525491562421088, 75.80000000000003979, -8.816778784387096835 ) ) ;
#12526 = CARTESIAN_POINT ( 'NONE',  ( 33.58253175000000113, 20.22500000273117848, -10.91162601494193751 ) ) ;
#12527 = DIRECTION ( 'NONE',  ( 0.7071067811865526798, 0.000000000000000000, 0.7071067811865423547 ) ) ;
#12528 = CARTESIAN_POINT ( 'NONE',  ( 20.75514604977249178, 50.07500000273120122, 28.56700777964553950 ) ) ;
#12529 =( LENGTH_UNIT ( ) NAMED_UNIT ( * ) SI_UNIT ( .MILLI., .METRE. ) );
#12530 = CARTESIAN_POINT ( 'NONE',  ( 32.50000000000000711, 28.89999999999998792, 10.55989012756945122 ) ) ;
#12531 = CARTESIAN_POINT ( 'NONE',  ( -26.29305231718578995, 28.20000000000000284, 19.10302069950538595 ) ) ;
#12532 = CARTESIAN_POINT ( 'NONE',  ( 7.236395654485755280, 16.22499999726881370, 22.27133577429736988 ) ) ;
#12533 = CARTESIAN_POINT ( 'NONE',  ( -27.16883889988623935, 75.32500000273117280, 19.73931689729374739 ) ) ;
#12534 = CARTESIAN_POINT ( 'NONE',  ( 0.000000000000000000, 0.000000000000000000, 0.000000000000000000 ) ) ;
#12535 = CARTESIAN_POINT ( 'NONE',  ( -26.29305231718579350, 20.30000000546239391, -19.10302069950537884 ) ) ;
#12536 = CARTESIAN_POINT ( 'NONE',  ( -20.75514604977248823, 59.07500000273120122, -28.56700777964554305 ) ) ;
#12537 = CARTESIAN_POINT ( 'NONE',  ( -4.635254915624208216, 74.65000000546240244, 14.26584774442730463 ) ) ;
#12538 = EDGE_LOOP ( 'NONE', ( #31169, #32586, #11044, #24131 ) ) ;
#12539 = CARTESIAN_POINT ( 'NONE',  ( -27.16883889988623935, 21.32500000273118701, 19.73931689729374739 ) ) ;
#12540 = CARTESIAN_POINT ( 'NONE',  ( 24.50000000000000355, 9.649999994537628467, 7.960532557706212486 ) ) ;
#12541 = CARTESIAN_POINT ( 'NONE',  ( -0.04044903254992426173, 19.02381916759064495, 27.95245687107223276 ) ) ;
#12542 = CARTESIAN_POINT ( 'NONE',  ( -10.04305231718578462, 26.40000000000000568, 30.90933677959249337 ) ) ;
#12543 = CARTESIAN_POINT ( 'NONE',  ( 33.58253175000000113, 40.22500000273119269, -10.91162601494193751 ) ) ;
#12544 = CARTESIAN_POINT ( 'NONE',  ( -5.147494310547430452, 64.05125428700922896, -32.49999999999999289 ) ) ;
#12545 = CARTESIAN_POINT ( 'NONE',  ( 20.75514604977249178, 54.07500000273118701, 28.56700777964553950 ) ) ;
#12546 = CARTESIAN_POINT ( 'NONE',  ( -20.47846945139902175, 47.81288166759064495, -20.53372385742072481 ) ) ;
#12547 = LINE ( 'NONE', #12373, #33482 ) ;
#12548 = CARTESIAN_POINT ( 'NONE',  ( 28.00173670424535644, 39.20795166574269075, -7.543491769121920321 ) ) ;
#12549 = CARTESIAN_POINT ( 'NONE',  ( 20.08610463437157279, 57.80000000546236549, -27.64615127144129758 ) ) ;
#12550 = CARTESIAN_POINT ( 'NONE',  ( 4.300734207923761154, 71.47500000273116427, 13.23629886949340495 ) ) ;
#12551 = CARTESIAN_POINT ( 'NONE',  ( 19.82091636218621389, 7.949999994537631842, -14.40073868116559197 ) ) ;
#12552 = CARTESIAN_POINT ( 'NONE',  ( 6.950374756619257965, 66.13503499907601224, -26.09010956794244507 ) ) ;
#12553 = CARTESIAN_POINT ( 'NONE',  ( -1.778240108872766143E-15, 53.50000000000000000, -32.49999999999999289 ) ) ;
#12554 = CARTESIAN_POINT ( 'NONE',  ( -10.37757302488623701, 1.525000002731202731, 31.93888565452638417 ) ) ;
#12555 = FACE_OUTER_BOUND ( 'NONE', #26279, .T. ) ;
#12556 = CARTESIAN_POINT ( 'NONE',  ( -33.58253175000000113, 35.47500000273118559, 10.91162601494193929 ) ) ;
#12557 = CARTESIAN_POINT ( 'NONE',  ( -18.94512977948576093, 8.324999997268822227, 13.76444248337722698 ) ) ;
#12558 = ORIENTED_EDGE ( 'NONE', *, *, #22470, .F. ) ;
#12559 = CARTESIAN_POINT ( 'NONE',  ( -20.75514604977248112, 73.67500000273120975, 28.56700777964554661 ) ) ;
#12560 = CARTESIAN_POINT ( 'NONE',  ( -10.04305231718579172, 24.10000000546237686, -30.90933677959248982 ) ) ;
#12561 = CARTESIAN_POINT ( 'NONE',  ( 26.00068869287367335, 41.07552083333331439, 15.01150461594596308 ) ) ;
#12562 = CARTESIAN_POINT ( 'NONE',  ( 20.08610463437158344, 61.20000000546237118, 27.64615127144129403 ) ) ;
#12563 = VERTEX_POINT ( 'NONE', #28997 ) ;
#12564 = CARTESIAN_POINT ( 'NONE',  ( 0.000000000000000000, 16.99999999999998579, 0.000000000000000000 ) ) ;
#12565 = CARTESIAN_POINT ( 'NONE',  ( -10.37757302488624411, 40.72500000273118559, -31.93888565452638417 ) ) ;
#12566 = CARTESIAN_POINT ( 'NONE',  ( 14.47279130897151767, 16.92499999726880944, -19.92008829642072598 ) ) ;
#12567 = CARTESIAN_POINT ( 'NONE',  ( 32.50000000000000000, 5.600000005462384856, -10.55989012756945833 ) ) ;
#12568 = CARTESIAN_POINT ( 'NONE',  ( -32.50000000000000000, 8.000000000000007105, 0.000000000000000000 ) ) ;
#12569 = CARTESIAN_POINT ( 'NONE',  ( 26.00068869287367690, 13.57552083333333037, 15.01150461594596486 ) ) ;
#12570 = CARTESIAN_POINT ( 'NONE',  ( 26.29305231718579350, 46.80000000000001137, 19.10302069950537529 ) ) ;
#12571 = DIRECTION ( 'NONE',  ( -0.000000000000000000, -1.000000000000000000, -0.000000000000000000 ) ) ;
#12572 = CARTESIAN_POINT ( 'NONE',  ( -2.162160676586881955E-15, 14.87500000273120193, -35.31076352940723240 ) ) ;
#12573 = CARTESIAN_POINT ( 'NONE',  ( -10.04305231718579172, 24.10000000546236265, -30.90933677959248982 ) ) ;
#12574 = CARTESIAN_POINT ( 'NONE',  ( 26.09010956794244507, 22.30690999907601579, 6.950374756619249084 ) ) ;
#12575 = CARTESIAN_POINT ( 'NONE',  ( 4.300734207923761154, 79.97500000273119269, 13.23629886949340495 ) ) ;
#12576 = CARTESIAN_POINT ( 'NONE',  ( -10.37757302488624411, 78.97500000273119269, -31.93888565452638417 ) ) ;
#12577 = CARTESIAN_POINT ( 'NONE',  ( 31.04172217648528687, 52.00000000000000711, 12.81397374188273908 ) ) ;
#12578 = CARTESIAN_POINT ( 'NONE',  ( 6.486482029760649416E-15, 73.87500000273119838, 35.31076352940723240 ) ) ;
#12579 = EDGE_LOOP ( 'NONE', ( #18359, #266, #2690, #10117 ) ) ;
#12580 = CARTESIAN_POINT ( 'NONE',  ( 18.94512977948576093, 13.32499999726879913, -13.76444248337722875 ) ) ;
#12581 = CARTESIAN_POINT ( 'NONE',  ( 23.41746824999999887, 4.724999997268818142, -7.608796670333727974 ) ) ;
#12582 = CARTESIAN_POINT ( 'NONE',  ( -24.20753774853730889, 52.53385416666666430, 13.97622843553633842 ) ) ;
#12583 = CARTESIAN_POINT ( 'NONE',  ( 33.58253175000000823, 62.02500000273116143, 10.91162601494192863 ) ) ;
#12584 = CARTESIAN_POINT ( 'NONE',  ( 33.58253175000000113, 22.47500000273119625, -10.91162601494193751 ) ) ;
#12585 = CARTESIAN_POINT ( 'NONE',  ( 27.16883889988624290, 12.17500000273118133, 19.73931689729373673 ) ) ;
#12586 = CARTESIAN_POINT ( 'NONE',  ( -26.07999730980490583, 32.33854166666666430, -6.988114217767815717 ) ) ;
#12587 = CARTESIAN_POINT ( 'NONE',  ( -25.98046417659859486, 16.73215250092398065, -15.04653450569291628 ) ) ;
#12588 = CARTESIAN_POINT ( 'NONE',  ( 30.02300923189239512, 64.85156249999998579, -2.619432448724977703E-13 ) ) ;
#12589 = CARTESIAN_POINT ( 'NONE',  ( -27.16883889988623935, 3.325000002731184789, 19.73931689729374739 ) ) ;
#12590 = DIRECTION ( 'NONE',  ( -0.000000000000000000, -1.000000000000000000, -0.000000000000000000 ) ) ;
#12591 = CARTESIAN_POINT ( 'NONE',  ( -32.50000000000000000, 40.09999999999998721, 10.55989012756946366 ) ) ;
#12592 = CARTESIAN_POINT ( 'NONE',  ( 27.16883889988623935, 46.32500000273117990, -19.73931689729374384 ) ) ;
#12593 = CARTESIAN_POINT ( 'NONE',  ( -18.94512977948576093, 7.824999997268822227, 13.76444248337722698 ) ) ;
#12594 = CARTESIAN_POINT ( 'NONE',  ( -24.20753774853730889, 66.28385416666664298, 13.97622843553634020 ) ) ;
#12595 = ORIENTED_EDGE ( 'NONE', *, *, #26240, .F. ) ;
#12596 = EDGE_CURVE ( 'NONE', #13948, #26987, #32413, .T. ) ;
#12597 = CARTESIAN_POINT ( 'NONE',  ( -33.58253175000000113, 55.47500000273119980, 10.91162601494193929 ) ) ;
#12598 = CARTESIAN_POINT ( 'NONE',  ( 5.779280353836490358E-15, 42.49999999999999289, 32.49999999999999289 ) ) ;
#12599 = CARTESIAN_POINT ( 'NONE',  ( 14.01125832528286352, 45.09152750092398065, -24.18731323226246843 ) ) ;
#12600 = CARTESIAN_POINT ( 'NONE',  ( -20.75514604977248112, 75.67500000273118133, 28.56700777964554661 ) ) ;
#12601 = EDGE_CURVE ( 'NONE', #19251, #5367, #7669, .T. ) ;
#12602 = EDGE_LOOP ( 'NONE', ( #27155, #2083, #12681, #9855, #2517, #28469 ) ) ;
#12603 = CARTESIAN_POINT ( 'NONE',  ( -33.58253175000000113, 21.02500000273117919, -10.91162601494193218 ) ) ;
#12604 = CARTESIAN_POINT ( 'NONE',  ( 26.00068869287367335, 13.57552083333332682, 15.01150461594596308 ) ) ;
#12605 = ORIENTED_EDGE ( 'NONE', *, *, #20503, .T. ) ;
#12606 = CARTESIAN_POINT ( 'NONE',  ( 0.000000000000000000, 70.00000000000000000, 0.000000000000000000 ) ) ;
#12607 = CARTESIAN_POINT ( 'NONE',  ( -10.37757302488624411, 68.72500000273117848, -31.93888565452638417 ) ) ;
#12608 = CARTESIAN_POINT ( 'NONE',  ( 26.00068869287340334, 40.50260416666666430, -15.01150461594642316 ) ) ;
#12609 = CARTESIAN_POINT ( 'NONE',  ( 24.50000000000000000, 12.00000000000001066, 0.000000000000000000 ) ) ;
#12610 = LINE ( 'NONE', #2311, #30862 ) ;
#12611 = CARTESIAN_POINT ( 'NONE',  ( 10.37757302488624767, 11.72500000273118914, 31.93888565452638417 ) ) ;
#12612 = CARTESIAN_POINT ( 'NONE',  ( 3.469446951953614189E-15, -57.99999999999999289, 0.000000000000000000 ) ) ;
#12613 = CARTESIAN_POINT ( 'NONE',  ( 28.00173670424535644, 52.95795166574269075, -7.543491769121920321 ) ) ;
#12614 = CARTESIAN_POINT ( 'NONE',  ( 9.270509831248425314, 72.70000000000001705, 12.75976212528059683 ) ) ;
#12615 = CARTESIAN_POINT ( 'NONE',  ( 26.29305231718578995, 65.70000000546237118, -19.10302069950538240 ) ) ;
#12616 = CARTESIAN_POINT ( 'NONE',  ( 10.04305231718578817, 55.39999999999999147, -30.90933677959249337 ) ) ;
#12617 = CARTESIAN_POINT ( 'NONE',  ( -32.50000000000000000, 52.00000000000000711, 0.000000000000000000 ) ) ;
#12618 = CARTESIAN_POINT ( 'NONE',  ( 7.570916362186213000, 16.14999999453761603, -23.30088464923126423 ) ) ;
#12619 = CARTESIAN_POINT ( 'NONE',  ( -15.00000000000000000, 72.35000000546236265, 4.873795443493597723 ) ) ;
#12620 = CARTESIAN_POINT ( 'NONE',  ( 24.20753774853731244, 23.31510416666666430, -13.97622843553632599 ) ) ;
#12621 = CARTESIAN_POINT ( 'NONE',  ( 33.58253175000000113, 28.22500000273119269, -10.91162601494193751 ) ) ;
#12622 = CARTESIAN_POINT ( 'NONE',  ( 10.37757302488624767, 77.72500000273117848, 31.93888565452638417 ) ) ;
#12623 = CARTESIAN_POINT ( 'NONE',  ( -2.162160676586881955E-15, 42.87500000273119127, -35.31076352940723240 ) ) ;
#12624 = CARTESIAN_POINT ( 'NONE',  ( -20.75514604977248112, 19.67500000273119909, 28.56700777964554661 ) ) ;
#12625 = CARTESIAN_POINT ( 'NONE',  ( -5.147494310547423346, 12.94874572391553258, 32.50000000000000000 ) ) ;
#12626 = CARTESIAN_POINT ( 'NONE',  ( -33.58253175000000113, 77.12500000273119838, 0.000000000000000000 ) ) ;
#12627 = CARTESIAN_POINT ( 'NONE',  ( 0.000000000000000000, 102.0000000000000284, 0.000000000000000000 ) ) ;
#12628 = CARTESIAN_POINT ( 'NONE',  ( -10.04305231718579172, 61.60000000000000142, -30.90933677959248982 ) ) ;
#12629 = CARTESIAN_POINT ( 'NONE',  ( 14.47279130897151767, 16.32499999726879736, 19.92008829642072953 ) ) ;
#12630 = CARTESIAN_POINT ( 'NONE',  ( 27.16883889988623935, 64.32500000273120122, -19.73931689729374384 ) ) ;
#12631 = CARTESIAN_POINT ( 'NONE',  ( 23.41746825000000243, 11.02499999726882152, 7.608796670333735079 ) ) ;
#12632 = CARTESIAN_POINT ( 'NONE',  ( -2.162160676586881955E-15, 72.87500000273115575, -35.31076352940723240 ) ) ;
#12633 = CARTESIAN_POINT ( 'NONE',  ( -27.16883889988623935, 9.325000002731176352, 19.73931689729374739 ) ) ;
#12634 = CARTESIAN_POINT ( 'NONE',  ( -14.47279130897151589, 13.82499999726882045, -19.92008829642072598 ) ) ;
#12635 = CARTESIAN_POINT ( 'NONE',  ( -27.95245687107223986, 16.44569416759064140, -0.04044903254993292840 ) ) ;
#12636 = EDGE_LOOP ( 'NONE', ( #6701, #15535, #20726, #21888 ) ) ;
#12637 = CARTESIAN_POINT ( 'NONE',  ( 10.37757302488624767, 47.72500000273117848, 31.93888565452638417 ) ) ;
#12638 = ORIENTED_EDGE ( 'NONE', *, *, #26046, .T. ) ;
#12639 = CARTESIAN_POINT ( 'NONE',  ( -30.02300923189239512, 35.63281249999998579, 2.654126918244515359E-13 ) ) ;
#12640 = CARTESIAN_POINT ( 'NONE',  ( 15.14183272437242067, 9.699999999999985079, 20.84094480462498211 ) ) ;
#12641 = CARTESIAN_POINT ( 'NONE',  ( -10.04305231718578462, 2.900000005462380237, 30.90933677959249337 ) ) ;
#12642 = CARTESIAN_POINT ( 'NONE',  ( -15.14183272437242067, 8.449999994537638059, -20.84094480462497856 ) ) ;
#12643 = CARTESIAN_POINT ( 'NONE',  ( 7.236395654485760609, 3.524999997268824181, -22.27133577429736633 ) ) ;
#12644 = CARTESIAN_POINT ( 'NONE',  ( 18.94512977948576093, 14.82499999726882933, -13.76444248337722875 ) ) ;
#12645 = CARTESIAN_POINT ( 'NONE',  ( -10.37757302488623701, 15.77500000273118808, 31.93888565452638417 ) ) ;
#12646 = CARTESIAN_POINT ( 'NONE',  ( -10.04305231718578462, 20.90000000546238113, 30.90933677959249337 ) ) ;
#12647 = CARTESIAN_POINT ( 'NONE',  ( -20.08610463437157989, 65.69999999999998863, -27.64615127144129758 ) ) ;
#12648 = CARTESIAN_POINT ( 'NONE',  ( 5.779280353836490358E-15, 7.000000005462371000, 32.49999999999999289 ) ) ;
#12649 = LINE ( 'NONE', #13844, #20973 ) ;
#12650 = CARTESIAN_POINT ( 'NONE',  ( -28.01184896238290278, 14.86458333333333037, 7.505752307973363457 ) ) ;
#12651 = CARTESIAN_POINT ( 'NONE',  ( 27.16883889988624290, 32.17500000273118843, 19.73931689729373673 ) ) ;
#12652 = CARTESIAN_POINT ( 'NONE',  ( -8.960552108402742093E-16, 80.87500000273116996, -14.63369212191046387 ) ) ;
#12653 = CARTESIAN_POINT ( 'NONE',  ( -28.01184896238304134, 39.21354166666666430, -7.505752307972844761 ) ) ;
#12654 = DIRECTION ( 'NONE',  ( 1.000000000000000000, 0.000000000000000000, 0.000000000000000000 ) ) ;
#12655 = ADVANCED_FACE ( 'NONE', ( #32071 ), #6158, .T. ) ;
#12656 = CARTESIAN_POINT ( 'NONE',  ( -23.41746825000000243, 14.02499999726881263, -7.608796670333730638 ) ) ;
#12657 = CARTESIAN_POINT ( 'NONE',  ( 20.08610463437157279, 5.300000000000006928, -27.64615127144129758 ) ) ;
#12658 = DIRECTION ( 'NONE',  ( 1.000000000000000000, 0.000000000000000000, 0.000000000000000000 ) ) ;
#12659 = CARTESIAN_POINT ( 'NONE',  ( -19.06425588902558133, 50.95274333240935505, 19.11951029504797006 ) ) ;
#12660 = CARTESIAN_POINT ( 'NONE',  ( -20.75514604977248112, 53.42500000273117422, 28.56700777964554661 ) ) ;
#12661 = CARTESIAN_POINT ( 'NONE',  ( -27.16883889988624290, 61.17500000273119554, -19.73931689729374028 ) ) ;
#12662 = CARTESIAN_POINT ( 'NONE',  ( -10.37757302488624411, 42.97500000273119269, -31.93888565452638417 ) ) ;
#12663 = CARTESIAN_POINT ( 'NONE',  ( -18.94512977948576093, 15.82499999726880091, 13.76444248337722698 ) ) ;
#12664 = CARTESIAN_POINT ( 'NONE',  ( 6.988114217767829928, 12.57291666666666252, -26.07999730980489872 ) ) ;
#12665 = CARTESIAN_POINT ( 'NONE',  ( -3.880418787951142701, 9.448745718453144704, 24.49999999999999645 ) ) ;
#12666 = AXIS2_PLACEMENT_3D ( 'NONE', #20239, #30679, #12506 ) ;
#12667 = CARTESIAN_POINT ( 'NONE',  ( -32.50000000000000000, 22.60000000546237331, 10.55989012756946366 ) ) ;
#12668 = CARTESIAN_POINT ( 'NONE',  ( 26.29305231718579350, 78.79999999999999716, 19.10302069950537529 ) ) ;
#12669 = CARTESIAN_POINT ( 'NONE',  ( -10.37757302488623701, 13.52500000273119873, 31.93888565452638417 ) ) ;
#12670 = CARTESIAN_POINT ( 'NONE',  ( 32.50000000000000000, 7.100000000000008527, -10.55989012756945833 ) ) ;
#12671 = CYLINDRICAL_SURFACE ( 'NONE', #17750, 24.50000000000000000 ) ;
#12672 = DIRECTION ( 'NONE',  ( 0.000000000000000000, 0.000000000000000000, -1.000000000000000000 ) ) ;
#12673 = CARTESIAN_POINT ( 'NONE',  ( 24.18731323226221974, 18.43972249907602290, -14.01125832528328985 ) ) ;
#12674 = CARTESIAN_POINT ( 'NONE',  ( -10.04305231718578462, 40.90000000546238823, 30.90933677959249337 ) ) ;
#12675 = CARTESIAN_POINT ( 'NONE',  ( -7.570916362186215665, 11.14999999453764090, 23.30088464923126423 ) ) ;
#12676 = CARTESIAN_POINT ( 'NONE',  ( -33.58253175000000113, 27.22500000273119269, 10.91162601494193929 ) ) ;
#12677 = VECTOR ( 'NONE', #32188, 1000.000000000000000 ) ;
#12678 = CONICAL_SURFACE ( 'NONE', #23666, 15.31642273298461276, 0.2613323016132377830 ) ;
#12679 = CARTESIAN_POINT ( 'NONE',  ( -26.07999730980477437, 35.48958333333332860, 6.988114217768305103 ) ) ;
#12680 = PRODUCT_RELATED_PRODUCT_CATEGORY ( 'part', '', ( #12 ) ) ;
#12681 = ORIENTED_EDGE ( 'NONE', *, *, #21130, .F. ) ;
#12682 = CARTESIAN_POINT ( 'NONE',  ( 33.58253175000000823, 70.02500000273121827, 10.91162601494192863 ) ) ;
#12683 = CARTESIAN_POINT ( 'NONE',  ( 2.740863092043355209E-13, 45.08593750000000711, 30.02300923189239512 ) ) ;
#12684 =( BOUNDED_CURVE ( )  B_SPLINE_CURVE ( 2, ( #32372, #10954, #21594, #965, #6298, #19352, #471, #29794, #16774, #1126, #26897, #3396, #27234 ),
 .UNSPECIFIED., .F., .T. ) 
 B_SPLINE_CURVE_WITH_KNOTS ( ( 3, 2, 2, 2, 2, 2, 3 ),
 ( 0.3500000000000000333, 0.3599999999999999867, 0.3800000000000000044, 0.4000000000000000222, 0.4199999999999999845, 0.4400000000000000022, 0.4500000000000000111 ),
 .UNSPECIFIED. ) 
 CURVE ( )  GEOMETRIC_REPRESENTATION_ITEM ( )  RATIONAL_B_SPLINE_CURVE ( ( 0.9755282581475768211, 0.9755282581475768211, 1.000000000000000000, 0.9510565162951535312, 1.000000000000000000, 0.9510565162951535312, 1.000000000000000000, 0.9510565162951535312, 1.000000000000000000, 0.9510565162951535312, 1.000000000000000000, 0.9755282581475768211, 0.9755282581475768211 ) ) 
 REPRESENTATION_ITEM ( '' )  );
#12685 = DIRECTION ( 'NONE',  ( 0.000000000000000000, 0.000000000000000000, -1.000000000000000000 ) ) ;
#12686 = ORIENTED_EDGE ( 'NONE', *, *, #30831, .T. ) ;
#12687 = CARTESIAN_POINT ( 'NONE',  ( -20.47846945139902175, 61.56288166759063074, -20.53372385742072481 ) ) ;
#12688 = CARTESIAN_POINT ( 'NONE',  ( 26.09010956794232428, 62.70871500092398065, -6.950374756619718042 ) ) ;
#12689 = CARTESIAN_POINT ( 'NONE',  ( -33.58253175000000113, 9.225000002731190918, 10.91162601494193929 ) ) ;
#12690 = CARTESIAN_POINT ( 'NONE',  ( 20.53372385742108008, 19.15586833240934794, 20.47846945139866648 ) ) ;
#12691 = FACE_BOUND ( 'NONE', #28503, .T. ) ;
#12692 = CARTESIAN_POINT ( 'NONE',  ( 33.58253175000000823, 36.27500000273119696, 10.91162601494192863 ) ) ;
#12693 = CARTESIAN_POINT ( 'NONE',  ( 10.04305231718579705, 43.10000000546237686, 30.90933677959248982 ) ) ;
#12694 = CARTESIAN_POINT ( 'NONE',  ( -9.657523855033125146E-16, 79.49999999999998579, -15.77193336357400710 ) ) ;
#12695 = CARTESIAN_POINT ( 'NONE',  ( -20.50609665441004736, 63.56249999999999289, -20.50609665440969565 ) ) ;
#12696 = CARTESIAN_POINT ( 'NONE',  ( -10.37757302488624411, 22.72500000273119980, -31.93888565452638417 ) ) ;
#12697 = CARTESIAN_POINT ( 'NONE',  ( -20.08610463437157989, 52.20000000546236407, -27.64615127144129758 ) ) ;
#12698 = CARTESIAN_POINT ( 'NONE',  ( -27.16883889988623935, 49.57500000273118701, 19.73931689729374739 ) ) ;
#12699 = CARTESIAN_POINT ( 'NONE',  ( -32.50000000000000000, 32.00000000000001421, 0.000000000000000000 ) ) ;
#12700 = CARTESIAN_POINT ( 'NONE',  ( -10.04305231718579172, 29.60000000000001563, -30.90933677959248982 ) ) ;
#12701 = CARTESIAN_POINT ( 'NONE',  ( -18.94512977948575738, 17.42499999726882010, -13.76444248337723231 ) ) ;
#12702 = CARTESIAN_POINT ( 'NONE',  ( 33.58253175000000113, 70.12500000273119838, -4.112674001490185761E-15 ) ) ;
#12703 = CARTESIAN_POINT ( 'NONE',  ( -32.50000000000000000, 70.50000000546238255, 0.000000000000000000 ) ) ;
#12704 = CARTESIAN_POINT ( 'NONE',  ( 11.25946833292375793, 74.17500000273119554, 8.180482586598731842 ) ) ;
#12705 = CARTESIAN_POINT ( 'NONE',  ( -33.58253175000000113, 61.27500000273118985, -10.91162601494193041 ) ) ;
#12706 = CARTESIAN_POINT ( 'NONE',  ( -12.13525491562421088, 72.05000000546240813, -8.816778784387096835 ) ) ;
#12707 = DIRECTION ( 'NONE',  ( -1.224646799147353454E-16, 1.000000000000000000, -0.000000000000000000 ) ) ;
#12708 = CARTESIAN_POINT ( 'NONE',  ( -20.75514604977248112, 9.425000002731202642, 28.56700777964554661 ) ) ;
#12709 = CARTESIAN_POINT ( 'NONE',  ( 24.50000000000000355, 11.84999999453761710, -7.960532557706203605 ) ) ;
#12710 = CARTESIAN_POINT ( 'NONE',  ( -27.95245687107223986, 23.32069416759064140, -0.04044903254993292840 ) ) ;
#12711 = CARTESIAN_POINT ( 'NONE',  ( 3.880418787951153803, 7.301254276084462091, 24.49999999999999645 ) ) ;
#12712 = CARTESIAN_POINT ( 'NONE',  ( -20.75514604977248823, 40.82500000273120122, -28.56700777964554305 ) ) ;
#12713 = CARTESIAN_POINT ( 'NONE',  ( -1.778240108872766143E-15, 64.00000000546238255, -32.49999999999999289 ) ) ;
#12714 = DIRECTION ( 'NONE',  ( -1.224646799147353207E-16, -1.499759782661857882E-32, 1.000000000000000000 ) ) ;
#12715 = CARTESIAN_POINT ( 'NONE',  ( -25.98046417659859486, 44.23215250092398065, -15.04653450569291628 ) ) ;
#12716 = DIRECTION ( 'NONE',  ( 0.8660254037844387076, 0.000000000000000000, -0.4999999999999998890 ) ) ;
#12717 = CARTESIAN_POINT ( 'NONE',  ( -7.543491769121917656, 41.78607666574268364, -28.00173670424536354 ) ) ;
#12718 = CARTESIAN_POINT ( 'NONE',  ( -2.092463501923844636E-15, 64.00000000546236834, -34.17252228774368916 ) ) ;
#12719 = CARTESIAN_POINT ( 'NONE',  ( 11.25946833292375793, 74.57500000273120122, -8.180482586598735395 ) ) ;
#12720 = CARTESIAN_POINT ( 'NONE',  ( 10.04305231718579705, 62.59999999999998721, 30.90933677959248982 ) ) ;
#12721 = CARTESIAN_POINT ( 'NONE',  ( -24.18731323226221974, 61.40847249907603356, 14.01125832528330406 ) ) ;
#12722 = CARTESIAN_POINT ( 'NONE',  ( 0.000000000000000000, 111.9999999999999858, 13.32050807568876927 ) ) ;
#12723 = CARTESIAN_POINT ( 'NONE',  ( -32.50000000000000000, 76.50000000546236834, 0.000000000000000000 ) ) ;
#12724 = FACE_OUTER_BOUND ( 'NONE', #25806, .T. ) ;
#12725 = EDGE_CURVE ( 'NONE', #22684, #27368, #29196, .T. ) ;
#12726 = CARTESIAN_POINT ( 'NONE',  ( -10.37757302488624411, 34.97500000273119980, -31.93888565452638417 ) ) ;
#12727 = CARTESIAN_POINT ( 'NONE',  ( -14.47279130897152299, 8.424999997268816543, 19.92008829642072243 ) ) ;
#12728 = ORIENTED_EDGE ( 'NONE', *, *, #18928, .T. ) ;
#12729 = CARTESIAN_POINT ( 'NONE',  ( -33.58253175000000113, 73.27500000273118985, -10.91162601494193218 ) ) ;
#12730 = CARTESIAN_POINT ( 'NONE',  ( -2.092463501923844636E-15, 24.00000000546238610, -34.17252228774368916 ) ) ;
#12731 = CARTESIAN_POINT ( 'NONE',  ( -28.01184896238290278, 42.36458333333332860, 7.505752307973363457 ) ) ;
#12732 = CARTESIAN_POINT ( 'NONE',  ( -26.00068869287368756, 59.98177083333332149, -15.01150461594595775 ) ) ;
#12733 = CARTESIAN_POINT ( 'NONE',  ( 20.75514604977249178, 54.07500000273118701, 28.56700777964553950 ) ) ;
#12734 = CARTESIAN_POINT ( 'NONE',  ( 10.04305231718578817, 61.90000000546235981, -30.90933677959249337 ) ) ;
#12735 = ORIENTED_EDGE ( 'NONE', *, *, #21542, .F. ) ;
#12736 = CARTESIAN_POINT ( 'NONE',  ( 3.880418787951134707, 5.301254276084476302, 24.50000000000000000 ) ) ;
#12737 = CARTESIAN_POINT ( 'NONE',  ( -27.16883889988623935, 45.32500000273117990, 19.73931689729374739 ) ) ;
#12738 = CARTESIAN_POINT ( 'NONE',  ( 18.94512977948575738, 18.42499999726882010, 13.76444248337723408 ) ) ;
#12739 = CARTESIAN_POINT ( 'NONE',  ( 10.37757302488624767, 65.97500000273120691, 31.93888565452638417 ) ) ;
#12740 = CARTESIAN_POINT ( 'NONE',  ( -20.08610463437156923, 4.800000005462381480, 27.64615127144130113 ) ) ;
#12741 = CARTESIAN_POINT ( 'NONE',  ( 20.75514604977248467, 58.42500000273119554, -28.56700777964554305 ) ) ;
#12742 = CARTESIAN_POINT ( 'NONE',  ( 3.000384657911015469E-15, 70.00000000000000000, -24.50000000000000000 ) ) ;
#12743 = CARTESIAN_POINT ( 'NONE',  ( -26.29305231718579350, 45.80000000000000426, -19.10302069950537884 ) ) ;
#12744 = FACE_OUTER_BOUND ( 'NONE', #22097, .T. ) ;
#12745 = CARTESIAN_POINT ( 'NONE',  ( 33.58253175000000113, 12.47500000273119447, -10.91162601494193751 ) ) ;
#12746 = AXIS2_PLACEMENT_3D ( 'NONE', #30214, #4145, #7053 ) ;
#12747 = CARTESIAN_POINT ( 'NONE',  ( -15.14183272437242067, 6.699999999999991296, -20.84094480462497856 ) ) ;
#12748 = CARTESIAN_POINT ( 'NONE',  ( 14.01125832528330051, 22.73659749907601935, 24.18731323226221974 ) ) ;
#12749 = CARTESIAN_POINT ( 'NONE',  ( -11.25946833292375793, 79.57500000273121543, 8.180482586598737171 ) ) ;
#12750 = CARTESIAN_POINT ( 'NONE',  ( -20.75514604977248823, 77.07500000273118701, -28.56700777964554305 ) ) ;
#12751 = CARTESIAN_POINT ( 'NONE',  ( 25.33181144634140836, 52.00000000000002842, 22.15645287102023175 ) ) ;
#12752 = AXIS2_PLACEMENT_3D ( 'NONE', #4539, #1608, #15012 ) ;
#12753 = CARTESIAN_POINT ( 'NONE',  ( 20.75514604977249178, 72.07500000273120122, 28.56700777964553950 ) ) ;
#12754 = ORIENTED_EDGE ( 'NONE', *, *, #15316, .T. ) ;
#12755 = CARTESIAN_POINT ( 'NONE',  ( 18.94512977948576093, 11.32499999726882578, -13.76444248337722875 ) ) ;
#12756 = CARTESIAN_POINT ( 'NONE',  ( -4.523095164977117273E-15, 6.124999997268802510, 24.62258325217400312 ) ) ;
#12757 = CARTESIAN_POINT ( 'NONE',  ( 27.95245687107222921, 54.53906249999998579, -2.463307335887066074E-13 ) ) ;
#12758 = CARTESIAN_POINT ( 'NONE',  ( 20.75514604977248467, 58.42500000273119554, -28.56700777964554305 ) ) ;
#12759 = CARTESIAN_POINT ( 'NONE',  ( -33.58253175000000113, 19.47500000273117493, 10.91162601494193929 ) ) ;
#12760 = CARTESIAN_POINT ( 'NONE',  ( 27.16883889988624290, 10.17500000273117955, 19.73931689729373673 ) ) ;
#12761 = CARTESIAN_POINT ( 'NONE',  ( -13.97622843553588901, 31.62239583333333215, 24.20753774853756823 ) ) ;
#12762 = CARTESIAN_POINT ( 'NONE',  ( 30.02300923189239867, 18.16444416759064140, 0.04044903254992252006 ) ) ;
#12763 = CARTESIAN_POINT ( 'NONE',  ( -7.505752307972844761, 65.85416666666665719, 28.01184896238304134 ) ) ;
#12764 = CARTESIAN_POINT ( 'NONE',  ( -10.37757302488623701, 3.525000002731190740, 31.93888565452638417 ) ) ;
#12765 = CARTESIAN_POINT ( 'NONE',  ( -1.778240108872766143E-15, 53.50000000000000000, -32.49999999999999289 ) ) ;
#12766 = CARTESIAN_POINT ( 'NONE',  ( -32.50000000000000000, 44.10000000000000142, 10.55989012756946366 ) ) ;
#12767 = CARTESIAN_POINT ( 'NONE',  ( 6.486482029760648627E-15, 45.62500000273119127, 35.31076352940722529 ) ) ;
#12768 = CARTESIAN_POINT ( 'NONE',  ( -18.94512977948575738, 11.42499999726881477, -13.76444248337723231 ) ) ;
#12769 = CARTESIAN_POINT ( 'NONE',  ( 5.779280353836490358E-15, 21.00000000546237544, 32.49999999999999289 ) ) ;
#12770 = VERTEX_POINT ( 'NONE', #3099 ) ;
#12771 = CARTESIAN_POINT ( 'NONE',  ( -20.75514604977248112, 51.67500000273117422, 28.56700777964554661 ) ) ;
#12772 = CARTESIAN_POINT ( 'NONE',  ( 32.50000000000000000, 59.50000000546238965, -3.980102097228898626E-15 ) ) ;
#12773 = CARTESIAN_POINT ( 'NONE',  ( 19.11951029504763611, 41.79725666759063785, -19.06425588902591173 ) ) ;
#12774 = CARTESIAN_POINT ( 'NONE',  ( -27.16883889988624290, 73.17500000273119554, -19.73931689729374028 ) ) ;
#12775 = ORIENTED_EDGE ( 'NONE', *, *, #32213, .T. ) ;
#12776 = CARTESIAN_POINT ( 'NONE',  ( -27.16883889988624290, 26.92500000273119554, -19.73931689729374028 ) ) ;
#12777 = AXIS2_PLACEMENT_3D ( 'NONE', #25952, #4499, #9822 ) ;
#12778 = CARTESIAN_POINT ( 'NONE',  ( -20.50609665441004736, 18.87499999999999645, -20.50609665440969565 ) ) ;
#12779 = ORIENTED_EDGE ( 'NONE', *, *, #22119, .F. ) ;
#12780 = CARTESIAN_POINT ( 'NONE',  ( 26.29305231718579350, 29.30000000546237260, 19.10302069950537529 ) ) ;
#12781 = CARTESIAN_POINT ( 'NONE',  ( -27.16883889988623935, 61.32500000273119412, 19.73931689729374739 ) ) ;
#12782 = CARTESIAN_POINT ( 'NONE',  ( 7.505752307973351023, 38.06770833333332860, 28.01184896238290278 ) ) ;
#12783 = CARTESIAN_POINT ( 'NONE',  ( -7.570916362186215665, 17.39999999999999858, 23.30088464923126423 ) ) ;
#12784 = CARTESIAN_POINT ( 'NONE',  ( 23.41746824999999887, 3.124999997268812280, 0.000000000000000000 ) ) ;
#12785 = CARTESIAN_POINT ( 'NONE',  ( 27.16883889988623935, 6.325000002731173687, -19.73931689729374384 ) ) ;
#12786 = CARTESIAN_POINT ( 'NONE',  ( -24.50000000000000000, 6.649999994537635573, -7.960532557706207157 ) ) ;
#12787 = CARTESIAN_POINT ( 'NONE',  ( 7.468012846824281681, 52.38503499907601224, -28.02196122052058058 ) ) ;
#12788 = CARTESIAN_POINT ( 'NONE',  ( -15.00000000000000000, 74.10000000000002274, 4.873795443493597723 ) ) ;
#12789 = CARTESIAN_POINT ( 'NONE',  ( 0.000000000000000000, 80.00000000000001421, 0.000000000000000000 ) ) ;
#12790 = FACE_OUTER_BOUND ( 'NONE', #25212, .T. ) ;
#12791 = CARTESIAN_POINT ( 'NONE',  ( -26.29305231718579350, 15.79999999999999538, -19.10302069950537884 ) ) ;
#12792 = CARTESIAN_POINT ( 'NONE',  ( -19.82091636218621389, 10.94999999453763451, 14.40073868116558842 ) ) ;
#12793 = CARTESIAN_POINT ( 'NONE',  ( -8.601468415847518756, 80.57500000273118701, -11.83890561707634781 ) ) ;
#12794 = CARTESIAN_POINT ( 'NONE',  ( 26.07999730980490227, 23.74479166666666430, 6.988114217767821046 ) ) ;
#12795 = EDGE_CURVE ( 'NONE', #6130, #18703, #23866, .T. ) ;
#12796 = CARTESIAN_POINT ( 'NONE',  ( 27.16883889988623935, 34.32500000273120122, -19.73931689729374384 ) ) ;
#12797 = CARTESIAN_POINT ( 'NONE',  ( -13.91746824999999532, 70.97500000273119269, 4.522059556121122093 ) ) ;
#12798 = CARTESIAN_POINT ( 'NONE',  ( -20.75514604977248112, 35.67500000273118843, 28.56700777964554661 ) ) ;
#12799 = CARTESIAN_POINT ( 'NONE',  ( 20.75514604977249178, 20.07500000273118701, 28.56700777964553950 ) ) ;
#12800 = EDGE_CURVE ( 'NONE', #2261, #25651, #633, .T. ) ;
#12801 = AXIS2_PLACEMENT_3D ( 'NONE', #11403, #8658, #21880 ) ;
#12802 = CARTESIAN_POINT ( 'NONE',  ( -20.75514604977248823, 78.82500000273120122, -28.56700777964554305 ) ) ;
#12803 = CARTESIAN_POINT ( 'NONE',  ( -10.58590195883389207, 74.00000000000001421, -10.62726115788808201 ) ) ;
#12804 = CARTESIAN_POINT ( 'NONE',  ( 20.08610463437157279, 59.30000000000001847, -27.64615127144129758 ) ) ;
#12805 = CARTESIAN_POINT ( 'NONE',  ( -23.41746824999999887, 15.62499999726882294, -2.867812753649727150E-15 ) ) ;
#12806 = CARTESIAN_POINT ( 'NONE',  ( -10.37757302488623701, 63.52500000273120406, 31.93888565452638417 ) ) ;
#12807 = CARTESIAN_POINT ( 'NONE',  ( 23.41746825000000243, 9.024999997268826846, 7.608796670333735079 ) ) ;
#12808 = CARTESIAN_POINT ( 'NONE',  ( -2.162160676586881955E-15, 70.87500000273118417, -35.31076352940723240 ) ) ;
#12809 = CARTESIAN_POINT ( 'NONE',  ( -33.58253175000000113, 7.125000002731196602, 0.000000000000000000 ) ) ;
#12810 = CARTESIAN_POINT ( 'NONE',  ( 18.94512977948576093, 17.32499999726880446, -13.76444248337722875 ) ) ;
#12811 = CARTESIAN_POINT ( 'NONE',  ( 6.950374756619721595, 18.88059000092397355, 26.09010956794232428 ) ) ;
#12812 = VERTEX_POINT ( 'NONE', #33075 ) ;
#12813 = CARTESIAN_POINT ( 'NONE',  ( -27.16883889988624290, 42.92500000273118133, -19.73931689729374028 ) ) ;
#12814 = ORIENTED_EDGE ( 'NONE', *, *, #755, .F. ) ;
#12815 = CARTESIAN_POINT ( 'NONE',  ( 28.01184896238304134, 44.36979166666666430, 7.505752307972846538 ) ) ;
#12816 = CARTESIAN_POINT ( 'NONE',  ( 3.980102097228898626E-15, 80.00000000000001421, 32.50000000000000000 ) ) ;
#12817 = CARTESIAN_POINT ( 'NONE',  ( 26.29305231718578995, 3.700000005462375618, -19.10302069950538240 ) ) ;
#12818 = CARTESIAN_POINT ( 'NONE',  ( -10.37757302488624411, 78.72500000273119269, -31.93888565452638417 ) ) ;
#12819 = CIRCLE ( 'NONE', #750, 24.50000000000000000 ) ;
#12820 = CARTESIAN_POINT ( 'NONE',  ( -14.47279130897152122, 2.424999997268802332, 19.92008829642072243 ) ) ;
#12821 = AXIS2_PLACEMENT_3D ( 'NONE', #4680, #12229, #2104 ) ;
#12822 = CARTESIAN_POINT ( 'NONE',  ( 1.507698388325705758E-15, 15.12499999726880873, -24.62258325217400312 ) ) ;
#12823 = CARTESIAN_POINT ( 'NONE',  ( 33.58253175000000823, 16.27500000273118630, 10.91162601494192863 ) ) ;
#12824 = CARTESIAN_POINT ( 'NONE',  ( -26.29305231718578995, 18.70000000546237473, 19.10302069950538595 ) ) ;
#12825 = CARTESIAN_POINT ( 'NONE',  ( -32.50000000000000000, 65.89999999999997726, -10.55989012756945478 ) ) ;
#12826 = CARTESIAN_POINT ( 'NONE',  ( 3.880418787951134707, 11.30125427608447097, 24.50000000000000000 ) ) ;
#12827 = CARTESIAN_POINT ( 'NONE',  ( 5.779280353836490358E-15, 29.00000000546237544, 32.49999999999999289 ) ) ;
#12828 = CARTESIAN_POINT ( 'NONE',  ( -20.53372385742071771, 64.14100666759063074, 20.47846945139902530 ) ) ;
#12829 = CARTESIAN_POINT ( 'NONE',  ( -26.29305231718579350, 32.30000000546237260, -19.10302069950537884 ) ) ;
#12830 = CARTESIAN_POINT ( 'NONE',  ( 28.01184896238304134, 40.93229166666666430, 7.505752307972846538 ) ) ;
#12831 = APPLICATION_PROTOCOL_DEFINITION ( 'draft international standard', 'automotive_design', 1998, #869 ) ;
#12832 = CARTESIAN_POINT ( 'NONE',  ( -18.94512977948575738, 17.92499999726882010, -13.76444248337723231 ) ) ;
#12833 = CARTESIAN_POINT ( 'NONE',  ( 26.29305231718578995, 7.199999999999984190, -19.10302069950538240 ) ) ;
#12834 = FACE_OUTER_BOUND ( 'NONE', #26978, .T. ) ;
#12835 = EDGE_CURVE ( 'NONE', #19940, #5896, #6362, .T. ) ;
#12836 = CARTESIAN_POINT ( 'NONE',  ( 14.01125832528330051, 50.23659749907603356, 24.18731323226221974 ) ) ;
#12837 = CARTESIAN_POINT ( 'NONE',  ( -33.58253175000000113, 49.12500000273117706, 0.000000000000000000 ) ) ;
#12838 = CARTESIAN_POINT ( 'NONE',  ( 33.58253175000000823, 62.27500000273118275, 10.91162601494192863 ) ) ;
#12839 = CARTESIAN_POINT ( 'NONE',  ( -33.58253175000000113, 39.37500000273119838, 0.000000000000000000 ) ) ;
#12840 = DIRECTION ( 'NONE',  ( -1.000000000000000000, -1.224646799147353454E-16, 0.000000000000000000 ) ) ;
#12841 = EDGE_CURVE ( 'NONE', #19251, #19356, #19881, .T. ) ;
#12842 = CARTESIAN_POINT ( 'NONE',  ( -15.31593959127081028, -56.96472381958990638, 0.000000000000000000 ) ) ;
#12843 = DIRECTION ( 'NONE',  ( -0.000000000000000000, -1.000000000000000000, -0.000000000000000000 ) ) ;
#12844 = CARTESIAN_POINT ( 'NONE',  ( -32.50000000000000000, 80.00000000000000000, 0.000000000000000000 ) ) ;
#12845 = CARTESIAN_POINT ( 'NONE',  ( 10.37757302488624056, 18.52500000273120406, -31.93888565452638417 ) ) ;
#12846 = DIRECTION ( 'NONE',  ( -0.000000000000000000, 1.000000000000000000, -0.000000000000000000 ) ) ;
#12847 = DIRECTION ( 'NONE',  ( -0.000000000000000000, -1.000000000000000000, -0.000000000000000000 ) ) ;
#12848 = DIRECTION ( 'NONE',  ( 0.000000000000000000, 0.000000000000000000, 1.000000000000000000 ) ) ;
#12849 = CARTESIAN_POINT ( 'NONE',  ( 19.11951029504797006, 19.15586833240934794, 19.06425588902558133 ) ) ;
#12850 = CARTESIAN_POINT ( 'NONE',  ( -32.50000000000000000, 36.50000000546236834, 0.000000000000000000 ) ) ;
#12851 = CARTESIAN_POINT ( 'NONE',  ( -33.04126587500000056, 0.8125000040967722548, 0.000000000000000000 ) ) ;
#12852 = CARTESIAN_POINT ( 'NONE',  ( 33.58253175000000113, 26.12500000273118417, -4.112674001490185761E-15 ) ) ;
#12853 = CARTESIAN_POINT ( 'NONE',  ( 6.988114217768294445, 41.50520833333333570, 26.07999730980477437 ) ) ;
#12854 = EDGE_LOOP ( 'NONE', ( #8622, #5911, #1435, #13033 ) ) ;
#12855 = CARTESIAN_POINT ( 'NONE',  ( -10.37757302488623701, 59.52500000273118275, 31.93888565452638417 ) ) ;
#12856 = CARTESIAN_POINT ( 'NONE',  ( -2.584737979205441561E-13, 46.80468750000000000, -30.02300923189239512 ) ) ;
#12857 = ORIENTED_EDGE ( 'NONE', *, *, #27597, .F. ) ;
#12858 = CARTESIAN_POINT ( 'NONE',  ( -2.584737979205441561E-13, 19.30468749999999645, -30.02300923189239512 ) ) ;
#12859 = CARTESIAN_POINT ( 'NONE',  ( 7.468012846824777284, 15.44309000092397355, 28.02196122052045268 ) ) ;
#12860 = CARTESIAN_POINT ( 'NONE',  ( 33.58253175000000823, 14.02500000273117209, 10.91162601494192863 ) ) ;
#12861 = CARTESIAN_POINT ( 'NONE',  ( -28.02196122052058413, 20.58815999907601935, -7.468012846824272799 ) ) ;
#12862 = DIRECTION ( 'NONE',  ( 1.000000000000000000, 1.224646799147353454E-16, 0.000000000000000000 ) ) ;
#12863 = CARTESIAN_POINT ( 'NONE',  ( -27.16883889988624290, 33.17500000273118843, -19.73931689729374028 ) ) ;
#12864 = CARTESIAN_POINT ( 'NONE',  ( 32.50000000000000711, 35.40000000546237402, 10.55989012756945122 ) ) ;
#12865 = CARTESIAN_POINT ( 'NONE',  ( -4.635254915624208216, 78.39999999999996305, 14.26584774442730463 ) ) ;
#12866 = CARTESIAN_POINT ( 'NONE',  ( 4.412827539393359662E-15, -59.03347138510255832, 0.000000000000000000 ) ) ;
#12867 = CARTESIAN_POINT ( 'NONE',  ( -27.16883889988624290, 24.92500000273117777, -19.73931689729374028 ) ) ;
#12868 = CARTESIAN_POINT ( 'NONE',  ( 15.14183272437242067, 5.449999994537614967, 20.84094480462498211 ) ) ;
#12869 = CARTESIAN_POINT ( 'NONE',  ( -10.37757302488624411, 50.97500000273119980, -31.93888565452638417 ) ) ;
#12870 = SURFACE_STYLE_USAGE ( .BOTH. , #2402 ) ;
#12871 = CARTESIAN_POINT ( 'NONE',  ( 6.277390505771533514E-15, 28.50000000000000000, 34.17252228774368916 ) ) ;
#12872 = CARTESIAN_POINT ( 'NONE',  ( 20.08610463437158344, 30.69999999999999218, 27.64615127144129403 ) ) ;
#12873 = CARTESIAN_POINT ( 'NONE',  ( -15.14183272437241889, 6.699999999999991296, -20.84094480462497856 ) ) ;
#12874 = CARTESIAN_POINT ( 'NONE',  ( 6.486482029760649416E-15, 69.62500000273118417, 35.31076352940723240 ) ) ;
#12875 = CARTESIAN_POINT ( 'NONE',  ( -31.95463953835047377, 66.99999999999998579, -10.27070314127411521 ) ) ;
#12876 = CARTESIAN_POINT ( 'NONE',  ( -1.778240108872766143E-15, 20.00000000546237544, -32.49999999999999289 ) ) ;
#12877 = CARTESIAN_POINT ( 'NONE',  ( -27.16883889988624290, 61.17500000273118133, -19.73931689729374028 ) ) ;
#12878 = CARTESIAN_POINT ( 'NONE',  ( 10.04305231718579705, 7.100000005462375974, 30.90933677959248982 ) ) ;
#12879 = CARTESIAN_POINT ( 'NONE',  ( -33.58253175000000113, 13.22500000273119802, 10.91162601494193929 ) ) ;
#12880 = PRODUCT_DEFINITION_SHAPE ( 'NONE', 'NONE',  #33993 ) ;
#12881 = CARTESIAN_POINT ( 'NONE',  ( -19.11951029504763611, 33.20350666759063074, 19.06425588902592239 ) ) ;
#12882 = CARTESIAN_POINT ( 'NONE',  ( 18.68038058909793619, 66.99999999999997158, -27.25458793344660080 ) ) ;
#12883 = CARTESIAN_POINT ( 'NONE',  ( 20.75514604977249178, 33.82500000273117990, 28.56700777964553950 ) ) ;
#12884 = LINE ( 'NONE', #23360, #21547 ) ;
#12885 = DIRECTION ( 'NONE',  ( 0.000000000000000000, 0.000000000000000000, -1.000000000000000000 ) ) ;
#12886 = CARTESIAN_POINT ( 'NONE',  ( -13.91746824999999532, 74.97500000273119269, 4.522059556121122093 ) ) ;
#12887 = CARTESIAN_POINT ( 'NONE',  ( 30.02300923189239867, 49.66368083240936215, -0.04044903255044467877 ) ) ;
#12888 = CARTESIAN_POINT ( 'NONE',  ( -32.50000000000000000, 56.60000000546236976, 10.55989012756946366 ) ) ;
#12889 = VECTOR ( 'NONE', #27106, 1000.000000000000000 ) ;
#12890 = CARTESIAN_POINT ( 'NONE',  ( -11.25946833292375793, 75.17500000273119554, -8.180482586598733619 ) ) ;
#12891 = CARTESIAN_POINT ( 'NONE',  ( 0.000000000000000000, 16.99999999999998579, 0.000000000000000000 ) ) ;
#12892 = CARTESIAN_POINT ( 'NONE',  ( -24.20753774853730889, 18.15885416666666075, 13.97622843553633842 ) ) ;
#12893 = DIRECTION ( 'NONE',  ( 0.000000000000000000, -0.9659258262890680902, 0.2588190451025213501 ) ) ;
#12894 = CARTESIAN_POINT ( 'NONE',  ( -32.50000000000000000, 78.50000000546236834, 0.000000000000000000 ) ) ;
#12895 = CARTESIAN_POINT ( 'NONE',  ( 15.01150461594596308, 23.02864583333332149, -26.00068869287367335 ) ) ;
#12896 = CARTESIAN_POINT ( 'NONE',  ( -20.75514604977248112, 37.67500000273118133, 28.56700777964554661 ) ) ;
#12897 = CARTESIAN_POINT ( 'NONE',  ( -23.41746824999999887, 8.124999997268817609, -2.867812753649727150E-15 ) ) ;
#12898 = ORIENTED_EDGE ( 'NONE', *, *, #3757, .F. ) ;
#12899 = CARTESIAN_POINT ( 'NONE',  ( 33.58253175000000113, 76.47500000273117848, -10.91162601494193751 ) ) ;
#12900 = CARTESIAN_POINT ( 'NONE',  ( 32.50000000000000711, 21.40000000546237757, 10.55989012756945122 ) ) ;
#12901 = CARTESIAN_POINT ( 'NONE',  ( -28.01184896238290278, 45.80208333333333570, 7.505752307973363457 ) ) ;
#12902 = CARTESIAN_POINT ( 'NONE',  ( 26.00068869287340334, 57.69010416666667140, -15.01150461594642316 ) ) ;
#12903 = CARTESIAN_POINT ( 'NONE',  ( -10.37757302488624411, 52.97500000273119980, -31.93888565452638417 ) ) ;
#12904 = CARTESIAN_POINT ( 'NONE',  ( -32.50000000000000000, 54.50000000546237544, 0.000000000000000000 ) ) ;
#12905 = VECTOR ( 'NONE', #6413, 1000.000000000000000 ) ;
#12906 = CARTESIAN_POINT ( 'NONE',  ( 3.245314017740486554E-15, 0.000000000000000000, -26.50000000000000355 ) ) ;
#12907 = CARTESIAN_POINT ( 'NONE',  ( 33.58253175000000823, 40.02500000273119696, 10.91162601494192863 ) ) ;
#12908 = CARTESIAN_POINT ( 'NONE',  ( 2.445080149700053643E-15, 72.75000000546238255, 15.00000000000000000 ) ) ;
#12909 = CARTESIAN_POINT ( 'NONE',  ( -10.37757302488623701, 65.77500000273117564, 31.93888565452638417 ) ) ;
#12910 = CARTESIAN_POINT ( 'NONE',  ( -32.50000000000000000, 2.600000005462363095, 10.55989012756946366 ) ) ;
#12911 = CARTESIAN_POINT ( 'NONE',  ( 33.58253175000000113, 58.22500000273117138, -10.91162601494193574 ) ) ;
#12912 = CARTESIAN_POINT ( 'NONE',  ( 26.29305231718578995, 49.19999999999999574, -19.10302069950538240 ) ) ;
#12913 = CARTESIAN_POINT ( 'NONE',  ( -20.08610463437156923, 14.29999999999998472, 27.64615127144130113 ) ) ;
#12914 = CARTESIAN_POINT ( 'NONE',  ( -27.16883889988623935, 13.57500000273120833, 19.73931689729374739 ) ) ;
#12915 = CARTESIAN_POINT ( 'NONE',  ( -32.50000000000000000, 74.10000000000000853, 10.55989012756946366 ) ) ;
#12916 = CARTESIAN_POINT ( 'NONE',  ( -27.95245687107223986, 30.75743083240935505, 0.04044903255043252877 ) ) ;
#12917 = CARTESIAN_POINT ( 'NONE',  ( -11.25946833292375793, 79.17500000273119554, -8.180482586598733619 ) ) ;
#12918 = CARTESIAN_POINT ( 'NONE',  ( 27.16883889988623935, 76.57500000273120122, -19.73931689729374384 ) ) ;
#12919 = LINE ( 'NONE', #18592, #26993 ) ;
#12920 = CARTESIAN_POINT ( 'NONE',  ( 20.75514604977248467, 76.67500000273116711, -28.56700777964554305 ) ) ;
#12921 = ORIENTED_EDGE ( 'NONE', *, *, #22774, .F. ) ;
#12922 = CARTESIAN_POINT ( 'NONE',  ( 14.47279130897151589, 12.82499999726882400, 19.92008829642072953 ) ) ;
#12923 = CARTESIAN_POINT ( 'NONE',  ( -7.236395654485763274, 6.024999997268825958, 22.27133577429736633 ) ) ;
#12924 = CARTESIAN_POINT ( 'NONE',  ( -19.09188309203660694, 59.26562500000000000, 19.09188309203694800 ) ) ;
#12925 = CARTESIAN_POINT ( 'NONE',  ( -33.58253175000000113, 53.22500000273118559, 10.91162601494193929 ) ) ;
#12926 = CARTESIAN_POINT ( 'NONE',  ( -2.162160676586881955E-15, 18.87500000273119483, -35.31076352940723240 ) ) ;
#12927 = CARTESIAN_POINT ( 'NONE',  ( -10.37757302488624411, 2.975000002731182036, -31.93888565452638417 ) ) ;
#12928 = CARTESIAN_POINT ( 'NONE',  ( -2.428612866367529427E-13, 43.36718749999999289, -27.95245687107223276 ) ) ;
#12929 = CARTESIAN_POINT ( 'NONE',  ( 30.02300923189239867, 25.03944416759064495, 0.04044903254992252006 ) ) ;
#12930 = ADVANCED_FACE ( 'NONE', ( #32899 ), #24854, .T. ) ;
#12931 = CARTESIAN_POINT ( 'NONE',  ( -7.468012846824272799, 19.72878499907601935, 28.02196122052058413 ) ) ;
#12932 = CARTESIAN_POINT ( 'NONE',  ( 32.50000000000000000, 77.50000000546238255, -3.980102097228898626E-15 ) ) ;
#12933 = CARTESIAN_POINT ( 'NONE',  ( 23.28634348215027572, 51.99999999999997868, -23.32808161240107125 ) ) ;
#12934 = CARTESIAN_POINT ( 'NONE',  ( 33.58253175000000823, 48.02500000273120406, 10.91162601494192685 ) ) ;
#12935 = CARTESIAN_POINT ( 'NONE',  ( 1.507698388325705758E-15, 7.124999997268828267, -24.62258325217400312 ) ) ;
#12936 = EDGE_CURVE ( 'NONE', #12338, #26701, #30006, .T. ) ;
#12937 = EDGE_CURVE ( 'NONE', #19806, #28529, #4430, .T. ) ;
#12938 = DIRECTION ( 'NONE',  ( -0.000000000000000000, -1.000000000000000000, -0.000000000000000000 ) ) ;
#12939 = ORIENTED_EDGE ( 'NONE', *, *, #33702, .F. ) ;
#12940 = CARTESIAN_POINT ( 'NONE',  ( -20.75514604977248823, 53.07500000273118701, -28.56700777964554305 ) ) ;
#12941 = LINE ( 'NONE', #20847, #32148 ) ;
#12942 = CARTESIAN_POINT ( 'NONE',  ( 6.950374756619721595, 42.94309000092397355, 26.09010956794232428 ) ) ;
#12943 = CARTESIAN_POINT ( 'NONE',  ( 10.37757302488624056, 72.77500000273118985, -31.93888565452638417 ) ) ;
#12944 = ORIENTED_EDGE ( 'NONE', *, *, #1897, .F. ) ;
#12945 = CARTESIAN_POINT ( 'NONE',  ( 27.16883889988623935, 26.32500000273117635, -19.73931689729374384 ) ) ;
#12946 = EDGE_CURVE ( 'NONE', #7457, #23226, #30832, .T. ) ;
#12947 = CARTESIAN_POINT ( 'NONE',  ( -7.505752307973343918, 19.16145833333332860, -28.01184896238290989 ) ) ;
#12948 = ORIENTED_EDGE ( 'NONE', *, *, #21821, .F. ) ;
#12949 = VECTOR ( 'NONE', #13256, 1000.000000000000000 ) ;
#12950 = DIRECTION ( 'NONE',  ( -0.000000000000000000, 1.000000000000000000, -0.000000000000000000 ) ) ;
#12951 = CARTESIAN_POINT ( 'NONE',  ( -27.16883889988624290, 58.92500000273118133, -19.73931689729374028 ) ) ;
#12952 = CARTESIAN_POINT ( 'NONE',  ( 15.01150461594643204, 51.67447916666665719, 26.00068869287340334 ) ) ;
#12953 = CARTESIAN_POINT ( 'NONE',  ( 19.82091636218621034, 15.80000000000000782, 14.40073868116559730 ) ) ;
#12954 = CARTESIAN_POINT ( 'NONE',  ( 14.47279130897151767, 2.824999997268819119, 19.92008829642072953 ) ) ;
#12955 = CARTESIAN_POINT ( 'NONE',  ( -33.58253175000000113, 5.225000002731188253, 10.91162601494193929 ) ) ;
#12956 = CARTESIAN_POINT ( 'NONE',  ( 10.04305231718579705, 28.60000000000001563, 30.90933677959248982 ) ) ;
#12957 = CARTESIAN_POINT ( 'NONE',  ( -15.04653450569338524, 62.26784749907602645, -25.98046417659831775 ) ) ;
#12958 = CARTESIAN_POINT ( 'NONE',  ( 33.58253175000000823, 78.27500000273116143, 10.91162601494192863 ) ) ;
#12959 = FACE_OUTER_BOUND ( 'NONE', #16536, .T. ) ;
#12960 = CARTESIAN_POINT ( 'NONE',  ( -20.08610463437156923, 4.300000000000009592, 27.64615127144130113 ) ) ;
#12961 = CARTESIAN_POINT ( 'NONE',  ( -10.04305231718579172, 19.59999999999999076, -30.90933677959248982 ) ) ;
#12962 = CARTESIAN_POINT ( 'NONE',  ( 19.09188309203661049, 57.54687500000000000, -19.09188309203694445 ) ) ;
#12963 = CARTESIAN_POINT ( 'NONE',  ( -7.570916362186210335, 14.34999999453762065, -23.30088464923126779 ) ) ;
#12964 = CARTESIAN_POINT ( 'NONE',  ( -15.00000000000000000, 74.25000000546239676, 0.000000000000000000 ) ) ;
#12965 = CARTESIAN_POINT ( 'NONE',  ( 24.20753774853731244, 26.75260416666666430, -13.97622843553632599 ) ) ;
#12966 = CARTESIAN_POINT ( 'NONE',  ( -10.37757302488623701, 31.52500000273117564, 31.93888565452638417 ) ) ;
#12967 = CARTESIAN_POINT ( 'NONE',  ( 13.91746825000000065, 71.77500000273117564, 4.522059556121114987 ) ) ;
#12968 = CARTESIAN_POINT ( 'NONE',  ( 10.37757302488624767, 33.97500000273119269, 31.93888565452638417 ) ) ;
#12969 = CARTESIAN_POINT ( 'NONE',  ( -10.37757302488624411, 20.97500000273119625, -31.93888565452638417 ) ) ;
#12970 = CARTESIAN_POINT ( 'NONE',  ( -26.29305231718579350, 63.79999999999999716, -19.10302069950537884 ) ) ;
#12971 = CARTESIAN_POINT ( 'NONE',  ( 26.09010956794232428, 48.95871500092396644, -6.950374756619718042 ) ) ;
#12972 = CARTESIAN_POINT ( 'NONE',  ( 6.486482029760648627E-15, 75.62500000273119838, 35.31076352940722529 ) ) ;
#12973 = FACE_OUTER_BOUND ( 'NONE', #18023, .T. ) ;
#12974 = CARTESIAN_POINT ( 'NONE',  ( 10.04305231718579705, 58.60000000000000142, 30.90933677959248982 ) ) ;
#12975 = CARTESIAN_POINT ( 'NONE',  ( 7.236395654485760609, 15.02499999726880731, -22.27133577429736633 ) ) ;
#12976 = CARTESIAN_POINT ( 'NONE',  ( 10.37757302488624056, 64.52500000273120406, -31.93888565452638417 ) ) ;
#12977 = CARTESIAN_POINT ( 'NONE',  ( 7.236395654485760609, 5.524999997268825958, -22.27133577429736633 ) ) ;
#12978 = CIRCLE ( 'NONE', #13548, 2.000000000000000000 ) ;
#12979 = CARTESIAN_POINT ( 'NONE',  ( -33.58253175000000113, 71.37500000273121259, 0.000000000000000000 ) ) ;
#12980 = CARTESIAN_POINT ( 'NONE',  ( 33.58253175000000823, 8.025000002731188076, 10.91162601494192685 ) ) ;
#12981 = CARTESIAN_POINT ( 'NONE',  ( -23.41746824999999887, 16.12499999726882294, -2.867812753649727150E-15 ) ) ;
#12982 = CARTESIAN_POINT ( 'NONE',  ( 0.04044903254993986036, 17.30506916759064140, -27.95245687107223986 ) ) ;
#12983 = ORIENTED_EDGE ( 'NONE', *, *, #24210, .F. ) ;
#12984 = VECTOR ( 'NONE', #15699, 1000.000000000000000 ) ;
#12985 = CARTESIAN_POINT ( 'NONE',  ( -33.58253175000000113, 43.22500000273118559, 10.91162601494193929 ) ) ;
#12986 = ADVANCED_FACE ( 'NONE', ( #12328 ), #16595, .T. ) ;
#12987 =( BOUNDED_CURVE ( )  B_SPLINE_CURVE ( 2, ( #13850, #16758, #22075, #32520, #8521, #13685, #8851, #27217, #16431, #21413, #31856, #19501, #3710 ),
 .UNSPECIFIED., .F., .F. ) 
 B_SPLINE_CURVE_WITH_KNOTS ( ( 3, 2, 2, 2, 2, 2, 3 ),
 ( 0.3653846153846153633, 0.3666666666666666408, 0.3692307692307692513, 0.3717948717948718063, 0.3743589743589743613, 0.3769230769230769162, 0.3782051282051281937 ),
 .UNSPECIFIED. ) 
 CURVE ( )  GEOMETRIC_REPRESENTATION_ITEM ( )  RATIONAL_B_SPLINE_CURVE ( ( 0.9755282581475768211, 0.9755282581475768211, 1.000000000000000000, 0.9510565162951535312, 1.000000000000000000, 0.9510565162951535312, 1.000000000000000000, 0.9510565162951535312, 1.000000000000000000, 0.9510565162951535312, 1.000000000000000000, 0.9755282581475768211, 0.9755282581475768211 ) ) 
 REPRESENTATION_ITEM ( '' )  );
#12988 = ORIENTED_EDGE ( 'NONE', *, *, #15037, .T. ) ;
#12989 = CARTESIAN_POINT ( 'NONE',  ( 26.00068869287340334, 43.94010416666665719, -15.01150461594642316 ) ) ;
#12990 = CARTESIAN_POINT ( 'NONE',  ( -7.579748464070165821E-14, 10.49999999999999112, -24.50000000000000000 ) ) ;
#12991 = CARTESIAN_POINT ( 'NONE',  ( 26.29305231718579350, 3.300000005462377928, 19.10302069950537529 ) ) ;
#12992 = CARTESIAN_POINT ( 'NONE',  ( -4.934616302121927505E-14, 72.50000000000001421, 32.50000000000000000 ) ) ;
#12993 = CARTESIAN_POINT ( 'NONE',  ( -23.41746824999999887, 6.124999997268814944, -2.867812753649727150E-15 ) ) ;
#12994 = CARTESIAN_POINT ( 'NONE',  ( -7.236395654485757944, 17.22499999726881370, -22.27133577429736988 ) ) ;
#12995 = CARTESIAN_POINT ( 'NONE',  ( 33.58253175000000823, 14.27500000273119340, 10.91162601494192863 ) ) ;
#12996 = CARTESIAN_POINT ( 'NONE',  ( -10.04305231718578462, 56.40000000000000568, 30.90933677959249337 ) ) ;
#12997 = CARTESIAN_POINT ( 'NONE',  ( -15.14183272437242778, 5.300000000000006040, 20.84094480462497856 ) ) ;
#12998 = CARTESIAN_POINT ( 'NONE',  ( -1.778240108872766143E-15, 29.50000000000000711, -32.49999999999999289 ) ) ;
#12999 = CARTESIAN_POINT ( 'NONE',  ( -0.04044903255044120238, 31.61680583240936215, -30.02300923189239867 ) ) ;
#13000 = CARTESIAN_POINT ( 'NONE',  ( -8.960552108402742093E-16, 78.87500000273118417, -14.63369212191046387 ) ) ;
#13001 = CARTESIAN_POINT ( 'NONE',  ( 28.01184896238290278, 40.64583333333332860, -7.505752307973347470 ) ) ;
#13002 = CONTEXT_DEPENDENT_SHAPE_REPRESENTATION ( #8548, #4354 ) ;
#13003 = DIRECTION ( 'NONE',  ( 0.000000000000000000, 0.000000000000000000, -1.000000000000000000 ) ) ;
#13004 = CARTESIAN_POINT ( 'NONE',  ( 0.000000000000000000, 0.000000000000000000, 0.000000000000000000 ) ) ;
#13005 = CARTESIAN_POINT ( 'NONE',  ( -32.50000000000000000, 8.000000000000007105, 0.000000000000000000 ) ) ;
#13006 = DIRECTION ( 'NONE',  ( -1.000000000000000000, 0.000000000000000000, 0.000000000000000000 ) ) ;
#13007 = CARTESIAN_POINT ( 'NONE',  ( 13.94119854578893580, 55.96576416574269786, -24.22776226481265383 ) ) ;
#13008 = CARTESIAN_POINT ( 'NONE',  ( -33.58253175000000113, 49.22500000273119269, 10.91162601494193929 ) ) ;
#13009 = CARTESIAN_POINT ( 'NONE',  ( -33.58253175000000113, 53.37500000273119838, 0.000000000000000000 ) ) ;
#13010 = CARTESIAN_POINT ( 'NONE',  ( 10.37757302488624056, 40.77500000273118275, -31.93888565452638417 ) ) ;
#13011 = CYLINDRICAL_SURFACE ( 'NONE', #14541, 32.50000000000000000 ) ;
#13012 = AXIS2_PLACEMENT_3D ( 'NONE', #31476, #2820, #23763 ) ;
#13013 = CARTESIAN_POINT ( 'NONE',  ( 27.95245687107223276, 13.28906249999999467, -2.463307335887066074E-13 ) ) ;
#13014 = FACE_OUTER_BOUND ( 'NONE', #26156, .T. ) ;
#13015 = CARTESIAN_POINT ( 'NONE',  ( -0.5356671165000767010, 16.99999999999998224, -23.72333643937275482 ) ) ;
#13016 = CARTESIAN_POINT ( 'NONE',  ( -32.50000000000000000, 28.10000000000001208, 10.55989012756946366 ) ) ;
#13017 = CARTESIAN_POINT ( 'NONE',  ( 27.16883889988623935, 18.32500000273119767, -19.73931689729374384 ) ) ;
#13018 = CARTESIAN_POINT ( 'NONE',  ( -13.91746824999999532, 81.27500000273120406, -4.522059556121115875 ) ) ;
#13019 = CARTESIAN_POINT ( 'NONE',  ( 23.95873412499999944, 18.31249999863440792, 0.000000000000000000 ) ) ;
#13020 = CARTESIAN_POINT ( 'NONE',  ( 3.880418787951159132, 10.19874571299079236, -24.49999999999999289 ) ) ;
#13021 = CARTESIAN_POINT ( 'NONE',  ( -26.09010956794245217, 17.15065999907602290, -6.950374756619243755 ) ) ;
#13022 = CARTESIAN_POINT ( 'NONE',  ( 10.04305231718578817, 37.90000000546238113, -30.90933677959249337 ) ) ;
#13023 = CARTESIAN_POINT ( 'NONE',  ( 20.08610463437158344, 10.70000000000001172, 27.64615127144129403 ) ) ;
#13024 = CARTESIAN_POINT ( 'NONE',  ( -27.16883889988623935, 25.32500000273119056, 19.73931689729374739 ) ) ;
#13025 = CARTESIAN_POINT ( 'NONE',  ( -2.428612866367529427E-13, 46.80468750000000000, -27.95245687107222921 ) ) ;
#13026 = ORIENTED_EDGE ( 'NONE', *, *, #22774, .T. ) ;
#13027 = CARTESIAN_POINT ( 'NONE',  ( -27.16883889988624290, 60.92500000273119554, -19.73931689729374028 ) ) ;
#13028 = CARTESIAN_POINT ( 'NONE',  ( 7.505752307973351023, 48.38020833333332860, 28.01184896238290278 ) ) ;
#13029 = ADVANCED_FACE ( 'NONE', ( #33253 ), #9749, .T. ) ;
#13030 = ORIENTED_EDGE ( 'NONE', *, *, #24060, .T. ) ;
#13031 = CARTESIAN_POINT ( 'NONE',  ( -7.505752307972844761, 14.29166666666666430, 28.01184896238304134 ) ) ;
#13032 = CARTESIAN_POINT ( 'NONE',  ( -30.02300923189239867, 13.00819416759064318, -0.04044903254991731589 ) ) ;
#13033 = ORIENTED_EDGE ( 'NONE', *, *, #2129, .F. ) ;
#13034 = CARTESIAN_POINT ( 'NONE',  ( 20.75514604977249178, 5.825000002731183457, 28.56700777964553950 ) ) ;
#13035 = ADVANCED_FACE ( 'NONE', ( #29999 ), #6503, .T. ) ;
#13036 = LINE ( 'NONE', #23507, #27795 ) ;
#13037 = CARTESIAN_POINT ( 'NONE',  ( -10.37757302488623701, 35.77500000273120406, 31.93888565452638417 ) ) ;
#13038 = CARTESIAN_POINT ( 'NONE',  ( 10.04305231718579705, 39.10000000546237686, 30.90933677959248982 ) ) ;
#13039 = CARTESIAN_POINT ( 'NONE',  ( 4.635254915624209993, 79.39999999999997726, -14.26584774442730463 ) ) ;
#13040 = CARTESIAN_POINT ( 'NONE',  ( -26.29305231718578995, 48.19999999999999574, 19.10302069950538595 ) ) ;
#13041 = CARTESIAN_POINT ( 'NONE',  ( 33.58253175000000823, 20.02500000273118275, 10.91162601494192863 ) ) ;
#13042 = CARTESIAN_POINT ( 'NONE',  ( 6.486482029760649416E-15, 51.87500000273119127, 35.31076352940723240 ) ) ;
#13043 = CARTESIAN_POINT ( 'NONE',  ( 10.04305231718579705, 28.60000000000000142, 30.90933677959248982 ) ) ;
#13044 = CARTESIAN_POINT ( 'NONE',  ( -32.50000000000000000, 25.89999999999999503, -10.55989012756945478 ) ) ;
#13045 = CARTESIAN_POINT ( 'NONE',  ( -24.50000000000001066, 5.100000000000012967, 7.960532557706201828 ) ) ;
#13046 = CARTESIAN_POINT ( 'NONE',  ( 6.486482029760649416E-15, 67.62500000273119838, 35.31076352940723240 ) ) ;
#13047 = CARTESIAN_POINT ( 'NONE',  ( 15.14183272437242245, 2.049999994537635484, -20.84094480462497856 ) ) ;
#13048 = CARTESIAN_POINT ( 'NONE',  ( -5.147494310547430452, 76.94874572391552192, 32.50000000000000000 ) ) ;
#13049 = CARTESIAN_POINT ( 'NONE',  ( -2.162160676586882350E-15, 60.87500000273117706, -35.31076352940722529 ) ) ;
#13050 = DIRECTION ( 'NONE',  ( -0.000000000000000000, -1.000000000000000000, -0.000000000000000000 ) ) ;
#13051 = CARTESIAN_POINT ( 'NONE',  ( -33.58253175000000113, 15.12500000273120371, 0.000000000000000000 ) ) ;
#13052 = CARTESIAN_POINT ( 'NONE',  ( -19.06425588902591173, 34.06288166759063785, -19.11951029504763611 ) ) ;
#13053 = FACE_OUTER_BOUND ( 'NONE', #2813, .T. ) ;
#13054 = CARTESIAN_POINT ( 'NONE',  ( 33.58253175000000823, 32.02500000273118275, 10.91162601494192863 ) ) ;
#13055 = CARTESIAN_POINT ( 'NONE',  ( -32.50000000000000000, 64.50000000546239676, 0.000000000000000000 ) ) ;
#13056 = CARTESIAN_POINT ( 'NONE',  ( 3.778760231354629433E-15, 0.5000000000000067724, -24.50000000000000355 ) ) ;
#13057 = CARTESIAN_POINT ( 'NONE',  ( -11.25946833292375793, 74.67500000273119554, -8.180482586598733619 ) ) ;
#13058 = CARTESIAN_POINT ( 'NONE',  ( -28.00173670424535644, 51.23920166574269786, 7.543491769121936308 ) ) ;
#13059 = CARTESIAN_POINT ( 'NONE',  ( 20.08610463437158344, 55.20000000546238539, 27.64615127144129403 ) ) ;
#13060 = CARTESIAN_POINT ( 'NONE',  ( -8.960552108402742093E-16, 74.87500000273119838, -14.63369212191046387 ) ) ;
#13061 = CARTESIAN_POINT ( 'NONE',  ( 13.97622843553633665, 20.73697916666666075, 24.20753774853730889 ) ) ;
#13062 = CARTESIAN_POINT ( 'NONE',  ( -1.053607264507113999E-13, 63.00000000546238255, 32.50000000000000711 ) ) ;
#13063 = CARTESIAN_POINT ( 'NONE',  ( 32.50000000000000000, 67.60000000546237686, -10.55989012756945833 ) ) ;
#13064 = CARTESIAN_POINT ( 'NONE',  ( -30.02300923189239512, 18.44531249999999645, 2.654126918244515359E-13 ) ) ;
#13065 = CARTESIAN_POINT ( 'NONE',  ( 33.58253175000000823, 34.27500000273116854, 10.91162601494192863 ) ) ;
#13066 = CARTESIAN_POINT ( 'NONE',  ( -7.236395654485757944, 13.72499999726881015, -22.27133577429736988 ) ) ;
#13067 = ORIENTED_EDGE ( 'NONE', *, *, #33259, .F. ) ;
#13068 = CARTESIAN_POINT ( 'NONE',  ( -28.02196122052045268, 43.80246500092398776, 7.468012846824790607 ) ) ;
#13069 = CARTESIAN_POINT ( 'NONE',  ( -32.50000000000000000, 20.50000000546238610, 0.000000000000000000 ) ) ;
#13070 = CARTESIAN_POINT ( 'NONE',  ( -30.02300923189239512, 42.50781249999997868, 2.654126918244515359E-13 ) ) ;
#13071 = CARTESIAN_POINT ( 'NONE',  ( 20.50609665440969565, 57.54687500000000000, -20.50609665441004736 ) ) ;
#13072 = EDGE_CURVE ( 'NONE', #20157, #4399, #4531, .T. ) ;
#13073 = CARTESIAN_POINT ( 'NONE',  ( -27.16883889988624290, 57.17500000273118133, -19.73931689729374028 ) ) ;
#13074 = EDGE_CURVE ( 'NONE', #13367, #14415, #14948, .T. ) ;
#13075 = CARTESIAN_POINT ( 'NONE',  ( -26.29305231718579350, 54.30000000546236549, -19.10302069950537884 ) ) ;
#13076 = CARTESIAN_POINT ( 'NONE',  ( -15.14183272437242778, 13.04999999453763770, 20.84094480462497856 ) ) ;
#13077 = CARTESIAN_POINT ( 'NONE',  ( 27.16883889988624290, 39.92500000273119554, 19.73931689729373673 ) ) ;
#13078 = PLANE ( 'NONE',  #22531 ) ;
#13079 = CARTESIAN_POINT ( 'NONE',  ( 10.37757302488624056, 70.77500000273117564, -31.93888565452638417 ) ) ;
#13080 = CARTESIAN_POINT ( 'NONE',  ( 10.04305231718578817, 1.900000005462365582, -30.90933677959249337 ) ) ;
#13081 = CARTESIAN_POINT ( 'NONE',  ( 10.37757302488624767, 63.72500000273119269, 31.93888565452638417 ) ) ;
#13082 = CARTESIAN_POINT ( 'NONE',  ( -2.584737979205442066E-13, 19.30468749999999645, -30.02300923189239867 ) ) ;
#13083 = CARTESIAN_POINT ( 'NONE',  ( 20.08610463437158344, 46.70000000000000284, 27.64615127144129403 ) ) ;
#13084 = CARTESIAN_POINT ( 'NONE',  ( 23.41746824999999887, 4.624999997268814056, 0.000000000000000000 ) ) ;
#13085 = CARTESIAN_POINT ( 'NONE',  ( -27.16883889988624290, 13.17500000273119554, -19.73931689729374028 ) ) ;
#13086 = CARTESIAN_POINT ( 'NONE',  ( -20.08610463437156923, 66.80000000546236549, 27.64615127144130113 ) ) ;
#13087 = CARTESIAN_POINT ( 'NONE',  ( 24.18731323226221974, 35.62722249907602645, -14.01125832528328985 ) ) ;
#13088 = CARTESIAN_POINT ( 'NONE',  ( 11.25946833292375793, 78.17500000273119554, 8.180482586598731842 ) ) ;
#13089 = DIRECTION ( 'NONE',  ( -1.000000000000000000, 0.000000000000000000, 0.000000000000000000 ) ) ;
#13090 = CARTESIAN_POINT ( 'NONE',  ( 0.000000000000000000, 80.00000000000001421, 0.000000000000000000 ) ) ;
#13091 = CARTESIAN_POINT ( 'NONE',  ( -20.75514604977248112, 75.67500000273118133, 28.56700777964554661 ) ) ;
#13092 = ORIENTED_EDGE ( 'NONE', *, *, #11730, .T. ) ;
#13093 = DIRECTION ( 'NONE',  ( -0.000000000000000000, -1.000000000000000000, -0.000000000000000000 ) ) ;
#13094 = CARTESIAN_POINT ( 'NONE',  ( -24.20753774853730889, 59.40885416666666430, 13.97622843553633842 ) ) ;
#13095 =( BOUNDED_CURVE ( )  B_SPLINE_CURVE ( 2, ( #4577, #4918, #25520, #12640, #23289, #33402, #33757, #7832, #30824, #18321, #7317, #2521, #12990 ),
 .UNSPECIFIED., .F., .T. ) 
 B_SPLINE_CURVE_WITH_KNOTS ( ( 3, 2, 2, 2, 2, 2, 3 ),
 ( 0.5277777777777777901, 0.5333333333333333259, 0.5444444444444443976, 0.5555555555555555802, 0.5666666666666666519, 0.5777777777777777235, 0.5833333333333333703 ),
 .UNSPECIFIED. ) 
 CURVE ( )  GEOMETRIC_REPRESENTATION_ITEM ( )  RATIONAL_B_SPLINE_CURVE ( ( 0.9755282581475768211, 0.9755282581475768211, 1.000000000000000000, 0.9510565162951535312, 1.000000000000000000, 0.9510565162951535312, 1.000000000000000000, 0.9510565162951535312, 1.000000000000000000, 0.9510565162951535312, 1.000000000000000000, 0.9755282581475765991, 0.9755282581475768211 ) ) 
 REPRESENTATION_ITEM ( '' )  );
#13096 = CARTESIAN_POINT ( 'NONE',  ( 10.37757302488624056, 56.52500000273118275, -31.93888565452638417 ) ) ;
#13097 = CARTESIAN_POINT ( 'NONE',  ( 10.37757302488624767, 17.97500000273118204, 31.93888565452638417 ) ) ;
#13098 = CARTESIAN_POINT ( 'NONE',  ( 27.16883889988624290, 2.175000002731186655, 19.73931689729373673 ) ) ;
#13099 = CARTESIAN_POINT ( 'NONE',  ( 6.988114217768294445, 44.94270833333332860, 26.07999730980477437 ) ) ;
#13100 = CARTESIAN_POINT ( 'NONE',  ( 7.543491769121427382, 31.19829833425730570, -28.00173670424548433 ) ) ;
#13101 = CARTESIAN_POINT ( 'NONE',  ( -15.04653450569338524, 17.58034749907602290, -25.98046417659831775 ) ) ;
#13102 = CARTESIAN_POINT ( 'NONE',  ( 32.50000000000000000, 73.60000000546240528, -10.55989012756945833 ) ) ;
#13103 = CARTESIAN_POINT ( 'NONE',  ( 9.358181289160048877, 51.99999999999999289, -31.32043657353322885 ) ) ;
#13104 = CARTESIAN_POINT ( 'NONE',  ( -33.58253175000000113, 41.12500000273119838, 0.000000000000000000 ) ) ;
#13105 = CARTESIAN_POINT ( 'NONE',  ( 26.09010956794244507, 42.93190999907601935, 6.950374756619249084 ) ) ;
#13106 = CARTESIAN_POINT ( 'NONE',  ( 7.236395654485755280, 6.224999997268803931, 22.27133577429736988 ) ) ;
#13107 = CARTESIAN_POINT ( 'NONE',  ( -20.08610463437157989, 2.200000005462376063, -27.64615127144129758 ) ) ;
#13108 = VERTEX_POINT ( 'NONE', #25878 ) ;
#13109 = CARTESIAN_POINT ( 'NONE',  ( 33.58253175000000113, 56.37500000273119838, -4.112674001490185761E-15 ) ) ;
#13110 = CARTESIAN_POINT ( 'NONE',  ( -1.778240108872766143E-15, 4.000000005462373664, -32.49999999999999289 ) ) ;
#13111 = CARTESIAN_POINT ( 'NONE',  ( -14.01125832528285109, 43.37277750092397355, 24.18731323226248264 ) ) ;
#13112 = CARTESIAN_POINT ( 'NONE',  ( -33.58253175000000113, 77.27500000273117564, -10.91162601494193218 ) ) ;
#13113 = ORIENTED_EDGE ( 'NONE', *, *, #27597, .T. ) ;
#13114 = CARTESIAN_POINT ( 'NONE',  ( -33.58253175000000113, 27.12500000273120193, 0.000000000000000000 ) ) ;
#13115 = CARTESIAN_POINT ( 'NONE',  ( 20.50609665441005092, 17.15624999999999645, 20.50609665440969209 ) ) ;
#13116 = ORIENTED_EDGE ( 'NONE', *, *, #23213, .F. ) ;
#13117 = CARTESIAN_POINT ( 'NONE',  ( -32.50000000000000000, 58.10000000000000142, 10.55989012756946366 ) ) ;
#13118 = CARTESIAN_POINT ( 'NONE',  ( -33.58253175000000113, 61.12500000273119127, 0.000000000000000000 ) ) ;
#13119 = CARTESIAN_POINT ( 'NONE',  ( 28.01184896238290278, 50.95833333333332860, -7.505752307973347470 ) ) ;
#13120 = CARTESIAN_POINT ( 'NONE',  ( -14.47279130897151767, 11.82499999726882578, -19.92008829642072598 ) ) ;
#13121 = CARTESIAN_POINT ( 'NONE',  ( 10.37757302488624056, 2.525000002731203619, -31.93888565452638417 ) ) ;
#13122 = PRESENTATION_STYLE_ASSIGNMENT (( #18629 ) ) ;
#13123 = CARTESIAN_POINT ( 'NONE',  ( -28.02196122052058413, 61.83815999907601935, -7.468012846824272799 ) ) ;
#13124 = CARTESIAN_POINT ( 'NONE',  ( 5.779280353836490358E-15, 61.00000000546238255, 32.49999999999999289 ) ) ;
#13125 = CARTESIAN_POINT ( 'NONE',  ( -30.02300923189239867, 63.13281249999999289, 2.654126918244514854E-13 ) ) ;
#13126 = CARTESIAN_POINT ( 'NONE',  ( -10.04305231718579172, 59.60000000000000142, -30.90933677959248982 ) ) ;
#13127 = CARTESIAN_POINT ( 'NONE',  ( -20.08610463437157989, 13.70000000000000462, -27.64615127144129758 ) ) ;
#13128 = CARTESIAN_POINT ( 'NONE',  ( 27.95245687107223276, 64.85156249999997158, -2.463307335887066074E-13 ) ) ;
#13129 = CARTESIAN_POINT ( 'NONE',  ( -15.14183272437241889, 12.44999999453762918, -20.84094480462497856 ) ) ;
#13130 = CARTESIAN_POINT ( 'NONE',  ( 4.300734207923761154, 79.47500000273119269, 13.23629886949340495 ) ) ;
#13131 = CARTESIAN_POINT ( 'NONE',  ( -6.988114217768288228, 36.34895833333333570, -26.07999730980477437 ) ) ;
#13132 = CARTESIAN_POINT ( 'NONE',  ( 33.58253175000000823, 30.02500000273118985, 10.91162601494192863 ) ) ;
#13133 = CARTESIAN_POINT ( 'NONE',  ( 33.58253175000000113, 70.22500000273120691, -10.91162601494193751 ) ) ;
#13134 = CARTESIAN_POINT ( 'NONE',  ( -20.75514604977248823, 35.07500000273120833, -28.56700777964554305 ) ) ;
#13135 = CARTESIAN_POINT ( 'NONE',  ( -10.37757302488623701, 15.77500000273118808, 31.93888565452638417 ) ) ;
#13136 = CARTESIAN_POINT ( 'NONE',  ( -3.880418787951124493, 7.448745718453147369, 24.50000000000000355 ) ) ;
#13137 = CARTESIAN_POINT ( 'NONE',  ( 19.06425588902592239, 56.40663166759065206, 19.11951029504763611 ) ) ;
#13138 = EDGE_CURVE ( 'NONE', #22725, #15526, #23013, .T. ) ;
#13139 = CARTESIAN_POINT ( 'NONE',  ( -27.16883889988623935, 77.32500000273118701, 19.73931689729374739 ) ) ;
#13140 = CARTESIAN_POINT ( 'NONE',  ( 19.82091636218621034, 7.800000000000001599, 14.40073868116559730 ) ) ;
#13141 = CARTESIAN_POINT ( 'NONE',  ( -2.092463501923844636E-15, 55.49999999999999289, -34.17252228774368916 ) ) ;
#13142 = CARTESIAN_POINT ( 'NONE',  ( 18.94512977948575738, 16.42499999726882010, 13.76444248337723408 ) ) ;
#13143 = CARTESIAN_POINT ( 'NONE',  ( 33.58253175000000113, 64.12500000273119838, -4.112674001490185761E-15 ) ) ;
#13144 = CARTESIAN_POINT ( 'NONE',  ( 14.47279130897151767, 7.424999997268820096, -19.92008829642072598 ) ) ;
#13145 = ORIENTED_EDGE ( 'NONE', *, *, #17449, .F. ) ;
#13146 = CARTESIAN_POINT ( 'NONE',  ( -20.75514604977248112, 73.67500000273120975, 28.56700777964554661 ) ) ;
#13147 = CARTESIAN_POINT ( 'NONE',  ( -20.75514604977248823, 4.825000002731171911, -28.56700777964554305 ) ) ;
#13148 = CARTESIAN_POINT ( 'NONE',  ( -18.94512977948575738, 15.92499999726881832, -13.76444248337723231 ) ) ;
#13149 = CARTESIAN_POINT ( 'NONE',  ( 14.01125832528286352, 14.15402750092397532, -24.18731323226246843 ) ) ;
#13150 = ORIENTED_EDGE ( 'NONE', *, *, #18466, .T. ) ;
#13151 = CARTESIAN_POINT ( 'NONE',  ( -27.16883889988624290, 40.92500000273118133, -19.73931689729374028 ) ) ;
#13152 = EDGE_LOOP ( 'NONE', ( #13150, #12775, #19991, #8207, #24047, #10287 ) ) ;
#13153 = CARTESIAN_POINT ( 'NONE',  ( -28.01184896238304134, 42.65104166666666430, -7.505752307972844761 ) ) ;
#13154 = CARTESIAN_POINT ( 'NONE',  ( 5.147494310547434893, 11.05125428700922896, 32.49999999999999289 ) ) ;
#13155 = CARTESIAN_POINT ( 'NONE',  ( -26.29305231718578995, 6.700000005462378283, 19.10302069950538595 ) ) ;
#13156 = LINE ( 'NONE', #31514, #32608 ) ;
#13157 = CARTESIAN_POINT ( 'NONE',  ( 26.00068869287340334, 23.31510416666666430, -15.01150461594642316 ) ) ;
#13158 = CARTESIAN_POINT ( 'NONE',  ( 15.14183272437242245, 2.299999999999985612, -20.84094480462497856 ) ) ;
#13159 = CARTESIAN_POINT ( 'NONE',  ( 33.58253175000000113, 16.47500000273118204, -10.91162601494193751 ) ) ;
#13160 = CARTESIAN_POINT ( 'NONE',  ( -20.08610463437156923, 62.29999999999997584, 27.64615127144130113 ) ) ;
#13161 = CARTESIAN_POINT ( 'NONE',  ( -4.300734207923755825, 79.27500000273118985, 13.23629886949340673 ) ) ;
#13162 = CARTESIAN_POINT ( 'NONE',  ( -5.147494310547423346, 30.44874571845313938, 32.50000000000000000 ) ) ;
#13163 = CARTESIAN_POINT ( 'NONE',  ( 14.97647472619900455, 31.90326416574268364, -26.02091320914876960 ) ) ;
#13164 = CARTESIAN_POINT ( 'NONE',  ( 11.25946833292375793, 78.57500000273121543, -8.180482586598735395 ) ) ;
#13165 = CARTESIAN_POINT ( 'NONE',  ( -15.01150461594595775, 38.49739583333332860, 26.00068869287368756 ) ) ;
#13166 = ITEM_DEFINED_TRANSFORMATION ( 'NONE', 'NONE', #5739,  #1376 ) ;
#13167 = FACE_OUTER_BOUND ( 'NONE', #15847, .T. ) ;
#13168 = CARTESIAN_POINT ( 'NONE',  ( 7.570916362186213000, 16.39999999999999858, -23.30088464923126423 ) ) ;
#13169 = CARTESIAN_POINT ( 'NONE',  ( 32.50000000000000711, 2.899999999999995470, 10.55989012756945122 ) ) ;
#13170 = CARTESIAN_POINT ( 'NONE',  ( -15.00000000000000000, 73.90000000000001990, -4.873795443493594171 ) ) ;
#13171 = CARTESIAN_POINT ( 'NONE',  ( -19.06425588902558133, 57.82774333240935505, 19.11951029504797006 ) ) ;
#13172 = CARTESIAN_POINT ( 'NONE',  ( 33.58253175000000113, 48.12500000273117706, -4.112674001490185761E-15 ) ) ;
#13173 = CARTESIAN_POINT ( 'NONE',  ( 33.58253175000000823, 56.27500000273116854, 10.91162601494192863 ) ) ;
#13174 = PRODUCT_DEFINITION_FORMATION_WITH_SPECIFIED_SOURCE ( 'ANY', '', #20871, .NOT_KNOWN. ) ;
#13175 = CARTESIAN_POINT ( 'NONE',  ( 33.58253175000000113, 36.37500000273119838, -4.112674001490185761E-15 ) ) ;
#13176 = CARTESIAN_POINT ( 'NONE',  ( 0.000000000000000000, 80.00000000000001421, 0.000000000000000000 ) ) ;
#13177 = DIRECTION ( 'NONE',  ( -1.224646799147353454E-16, 1.000000000000000000, -0.000000000000000000 ) ) ;
#13178 = DIRECTION ( 'NONE',  ( -0.000000000000000000, -1.000000000000000000, -0.000000000000000000 ) ) ;
#13179 = DIRECTION ( 'NONE',  ( 0.000000000000000000, -1.000000000000000000, 0.000000000000000000 ) ) ;
#13180 = CARTESIAN_POINT ( 'NONE',  ( -26.29305231718579350, 77.80000000000002558, -19.10302069950537884 ) ) ;
#13181 = CARTESIAN_POINT ( 'NONE',  ( -27.16883889988623935, 17.32500000273119767, 19.73931689729374739 ) ) ;
#13182 = CARTESIAN_POINT ( 'NONE',  ( -1.778240108872766143E-15, 62.00000000546238255, -32.49999999999999289 ) ) ;
#13183 = CARTESIAN_POINT ( 'NONE',  ( 0.000000000000000000, 70.00000000000000000, 0.000000000000000000 ) ) ;
#13184 = CARTESIAN_POINT ( 'NONE',  ( 24.50000000000000000, 12.00000000000001066, 0.000000000000000000 ) ) ;
#13185 = CARTESIAN_POINT ( 'NONE',  ( 14.01125832528330051, 15.86159749907602112, 24.18731323226221974 ) ) ;
#13186 = CARTESIAN_POINT ( 'NONE',  ( 32.50000000000000000, 35.60000000546236976, -10.55989012756945833 ) ) ;
#13187 =( BOUNDED_CURVE ( )  B_SPLINE_CURVE ( 2, ( #1532, #17858, #17339, #17173, #22477, #7199, #17680, #27802, #9424, #9605, #25738, #22649, #27630 ),
 .UNSPECIFIED., .F., .T. ) 
 B_SPLINE_CURVE_WITH_KNOTS ( ( 3, 2, 2, 2, 2, 2, 3 ),
 ( 0.6388888888888889506, 0.6444444444444444864, 0.6555555555555555580, 0.6666666666666666297, 0.6777777777777778123, 0.6888888888888888840, 0.6944444444444444198 ),
 .UNSPECIFIED. ) 
 CURVE ( )  GEOMETRIC_REPRESENTATION_ITEM ( )  RATIONAL_B_SPLINE_CURVE ( ( 0.9755282581475768211, 0.9755282581475770431, 1.000000000000000000, 0.9510565162951535312, 1.000000000000000000, 0.9510565162951535312, 1.000000000000000000, 0.9510565162951535312, 1.000000000000000000, 0.9510565162951535312, 1.000000000000000000, 0.9755282581475768211, 0.9755282581475768211 ) ) 
 REPRESENTATION_ITEM ( '' )  );
#13188 = CARTESIAN_POINT ( 'NONE',  ( 7.313012447739250820E-14, 17.24999999453762456, 24.50000000000000000 ) ) ;
#13189 = CARTESIAN_POINT ( 'NONE',  ( 10.37757302488624767, 25.72500000273120335, 31.93888565452638417 ) ) ;
#13190 = CARTESIAN_POINT ( 'NONE',  ( -6.988114217768288228, 46.66145833333332860, -26.07999730980477437 ) ) ;
#13191 = EDGE_LOOP ( 'NONE', ( #24396, #2203, #30254, #20076, #25128, #27704 ) ) ;
#13192 = CARTESIAN_POINT ( 'NONE',  ( -10.37757302488624411, 64.72500000273119269, -31.93888565452638417 ) ) ;
#13193 = EDGE_LOOP ( 'NONE', ( #20141, #18485, #21188, #13275 ) ) ;
#13194 = CARTESIAN_POINT ( 'NONE',  ( 15.01150461594596308, 19.59114583333332149, -26.00068869287367335 ) ) ;
#13195 = CARTESIAN_POINT ( 'NONE',  ( 26.02091320914851025, 14.44048583425730925, -14.97647472619946463 ) ) ;
#13196 = CARTESIAN_POINT ( 'NONE',  ( 27.16883889988623935, 4.325000002731186122, -19.73931689729374384 ) ) ;
#13197 = CARTESIAN_POINT ( 'NONE',  ( 1.507698388325705758E-15, 1.124999997268814722, -24.62258325217400312 ) ) ;
#13198 = CARTESIAN_POINT ( 'NONE',  ( 20.75514604977248467, 32.67500000273118843, -28.56700777964554305 ) ) ;
#13199 = CARTESIAN_POINT ( 'NONE',  ( 20.08610463437157279, 35.80000000546235128, -27.64615127144129758 ) ) ;
#13200 = CARTESIAN_POINT ( 'NONE',  ( -2.092463501923844636E-15, 77.50000000000000000, -34.17252228774368916 ) ) ;
#13201 = CARTESIAN_POINT ( 'NONE',  ( -32.50000000000000000, 47.89999999999999858, -10.55989012756945300 ) ) ;
#13202 = CARTESIAN_POINT ( 'NONE',  ( 1.093617666956751375E-13, 61.50000000000000000, -32.50000000000000711 ) ) ;
#13203 = CARTESIAN_POINT ( 'NONE',  ( 20.75514604977248467, 46.67500000273118133, -28.56700777964554305 ) ) ;
#13204 =( NAMED_UNIT ( * ) PLANE_ANGLE_UNIT ( ) SI_UNIT ( $, .RADIAN. ) );
#13205 = CARTESIAN_POINT ( 'NONE',  ( 32.50000000000000000, 21.10000000000000142, -10.55989012756945833 ) ) ;
#13206 = CARTESIAN_POINT ( 'NONE',  ( 20.08610463437158344, 24.70000000000000284, 27.64615127144129403 ) ) ;
#13207 = CARTESIAN_POINT ( 'NONE',  ( 24.50000000000000355, 8.100000000000006750, -7.960532557706203605 ) ) ;
#13208 = CARTESIAN_POINT ( 'NONE',  ( -33.58253175000000113, 69.12500000273119838, 0.000000000000000000 ) ) ;
#13209 = CARTESIAN_POINT ( 'NONE',  ( 19.82091636218621389, 1.949999994537626735, -14.40073868116559197 ) ) ;
#13210 = CARTESIAN_POINT ( 'NONE',  ( 1.425975843264271514, 74.00000000000001421, -14.45395831230864481 ) ) ;
#13211 = CARTESIAN_POINT ( 'NONE',  ( -33.58253175000000113, 63.27500000273118985, -10.91162601494193041 ) ) ;
#13212 = CARTESIAN_POINT ( 'NONE',  ( 5.147494310547426899, 39.94874572391552903, -32.50000000000000000 ) ) ;
#13213 = CARTESIAN_POINT ( 'NONE',  ( 20.75514604977248467, 10.42500000273120087, -28.56700777964554305 ) ) ;
#13214 = CARTESIAN_POINT ( 'NONE',  ( 7.025853678916403666, 27.76079833425730925, -26.06988505166735237 ) ) ;
#13215 = EDGE_CURVE ( 'NONE', #9464, #1088, #136, .T. ) ;
#13216 = CARTESIAN_POINT ( 'NONE',  ( 24.50000000000000000, 1.849999994537612658, -7.960532557706203605 ) ) ;
#13217 = CARTESIAN_POINT ( 'NONE',  ( 8.327598234202002696E-15, -91.00000000000000000, 0.000000000000000000 ) ) ;
#13218 = CARTESIAN_POINT ( 'NONE',  ( -2.162160676586881955E-15, 34.62500000273119127, -35.31076352940723240 ) ) ;
#13219 = DIRECTION ( 'NONE',  ( 0.000000000000000000, 0.000000000000000000, -1.000000000000000000 ) ) ;
#13220 = CARTESIAN_POINT ( 'NONE',  ( 26.29305231718578995, 19.19999999999999574, -19.10302069950538240 ) ) ;
#13221 = ADVANCED_FACE ( 'NONE', ( #28286 ), #20823, .T. ) ;
#13222 = CARTESIAN_POINT ( 'NONE',  ( 13.91746824999999532, 77.97500000273122112, -4.522059556121118540 ) ) ;
#13223 = CARTESIAN_POINT ( 'NONE',  ( 7.468012846824281681, 48.94753499907601935, -28.02196122052058058 ) ) ;
#13224 = CARTESIAN_POINT ( 'NONE',  ( 32.50000000000000000, 53.60000000546238397, -10.55989012756945833 ) ) ;
#13225 = CARTESIAN_POINT ( 'NONE',  ( 13.91746824999999532, 76.47500000273120691, -4.522059556121118540 ) ) ;
#13226 =( NAMED_UNIT ( * ) SI_UNIT ( $, .STERADIAN. ) SOLID_ANGLE_UNIT ( ) );
#13227 = CARTESIAN_POINT ( 'NONE',  ( -6.988114217767819270, 17.72916666666666430, 26.07999730980490583 ) ) ;
#13228 = CARTESIAN_POINT ( 'NONE',  ( 23.41746825000000243, 7.024999997268802865, 7.608796670333735079 ) ) ;
#13229 = CARTESIAN_POINT ( 'NONE',  ( 32.50000000000000000, 71.60000000546240528, -10.55989012756945833 ) ) ;
#13230 = CARTESIAN_POINT ( 'NONE',  ( -20.50609665440969209, 24.89062500000000000, 20.50609665441005092 ) ) ;
#13231 = VECTOR ( 'NONE', #28687, 1000.000000000000000 ) ;
#13232 = CARTESIAN_POINT ( 'NONE',  ( -10.37757302488624411, 28.97500000273119269, -31.93888565452638417 ) ) ;
#13233 = CARTESIAN_POINT ( 'NONE',  ( -18.94512977948576093, 12.32499999726879913, 13.76444248337722698 ) ) ;
#13234 = ORIENTED_EDGE ( 'NONE', *, *, #17536, .F. ) ;
#13235 = CARTESIAN_POINT ( 'NONE',  ( 7.543491769121427382, 44.94829833425730925, -28.00173670424548433 ) ) ;
#13236 = CARTESIAN_POINT ( 'NONE',  ( -10.04305231718579172, 18.10000000546237331, -30.90933677959248982 ) ) ;
#13237 = CARTESIAN_POINT ( 'NONE',  ( 20.50609665441005092, 48.09375000000000000, 20.50609665440969209 ) ) ;
#13238 = DIRECTION ( 'NONE',  ( -0.000000000000000000, -1.000000000000000000, -0.000000000000000000 ) ) ;
#13239 = CARTESIAN_POINT ( 'NONE',  ( -20.75514604977248823, 57.07500000273117280, -28.56700777964554305 ) ) ;
#13240 = CARTESIAN_POINT ( 'NONE',  ( 10.04305231718578817, 53.90000000546238113, -30.90933677959249337 ) ) ;
#13241 = CARTESIAN_POINT ( 'NONE',  ( -8.601468415847518756, 77.07500000273117280, -11.83890561707634781 ) ) ;
#13242 = AXIS2_PLACEMENT_3D ( 'NONE', #22366, #33337, #29910 ) ;
#13243 = CARTESIAN_POINT ( 'NONE',  ( -33.58253175000000113, 43.22500000273118559, 10.91162601494193929 ) ) ;
#13244 = CARTESIAN_POINT ( 'NONE',  ( 20.08610463437157279, 55.29999999999999716, -27.64615127144129758 ) ) ;
#13245 = VECTOR ( 'NONE', #5312, 1000.000000000000227 ) ;
#13246 = CARTESIAN_POINT ( 'NONE',  ( -10.37757302488623701, 67.77500000273117564, 31.93888565452638417 ) ) ;
#13247 = DIRECTION ( 'NONE',  ( -0.000000000000000000, -1.000000000000000000, -0.000000000000000000 ) ) ;
#13248 = CARTESIAN_POINT ( 'NONE',  ( -20.75514604977248823, 60.82500000273120122, -28.56700777964554305 ) ) ;
#13249 = CARTESIAN_POINT ( 'NONE',  ( -28.01184896238304134, 25.46354166666666430, -7.505752307972844761 ) ) ;
#13250 = CARTESIAN_POINT ( 'NONE',  ( 6.277390505771533514E-15, 48.50000000000000711, 34.17252228774368916 ) ) ;
#13251 = CARTESIAN_POINT ( 'NONE',  ( 7.236395654485760609, 3.024999997268823293, -22.27133577429736633 ) ) ;
#13252 = CARTESIAN_POINT ( 'NONE',  ( -2.162160676586881955E-15, 10.87500000273118417, -35.31076352940723240 ) ) ;
#13253 = FACE_OUTER_BOUND ( 'NONE', #11908, .T. ) ;
#13254 = CARTESIAN_POINT ( 'NONE',  ( 26.09010956794244507, 32.61940999907601224, 6.950374756619249084 ) ) ;
#13255 = CARTESIAN_POINT ( 'NONE',  ( 13.91746825000000065, 72.27500000273118985, 4.522059556121114987 ) ) ;
#13256 = DIRECTION ( 'NONE',  ( 1.000000000000000000, 0.000000000000000000, 0.000000000000000000 ) ) ;
#13257 = CARTESIAN_POINT ( 'NONE',  ( 0.000000000000000000, 86.00000000000001421, 0.000000000000000000 ) ) ;
#13258 = CARTESIAN_POINT ( 'NONE',  ( 10.37757302488624056, 74.77500000273117564, -31.93888565452638417 ) ) ;
#13259 = ORIENTED_EDGE ( 'NONE', *, *, #17767, .F. ) ;
#13260 = CARTESIAN_POINT ( 'NONE',  ( 0.000000000000000000, 70.00000000000000000, 0.000000000000000000 ) ) ;
#13261 = CARTESIAN_POINT ( 'NONE',  ( 27.95245687107222921, 57.97656249999997868, -2.463307335887066074E-13 ) ) ;
#13262 = ADVANCED_FACE ( 'NONE', ( #31571 ), #15469, .T. ) ;
#13263 = CARTESIAN_POINT ( 'NONE',  ( -10.37757302488624411, 54.72500000273118559, -31.93888565452638417 ) ) ;
#13264 = CARTESIAN_POINT ( 'NONE',  ( -20.75514604977248823, 17.07500000273119056, -28.56700777964554305 ) ) ;
#13265 = CARTESIAN_POINT ( 'NONE',  ( 27.16883889988624290, 6.175000002731190207, 19.73931689729373673 ) ) ;
#13266 = CARTESIAN_POINT ( 'NONE',  ( 19.09188309203694800, 41.21875000000000000, 19.09188309203660694 ) ) ;
#13267 = CARTESIAN_POINT ( 'NONE',  ( -30.02300923189239867, 33.63319416759063785, -0.04044903254991731589 ) ) ;
#13268 = CARTESIAN_POINT ( 'NONE',  ( -20.53372385742107653, 17.43711833240935505, -20.47846945139867003 ) ) ;
#13269 = CARTESIAN_POINT ( 'NONE',  ( 10.04305231718578817, 75.90000000546235981, -30.90933677959249337 ) ) ;
#13270 = CARTESIAN_POINT ( 'NONE',  ( 28.37133278852445528, 51.99999999999997868, -17.03823453610128524 ) ) ;
#13271 = CARTESIAN_POINT ( 'NONE',  ( 20.75514604977248467, 36.42500000273118843, -28.56700777964554305 ) ) ;
#13272 = CARTESIAN_POINT ( 'NONE',  ( -6.950374756619247307, 50.66628499907601935, 26.09010956794245217 ) ) ;
#13273 = CARTESIAN_POINT ( 'NONE',  ( -23.41746825000000598, 11.72499999726880127, 7.608796670333726198 ) ) ;
#13274 = DIRECTION ( 'NONE',  ( 0.000000000000000000, -1.000000000000000000, 0.000000000000000000 ) ) ;
#13275 = ORIENTED_EDGE ( 'NONE', *, *, #22119, .T. ) ;
#13276 = CARTESIAN_POINT ( 'NONE',  ( 27.16883889988623935, 44.57500000273119412, -19.73931689729374384 ) ) ;
#13277 = CARTESIAN_POINT ( 'NONE',  ( 2.375766604868043252, 77.44874571845312516, -14.99999999999999822 ) ) ;
#13278 = CARTESIAN_POINT ( 'NONE',  ( -27.95245687107223986, 43.94569416759065206, -0.04044903254993292840 ) ) ;
#13279 = CARTESIAN_POINT ( 'NONE',  ( 10.37757302488624767, 71.97500000273119269, 31.93888565452638417 ) ) ;
#13280 = ORIENTED_EDGE ( 'NONE', *, *, #32350, .F. ) ;
#13281 = CARTESIAN_POINT ( 'NONE',  ( -33.58253175000000113, 27.22500000273119269, 10.91162601494193929 ) ) ;
#13282 = CARTESIAN_POINT ( 'NONE',  ( -28.01184896238304134, 28.90104166666666785, -7.505752307972844761 ) ) ;
#13283 = ORIENTED_EDGE ( 'NONE', *, *, #16553, .T. ) ;
#13284 = VECTOR ( 'NONE', #3678, 1000.000000000000000 ) ;
#13285 = CARTESIAN_POINT ( 'NONE',  ( -26.29305231718579350, 57.80000000000000426, -19.10302069950537884 ) ) ;
#13286 = CARTESIAN_POINT ( 'NONE',  ( -27.16883889988624290, 60.92500000273118133, -19.73931689729374028 ) ) ;
#13287 = CARTESIAN_POINT ( 'NONE',  ( 26.00068869287340334, 47.37760416666666430, -15.01150461594642316 ) ) ;
#13288 =( BOUNDED_CURVE ( )  B_SPLINE_CURVE ( 2, ( #17908, #2273, #22698, #12747, #32973, #12401, #23044, #18074, #22871, #17386, #28523, #5018, #10006 ),
 .UNSPECIFIED., .F., .T. ) 
 B_SPLINE_CURVE_WITH_KNOTS ( ( 3, 2, 2, 2, 2, 2, 3 ),
 ( 0.3611111111111111049, 0.3666666666666666408, 0.3777777777777777679, 0.3888888888888888951, 0.4000000000000000222, 0.4111111111111110938, 0.4166666666666666852 ),
 .UNSPECIFIED. ) 
 CURVE ( )  GEOMETRIC_REPRESENTATION_ITEM ( )  RATIONAL_B_SPLINE_CURVE ( ( 0.9755282581475768211, 0.9755282581475768211, 1.000000000000000000, 0.9510565162951535312, 1.000000000000000000, 0.9510565162951535312, 1.000000000000000000, 0.9510565162951535312, 1.000000000000000000, 0.9510565162951535312, 1.000000000000000000, 0.9755282581475765991, 0.9755282581475767101 ) ) 
 REPRESENTATION_ITEM ( '' )  );
#13289 = CARTESIAN_POINT ( 'NONE',  ( 3.445340210940985210E-14, 7.249999994537621895, 24.50000000000000000 ) ) ;
#13290 = CARTESIAN_POINT ( 'NONE',  ( 18.94512977948576093, 9.324999997268824004, -13.76444248337722875 ) ) ;
#13291 = CARTESIAN_POINT ( 'NONE',  ( 33.58253175000000113, 2.125000002731192161, -4.112674001490185761E-15 ) ) ;
#13292 =( BOUNDED_CURVE ( )  B_SPLINE_CURVE ( 2, ( #28914, #20875, #4901, #15556, #20537, #30981, #28748, #31323, #7481, #2502, #15382, #5415, #23610 ),
 .UNSPECIFIED., .F., .F. ) 
 B_SPLINE_CURVE_WITH_KNOTS ( ( 3, 2, 2, 2, 2, 2, 3 ),
 ( 0.1500000000000000222, 0.1600000000000000033, 0.1799999999999999933, 0.2000000000000000111, 0.2200000000000000011, 0.2399999999999999911, 0.2500000000000000000 ),
 .UNSPECIFIED. ) 
 CURVE ( )  GEOMETRIC_REPRESENTATION_ITEM ( )  RATIONAL_B_SPLINE_CURVE ( ( 0.9755282581475768211, 0.9755282581475768211, 1.000000000000000000, 0.9510565162951535312, 1.000000000000000000, 0.9510565162951535312, 1.000000000000000000, 0.9510565162951535312, 1.000000000000000000, 0.9510565162951535312, 1.000000000000000000, 0.9755282581475768211, 0.9755282581475768211 ) ) 
 REPRESENTATION_ITEM ( '' )  );
#13293 = CARTESIAN_POINT ( 'NONE',  ( -10.37757302488623701, 29.77500000273120051, 31.93888565452638417 ) ) ;
#13294 = CARTESIAN_POINT ( 'NONE',  ( 20.08610463437157279, 5.800000005462378816, -27.64615127144129758 ) ) ;
#13295 = CARTESIAN_POINT ( 'NONE',  ( 15.04653450569339945, 60.54909749907603356, 25.98046417659831775 ) ) ;
#13296 = DIRECTION ( 'NONE',  ( 0.000000000000000000, 0.000000000000000000, -1.000000000000000000 ) ) ;
#13297 = CARTESIAN_POINT ( 'NONE',  ( -32.50000000000000000, 32.10000000000000142, 10.55989012756946366 ) ) ;
#13298 = CARTESIAN_POINT ( 'NONE',  ( -32.50000000000000000, 59.99999999999998579, 0.000000000000000000 ) ) ;
#13299 = CARTESIAN_POINT ( 'NONE',  ( -26.29305231718578995, 16.19999999999997797, 19.10302069950538595 ) ) ;
#13300 = CARTESIAN_POINT ( 'NONE',  ( 27.95245687107223276, 57.97656249999998579, -2.463307335887066074E-13 ) ) ;
#13301 = CARTESIAN_POINT ( 'NONE',  ( 7.570916362186207671, 19.34999999453762598, 23.30088464923126779 ) ) ;
#13302 = CARTESIAN_POINT ( 'NONE',  ( 15.00000000000000355, 71.15000000546237402, 4.873795443493592394 ) ) ;
#13303 = CARTESIAN_POINT ( 'NONE',  ( 26.07999730980490227, 30.61979166666666075, 6.988114217767821046 ) ) ;
#13304 = CARTESIAN_POINT ( 'NONE',  ( 20.75514604977249178, 21.82500000273119056, 28.56700777964553950 ) ) ;
#13305 = CARTESIAN_POINT ( 'NONE',  ( 10.37757302488624767, 73.72500000273117848, 31.93888565452638417 ) ) ;
#13306 = CARTESIAN_POINT ( 'NONE',  ( 33.58253175000000823, 38.27500000273118985, 10.91162601494192863 ) ) ;
#13307 = CARTESIAN_POINT ( 'NONE',  ( 20.75514604977248467, 18.67500000273120264, -28.56700777964554305 ) ) ;
#13308 = PRODUCT_RELATED_PRODUCT_CATEGORY ( 'part', '', ( #7096 ) ) ;
#13309 = CARTESIAN_POINT ( 'NONE',  ( -7.570916362186215665, 7.399999999999989697, 23.30088464923126423 ) ) ;
#13310 = CARTESIAN_POINT ( 'NONE',  ( 26.06988505166735592, 59.55767333425731636, 7.025853678916393896 ) ) ;
#13311 = CARTESIAN_POINT ( 'NONE',  ( -27.16883889988624290, 68.92500000273119554, -19.73931689729374028 ) ) ;
#13312 = CARTESIAN_POINT ( 'NONE',  ( -20.08610463437157989, 26.20000000546237828, -27.64615127144129758 ) ) ;
#13313 = VECTOR ( 'NONE', #1163, 1000.000000000000114 ) ;
#13314 = CARTESIAN_POINT ( 'NONE',  ( 32.50000000000000000, 57.00000000000000711, -3.980102097228898626E-15 ) ) ;
#13315 = DIRECTION ( 'NONE',  ( -1.000000000000000000, -1.224646799147353454E-16, 0.000000000000000000 ) ) ;
#13316 = CARTESIAN_POINT ( 'NONE',  ( -33.58253175000000113, 57.22500000273117848, 10.91162601494193929 ) ) ;
#13317 = AXIS2_PLACEMENT_3D ( 'NONE', #7922, #5007, #15490 ) ;
#13318 = CARTESIAN_POINT ( 'NONE',  ( 1.507698388325705758E-15, 9.624999997268808727, -24.62258325217400312 ) ) ;
#13319 = ORIENTED_EDGE ( 'NONE', *, *, #33695, .T. ) ;
#13320 = CARTESIAN_POINT ( 'NONE',  ( 33.58253175000000823, 74.27500000273117564, 10.91162601494192863 ) ) ;
#13321 = CARTESIAN_POINT ( 'NONE',  ( -5.147494310547377161, 61.55125428154684641, -32.50000000000002132 ) ) ;
#13322 = CARTESIAN_POINT ( 'NONE',  ( -14.47279130897152122, 16.42499999726882365, 19.92008829642072243 ) ) ;
#13323 = CARTESIAN_POINT ( 'NONE',  ( -14.01125832528285109, 12.43527750092397532, 24.18731323226248264 ) ) ;
#13324 = ORIENTED_EDGE ( 'NONE', *, *, #2724, .F. ) ;
#13325 = CARTESIAN_POINT ( 'NONE',  ( 33.58253175000000113, 40.22500000273119269, -10.91162601494193751 ) ) ;
#13326 = DIRECTION ( 'NONE',  ( -1.224646799147353454E-16, 1.000000000000000000, -0.000000000000000000 ) ) ;
#13327 = ORIENTED_EDGE ( 'NONE', *, *, #5171, .T. ) ;
#13328 = CARTESIAN_POINT ( 'NONE',  ( 7.505752307972854531, 46.94791666666666430, -28.01184896238303423 ) ) ;
#13329 = CARTESIAN_POINT ( 'NONE',  ( -32.50000000000000000, 60.60000000546239107, 10.55989012756946366 ) ) ;
#13330 = CARTESIAN_POINT ( 'NONE',  ( 32.50000000000000711, 3.400000005462381569, 10.55989012756945122 ) ) ;
#13331 = DIRECTION ( 'NONE',  ( -0.000000000000000000, 1.000000000000000000, -0.000000000000000000 ) ) ;
#13332 = CARTESIAN_POINT ( 'NONE',  ( 2.740863092043355209E-13, 24.46093749999999645, 30.02300923189239512 ) ) ;
#13333 = CARTESIAN_POINT ( 'NONE',  ( -4.523095164977116484E-15, 16.12499999726880873, 24.62258325217400312 ) ) ;
#13334 = CARTESIAN_POINT ( 'NONE',  ( 33.58253175000000113, 8.375000002731169957, -4.112674001490185761E-15 ) ) ;
#13335 = AXIS2_PLACEMENT_3D ( 'NONE', #9927, #20403, #7346 ) ;
#13336 = CARTESIAN_POINT ( 'NONE',  ( -26.29305231718578995, 58.20000000000000284, 19.10302069950538595 ) ) ;
#13337 = CARTESIAN_POINT ( 'NONE',  ( 4.300734207923761154, 77.47500000273119269, 13.23629886949340495 ) ) ;
#13338 = CARTESIAN_POINT ( 'NONE',  ( 20.08610463437158344, 73.20000000546238539, 27.64615127144129403 ) ) ;
#13339 = CARTESIAN_POINT ( 'NONE',  ( -30.02300923189239867, 30.75743083240935505, 0.04044903255044988294 ) ) ;
#13340 = CARTESIAN_POINT ( 'NONE',  ( 4.300734207923761154, 77.97500000273119269, 13.23629886949340495 ) ) ;
#13341 = CARTESIAN_POINT ( 'NONE',  ( 30.02300923189239867, 44.22656249999999289, -2.619432448724978208E-13 ) ) ;
#13342 = VECTOR ( 'NONE', #4671, 1000.000000000000000 ) ;
#13343 = DIRECTION ( 'NONE',  ( -0.000000000000000000, 1.000000000000000000, -0.000000000000000000 ) ) ;
#13344 = CARTESIAN_POINT ( 'NONE',  ( 32.50000000000000000, 65.00000000000000000, -3.980102097228898626E-15 ) ) ;
#13345 = CARTESIAN_POINT ( 'NONE',  ( -32.50000000000000000, 4.000000000000003553, 0.000000000000000000 ) ) ;
#13346 = CARTESIAN_POINT ( 'NONE',  ( -26.06988505166722803, 58.11420166574269075, 7.025853678916877953 ) ) ;
#13347 = CARTESIAN_POINT ( 'NONE',  ( 20.75514604977249178, 41.82500000273119412, 28.56700777964553950 ) ) ;
#13348 = CARTESIAN_POINT ( 'NONE',  ( 9.270509831248423538, 71.55000000546236549, -12.75976212528059861 ) ) ;
#13349 = CARTESIAN_POINT ( 'NONE',  ( 33.58253175000000113, 58.37500000273119838, -4.112674001490185761E-15 ) ) ;
#13350 = CARTESIAN_POINT ( 'NONE',  ( -10.37757302488624411, 36.97500000273118559, -31.93888565452638417 ) ) ;
#13351 = FACE_OUTER_BOUND ( 'NONE', #32150, .T. ) ;
#13352 = CARTESIAN_POINT ( 'NONE',  ( -27.95245687107223276, 25.32031250000000000, 2.498001805406602216E-13 ) ) ;
#13353 = CARTESIAN_POINT ( 'NONE',  ( 26.29305231718578995, 15.70000000546237295, -19.10302069950538240 ) ) ;
#13354 = CARTESIAN_POINT ( 'NONE',  ( 8.094135239392500125, 17.00000000000001421, -22.02093934509174389 ) ) ;
#13355 = CARTESIAN_POINT ( 'NONE',  ( 20.08610463437157279, 73.29999999999996874, -27.64615127144129758 ) ) ;
#13356 = CARTESIAN_POINT ( 'NONE',  ( 10.37757302488624767, 15.72500000273117848, 31.93888565452638417 ) ) ;
#13357 = DIRECTION ( 'NONE',  ( 0.000000000000000000, 0.000000000000000000, 1.000000000000000000 ) ) ;
#13358 = EDGE_CURVE ( 'NONE', #4493, #4016, #31327, .T. ) ;
#13359 = CARTESIAN_POINT ( 'NONE',  ( 0.000000000000000000, 74.00000000000001421, -9.000000000000001776 ) ) ;
#13360 = CARTESIAN_POINT ( 'NONE',  ( 14.01125832528330051, 22.73659749907601935, 24.18731323226221974 ) ) ;
#13361 = CARTESIAN_POINT ( 'NONE',  ( 6.277390505771533514E-15, 37.00000000546237544, 34.17252228774368916 ) ) ;
#13362 = CARTESIAN_POINT ( 'NONE',  ( -3.880418787951118276, 10.30125427608447097, -24.50000000000000355 ) ) ;
#13363 = CARTESIAN_POINT ( 'NONE',  ( -20.75514604977248112, 27.42500000273118488, 28.56700777964554661 ) ) ;
#13364 = CARTESIAN_POINT ( 'NONE',  ( 26.07999730980490227, 47.80729166666666430, 6.988114217767821046 ) ) ;
#13365 = TOROIDAL_SURFACE ( 'NONE', #6756, 30.16025403784430736, 1.500000000000010436 ) ;
#13366 = EDGE_CURVE ( 'NONE', #29691, #5024, #2238, .T. ) ;
#13367 = VERTEX_POINT ( 'NONE', #28832 ) ;
#13368 = CARTESIAN_POINT ( 'NONE',  ( 20.75514604977248467, 62.42500000273118133, -28.56700777964554305 ) ) ;
#13369 = EDGE_CURVE ( 'NONE', #21053, #1690, #2866, .T. ) ;
#13370 = VERTEX_POINT ( 'NONE', #26266 ) ;
#13371 = CARTESIAN_POINT ( 'NONE',  ( -26.00068869287340334, 14.72135416666666607, 15.01150461594643382 ) ) ;
#13372 = CARTESIAN_POINT ( 'NONE',  ( 20.53372385742072481, 17.73475666759064140, -20.47846945139902175 ) ) ;
#13373 = CARTESIAN_POINT ( 'NONE',  ( -20.75514604977248823, 2.825000002731177240, -28.56700777964554305 ) ) ;
#13374 = ORIENTED_EDGE ( 'NONE', *, *, #22144, .F. ) ;
#13375 = DIRECTION ( 'NONE',  ( 0.000000000000000000, 0.000000000000000000, -1.000000000000000000 ) ) ;
#13376 = CARTESIAN_POINT ( 'NONE',  ( 27.16883889988623935, 26.57500000273119056, -19.73931689729374384 ) ) ;
#13377 = CARTESIAN_POINT ( 'NONE',  ( 32.50000000000000000, 35.60000000546236976, -10.55989012756945833 ) ) ;
#13378 = CARTESIAN_POINT ( 'NONE',  ( -10.04305231718578462, 76.39999999999999147, 30.90933677959249337 ) ) ;
#13379 = CARTESIAN_POINT ( 'NONE',  ( -20.08610463437157989, 54.20000000546236407, -27.64615127144129758 ) ) ;
#13380 = CARTESIAN_POINT ( 'NONE',  ( 10.04305231718579705, 76.59999999999999432, 30.90933677959248982 ) ) ;
#13381 = CARTESIAN_POINT ( 'NONE',  ( 27.16883889988624290, 40.17500000273119554, 19.73931689729373673 ) ) ;
#13382 = CARTESIAN_POINT ( 'NONE',  ( -32.50000000000000000, 20.10000000000000497, 10.55989012756946366 ) ) ;
#13383 = CARTESIAN_POINT ( 'NONE',  ( 26.29305231718579350, 22.79999999999998650, 19.10302069950537529 ) ) ;
#13384 = CARTESIAN_POINT ( 'NONE',  ( -19.82091636218621389, 7.200000000000011724, 14.40073868116558842 ) ) ;
#13385 = CARTESIAN_POINT ( 'NONE',  ( 33.58253175000000823, 70.02500000273121827, 10.91162601494192863 ) ) ;
#13386 = CARTESIAN_POINT ( 'NONE',  ( -4.732186688966233175E-15, 3.249999994537627224, 25.76082449383753925 ) ) ;
#13387 = AXIS2_PLACEMENT_3D ( 'NONE', #1766, #30776, #12247 ) ;
#13388 = CARTESIAN_POINT ( 'NONE',  ( 3.164787637625844585, 74.00000000000002842, -14.10554145339599152 ) ) ;
#13389 = CARTESIAN_POINT ( 'NONE',  ( -33.58253175000000113, 53.47500000273117848, 10.91162601494193929 ) ) ;
#13390 = CARTESIAN_POINT ( 'NONE',  ( 26.29305231718578995, 39.70000000546236407, -19.10302069950538240 ) ) ;
#13391 = CARTESIAN_POINT ( 'NONE',  ( -33.58253175000000113, 9.225000002731178483, 10.91162601494193929 ) ) ;
#13392 = CARTESIAN_POINT ( 'NONE',  ( -26.06988505166735237, 30.33892333425730925, -7.025853678916388567 ) ) ;
#13393 =( BOUNDED_CURVE ( )  B_SPLINE_CURVE ( 2, ( #32192, #5783, #21905, #32356, #16264, #26720, #24148, #8850, #619, #11107, #21577, #32023, #26882 ),
 .UNSPECIFIED., .F., .T. ) 
 B_SPLINE_CURVE_WITH_KNOTS ( ( 3, 2, 2, 2, 2, 2, 3 ),
 ( 0.5833333333333333703, 0.5888888888888889062, 0.5999999999999999778, 0.6111111111111111605, 0.6222222222222222321, 0.6333333333333333037, 0.6388888888888889506 ),
 .UNSPECIFIED. ) 
 CURVE ( )  GEOMETRIC_REPRESENTATION_ITEM ( )  RATIONAL_B_SPLINE_CURVE ( ( 0.9755282581475768211, 0.9755282581475770431, 1.000000000000000000, 0.9510565162951535312, 1.000000000000000000, 0.9510565162951535312, 1.000000000000000000, 0.9510565162951535312, 1.000000000000000000, 0.9510565162951535312, 1.000000000000000000, 0.9755282581475765991, 0.9755282581475768211 ) ) 
 REPRESENTATION_ITEM ( '' )  );
#13394 = CARTESIAN_POINT ( 'NONE',  ( 7.570916362186207671, 9.349999994537617098, 23.30088464923126779 ) ) ;
#13395 = CARTESIAN_POINT ( 'NONE',  ( -25.94559702212997365, 52.00000000000000000, 20.21712673764820778 ) ) ;
#13396 = PRODUCT_DEFINITION_CONTEXT ( 'detailed design', #27843, 'design' ) ;
#13397 = CARTESIAN_POINT ( 'NONE',  ( 10.37757302488624767, 37.72500000273119980, 31.93888565452638417 ) ) ;
#13398 = CARTESIAN_POINT ( 'NONE',  ( 32.50000000000000000, 57.00000000000000711, -3.980102097228898626E-15 ) ) ;
#13399 = CARTESIAN_POINT ( 'NONE',  ( 33.58253175000000113, 52.37500000273119838, -4.112674001490185761E-15 ) ) ;
#13400 = CARTESIAN_POINT ( 'NONE',  ( -4.300734207923755825, 77.27500000273118985, 13.23629886949340673 ) ) ;
#13401 = CARTESIAN_POINT ( 'NONE',  ( -25.98046417659831420, 47.65847249907603356, 15.04653450569339945 ) ) ;
#13402 = CARTESIAN_POINT ( 'NONE',  ( -32.50000000000000000, 52.40000000546239534, -10.55989012756945478 ) ) ;
#13403 = CARTESIAN_POINT ( 'NONE',  ( 13.91746824999999532, 78.47500000273120691, -4.522059556121118540 ) ) ;
#13404 =( LENGTH_UNIT ( ) NAMED_UNIT ( * ) SI_UNIT ( .MILLI., .METRE. ) );
#13405 = CARTESIAN_POINT ( 'NONE',  ( 13.97622843553589966, 12.71614583333333037, -24.20753774853756113 ) ) ;
#13406 = CARTESIAN_POINT ( 'NONE',  ( 26.29305231718579350, 69.30000000546237970, 19.10302069950537529 ) ) ;
#13407 = CARTESIAN_POINT ( 'NONE',  ( 26.00068869287367335, 20.45052083333332504, 15.01150461594596308 ) ) ;
#13408 =( GEOMETRIC_REPRESENTATION_CONTEXT ( 3 ) GLOBAL_UNCERTAINTY_ASSIGNED_CONTEXT ( ( #26770 ) ) GLOBAL_UNIT_ASSIGNED_CONTEXT ( ( #24512, #14220, #32058 ) ) REPRESENTATION_CONTEXT ( 'NONE', 'WORKASPACE' ) );
#13409 = CARTESIAN_POINT ( 'NONE',  ( 33.58253175000000113, 26.47500000273118559, -10.91162601494193751 ) ) ;
#13410 = CARTESIAN_POINT ( 'NONE',  ( 14.47279130897151767, 14.82499999726881690, 19.92008829642072953 ) ) ;
#13411 = ORIENTED_EDGE ( 'NONE', *, *, #18187, .T. ) ;
#13412 = CARTESIAN_POINT ( 'NONE',  ( -7.543491769121417612, 36.35454833425730925, 28.00173670424549499 ) ) ;
#13413 = CARTESIAN_POINT ( 'NONE',  ( 6.277390505771533514E-15, 15.00000000546237722, 34.17252228774368916 ) ) ;
#13414 = CARTESIAN_POINT ( 'NONE',  ( -28.01184896238290278, 52.67708333333333570, 7.505752307973363457 ) ) ;
#13415 = CARTESIAN_POINT ( 'NONE',  ( 2.445080149700053643E-15, 72.50000000000001421, 15.00000000000000000 ) ) ;
#13416 = CARTESIAN_POINT ( 'NONE',  ( 10.37757302488624767, 51.97500000273119980, 31.93888565452638417 ) ) ;
#13417 = CARTESIAN_POINT ( 'NONE',  ( 20.08610463437157279, 55.80000000546236549, -27.64615127144129758 ) ) ;
#13418 = ADVANCED_FACE ( 'NONE', ( #161 ), #2417, .F. ) ;
#13419 = CARTESIAN_POINT ( 'NONE',  ( 0.000000000000000000, 80.00000000000001421, -32.50000000000000000 ) ) ;
#13420 = CARTESIAN_POINT ( 'NONE',  ( 6.486482029760649416E-15, 37.62500000273118417, 35.31076352940723240 ) ) ;
#13421 = DIRECTION ( 'NONE',  ( -1.000000000000000000, 0.000000000000000000, 0.000000000000000000 ) ) ;
#13422 = CARTESIAN_POINT ( 'NONE',  ( 10.37757302488624056, 66.77500000273117564, -31.93888565452638417 ) ) ;
#13423 = CARTESIAN_POINT ( 'NONE',  ( -33.58253175000000113, 59.22500000273119980, 10.91162601494193929 ) ) ;
#13424 = CARTESIAN_POINT ( 'NONE',  ( -7.505752307973343918, 22.59895833333332860, -28.01184896238290989 ) ) ;
#13425 = CARTESIAN_POINT ( 'NONE',  ( 26.29305231718578995, 43.20000000000001705, -19.10302069950538240 ) ) ;
#13426 = CARTESIAN_POINT ( 'NONE',  ( -14.47279130897152122, 1.924999997268818541, 19.92008829642072243 ) ) ;
#13427 = CARTESIAN_POINT ( 'NONE',  ( 10.37757302488624767, 9.975000002731187365, 31.93888565452638417 ) ) ;
#13428 = CARTESIAN_POINT ( 'NONE',  ( -32.50000000000000000, 66.50000000546239676, 0.000000000000000000 ) ) ;
#13429 = CARTESIAN_POINT ( 'NONE',  ( -27.95245687107223986, 34.19493083240935505, 0.04044903255043252877 ) ) ;
#13430 = CARTESIAN_POINT ( 'NONE',  ( 13.91746824999999887, 74.37500000273116996, -1.704398294459741270E-15 ) ) ;
#13431 = CARTESIAN_POINT ( 'NONE',  ( 27.16883889988624290, 76.17500000273119554, 19.73931689729373673 ) ) ;
#13432 = LINE ( 'NONE', #23900, #22083 ) ;
#13433 = CARTESIAN_POINT ( 'NONE',  ( -33.58253175000000113, 67.37500000273121259, 0.000000000000000000 ) ) ;
#13434 = ORIENTED_EDGE ( 'NONE', *, *, #21544, .F. ) ;
#13435 =( BOUNDED_CURVE ( )  B_SPLINE_CURVE ( 2, ( #11708, #6229, #5903, #1060, #11541, #22023, #19281, #16541, #13961, #16380, #11383, #24268, #3655 ),
 .UNSPECIFIED., .F., .T. ) 
 B_SPLINE_CURVE_WITH_KNOTS ( ( 3, 2, 2, 2, 2, 2, 3 ),
 ( 0.7500000000000000000, 0.7555555555555555358, 0.7666666666666667185, 0.7777777777777777901, 0.7888888888888888618, 0.8000000000000000444, 0.8055555555555555802 ),
 .UNSPECIFIED. ) 
 CURVE ( )  GEOMETRIC_REPRESENTATION_ITEM ( )  RATIONAL_B_SPLINE_CURVE ( ( 0.9755282581475768211, 0.9755282581475768211, 1.000000000000000000, 0.9510565162951535312, 1.000000000000000000, 0.9510565162951535312, 1.000000000000000000, 0.9510565162951535312, 1.000000000000000000, 0.9510565162951535312, 1.000000000000000000, 0.9755282581475768211, 0.9755282581475768211 ) ) 
 REPRESENTATION_ITEM ( '' )  );
#13436 = CARTESIAN_POINT ( 'NONE',  ( -23.41746824999999887, 18.12499999726882649, -2.867812753649727150E-15 ) ) ;
#13437 = VECTOR ( 'NONE', #3768, 1000.000000000000227 ) ;
#13438 = CARTESIAN_POINT ( 'NONE',  ( -24.20753774853756823, 56.54427083333332149, -13.97622843553588723 ) ) ;
#13439 = CARTESIAN_POINT ( 'NONE',  ( -10.37757302488623701, 51.52500000273117564, 31.93888565452638417 ) ) ;
#13440 = CARTESIAN_POINT ( 'NONE',  ( 6.486482029760649416E-15, 17.87500000273119838, 35.31076352940723240 ) ) ;
#13441 = CARTESIAN_POINT ( 'NONE',  ( -2.162160676586881955E-15, 2.875000002731189941, -35.31076352940723240 ) ) ;
#13442 = CARTESIAN_POINT ( 'NONE',  ( 2.584737979205442066E-13, 41.64843749999999289, 27.95245687107223276 ) ) ;
#13443 = CARTESIAN_POINT ( 'NONE',  ( -28.00173670424549499, 30.33892333425730925, -7.543491769121417612 ) ) ;
#13444 = CARTESIAN_POINT ( 'NONE',  ( -14.97647472619899389, 16.43451416574268720, 26.02091320914878025 ) ) ;
#13445 = CARTESIAN_POINT ( 'NONE',  ( 26.29305231718579350, 75.30000000546236549, 19.10302069950537529 ) ) ;
#13446 = CARTESIAN_POINT ( 'NONE',  ( 32.17340636219253724, 52.00000000000002842, -8.405285767817208153 ) ) ;
#13447 = CARTESIAN_POINT ( 'NONE',  ( -33.58253175000000113, 37.22500000273119980, 10.91162601494193929 ) ) ;
#13448 = CARTESIAN_POINT ( 'NONE',  ( 27.95245687107223276, 46.22618083240936215, -0.04044903255042905932 ) ) ;
#13449 = CARTESIAN_POINT ( 'NONE',  ( -4.523095164977116484E-15, 18.12499999726882649, 24.62258325217400312 ) ) ;
#13450 = CARTESIAN_POINT ( 'NONE',  ( -4.405589869732278832E-13, 9.000000005462366559, 32.50000000000000000 ) ) ;
#13451 = ORIENTED_EDGE ( 'NONE', *, *, #14403, .T. ) ;
#13452 = CARTESIAN_POINT ( 'NONE',  ( 33.58253175000000113, 50.47500000273117848, -10.91162601494193751 ) ) ;
#13453 = CARTESIAN_POINT ( 'NONE',  ( 12.13525491562421088, 76.80000000000003979, 8.816778784387095058 ) ) ;
#13454 = TOROIDAL_SURFACE ( 'NONE', #32601, 30.16025403784430736, 3.500000000000010658 ) ;
#13455 = CARTESIAN_POINT ( 'NONE',  ( 6.950374756619721595, 49.81809000092397355, 26.09010956794232428 ) ) ;
#13456 = CARTESIAN_POINT ( 'NONE',  ( -10.37757302488624411, 70.97500000273119269, -31.93888565452638417 ) ) ;
#13457 = ORIENTED_EDGE ( 'NONE', *, *, #17205, .T. ) ;
#13458 = CARTESIAN_POINT ( 'NONE',  ( -2.162160676586881955E-15, 14.62500000273118239, -35.31076352940723240 ) ) ;
#13459 = CARTESIAN_POINT ( 'NONE',  ( 30.02300923189239512, 27.03906250000000000, -2.619432448724977703E-13 ) ) ;
#13460 = AXIS2_PLACEMENT_3D ( 'NONE', #5605, #18151, #5435 ) ;
#13461 = EDGE_CURVE ( 'NONE', #7658, #22688, #12884, .T. ) ;
#13462 = ORIENTED_EDGE ( 'NONE', *, *, #27079, .F. ) ;
#13463 = DIRECTION ( 'NONE',  ( 0.000000000000000000, -1.000000000000000000, 0.000000000000000000 ) ) ;
#13464 = CARTESIAN_POINT ( 'NONE',  ( -10.37757302488623701, 63.52500000273120406, 31.93888565452638417 ) ) ;
#13465 = CARTESIAN_POINT ( 'NONE',  ( -2.584737979205441561E-13, 46.80468750000000000, -30.02300923189239512 ) ) ;
#13466 = ADVANCED_FACE ( 'NONE', ( #23185 ), #7901, .T. ) ;
#13467 = CARTESIAN_POINT ( 'NONE',  ( 32.50000000000000000, 19.50000000546236834, -3.980102097228898626E-15 ) ) ;
#13468 = CARTESIAN_POINT ( 'NONE',  ( 19.82091636218621034, 17.80000000000001137, 14.40073868116559730 ) ) ;
#13469 = CARTESIAN_POINT ( 'NONE',  ( -4.523095164977117273E-15, 8.624999997268810503, 24.62258325217400312 ) ) ;
#13470 = CARTESIAN_POINT ( 'NONE',  ( -20.75514604977248823, 4.825000002731171023, -28.56700777964554305 ) ) ;
#13471 = CARTESIAN_POINT ( 'NONE',  ( 10.37757302488624056, 28.77500000273120051, -31.93888565452638417 ) ) ;
#13472 = LINE ( 'NONE', #572, #26951 ) ;
#13473 = CARTESIAN_POINT ( 'NONE',  ( 7.468012846824281681, 59.26003499907601935, -28.02196122052058058 ) ) ;
#13474 = CARTESIAN_POINT ( 'NONE',  ( 2.667360163309149608E-15, 78.00000000546238255, -32.50000000000000000 ) ) ;
#13475 = CARTESIAN_POINT ( 'NONE',  ( -8.601468415847515203, 79.17500000273120975, 11.83890561707634959 ) ) ;
#13476 = CARTESIAN_POINT ( 'NONE',  ( 26.29305231718578995, 75.70000000546239960, -19.10302069950538240 ) ) ;
#13477 = CARTESIAN_POINT ( 'NONE',  ( 26.29305231718578995, 15.20000000000000462, -19.10302069950538240 ) ) ;
#13478 = CARTESIAN_POINT ( 'NONE',  ( 13.97622843553633842, 61.98697916666665719, 24.20753774853730889 ) ) ;
#13479 = CARTESIAN_POINT ( 'NONE',  ( 18.94512977948576093, 1.324999997268816454, -13.76444248337722875 ) ) ;
#13480 = CARTESIAN_POINT ( 'NONE',  ( -13.91746824999999532, 72.97500000273117848, 4.522059556121122093 ) ) ;
#13481 = CARTESIAN_POINT ( 'NONE',  ( -27.95245687107222921, 28.75781249999999645, 2.498001805406602216E-13 ) ) ;
#13482 = CARTESIAN_POINT ( 'NONE',  ( -33.58253175000000113, 27.12500000273118772, 0.000000000000000000 ) ) ;
#13483 = CARTESIAN_POINT ( 'NONE',  ( 10.37757302488624056, 74.52500000273120406, -31.93888565452638417 ) ) ;
#13484 = CARTESIAN_POINT ( 'NONE',  ( -27.16883889988624290, 35.17500000273120264, -19.73931689729374028 ) ) ;
#13485 = CARTESIAN_POINT ( 'NONE',  ( -33.58253175000000113, 17.47500000273118204, 10.91162601494193929 ) ) ;
#13486 = CARTESIAN_POINT ( 'NONE',  ( -19.06425588902591173, 54.68788166759063785, -19.11951029504763611 ) ) ;
#13487 = CARTESIAN_POINT ( 'NONE',  ( 6.486482029760648627E-15, 69.62500000273118417, 35.31076352940722529 ) ) ;
#13488 = CARTESIAN_POINT ( 'NONE',  ( 20.08610463437157279, 3.800000005462383257, -27.64615127144129758 ) ) ;
#13489 = CARTESIAN_POINT ( 'NONE',  ( 10.04305231718578817, 51.39999999999998437, -30.90933677959249337 ) ) ;
#13490 = LINE ( 'NONE', #29423, #23212 ) ;
#13491 = CARTESIAN_POINT ( 'NONE',  ( 27.16883889988624290, 59.92500000273118133, 19.73931689729373673 ) ) ;
#13492 = CARTESIAN_POINT ( 'NONE',  ( -18.94512977948576093, 14.32499999726880091, 13.76444248337722698 ) ) ;
#13493 = ORIENTED_EDGE ( 'NONE', *, *, #33800, .T. ) ;
#13494 = CARTESIAN_POINT ( 'NONE',  ( 10.37757302488624056, 66.77500000273118985, -31.93888565452638417 ) ) ;
#13495 = CARTESIAN_POINT ( 'NONE',  ( 6.486482029760648627E-15, 1.625000002731185944, 35.31076352940722529 ) ) ;
#13496 = CIRCLE ( 'NONE', #21170, 15.00000000000000000 ) ;
#13497 = CARTESIAN_POINT ( 'NONE',  ( 18.94512977948576093, 0.8249999972688160099, -13.76444248337722875 ) ) ;
#13498 = CARTESIAN_POINT ( 'NONE',  ( 14.01125832528286352, 24.46652750092397355, -24.18731323226246843 ) ) ;
#13499 =( BOUNDED_CURVE ( )  B_SPLINE_CURVE ( 2, ( #5148, #21451, #23686, #26594, #15458, #151, #16140, #2583, #25914, #3091, #10307, #31894, #20785 ),
 .UNSPECIFIED., .F., .T. ) 
 B_SPLINE_CURVE_WITH_KNOTS ( ( 3, 2, 2, 2, 2, 2, 3 ),
 ( 0.01923076923076923184, 0.02051282051282051280, 0.02307692307692307820, 0.02564102564102564014, 0.02820512820512820554, 0.03076923076923077094, 0.03205128205128205537 ),
 .UNSPECIFIED. ) 
 CURVE ( )  GEOMETRIC_REPRESENTATION_ITEM ( )  RATIONAL_B_SPLINE_CURVE ( ( 0.9755282581475768211, 0.9755282581475768211, 1.000000000000000000, 0.9510565162951535312, 1.000000000000000000, 0.9510565162951535312, 1.000000000000000000, 0.9510565162951535312, 1.000000000000000000, 0.9510565162951535312, 1.000000000000000000, 0.9755282581475767101, 0.9755282581475768211 ) ) 
 REPRESENTATION_ITEM ( '' )  );
#13500 = ORIENTED_EDGE ( 'NONE', *, *, #28224, .F. ) ;
#13501 = CARTESIAN_POINT ( 'NONE',  ( 27.16883889988623935, 40.32500000273118701, -19.73931689729374384 ) ) ;
#13502 = CARTESIAN_POINT ( 'NONE',  ( -24.50000000000000711, 1.099999999999994316, 7.960532557706201828 ) ) ;
#13503 = ORIENTED_EDGE ( 'NONE', *, *, #11001, .F. ) ;
#13505 = CARTESIAN_POINT ( 'NONE',  ( -26.00068869287340334, 45.65885416666666430, 15.01150461594643382 ) ) ;
#13504 =( BOUNDED_CURVE ( )  B_SPLINE_CURVE ( 2, ( #26870, #26370, #21396, #6097, #23629, #13329, #2859, #31842, #29595, #21564, #29098, #32009, #8504 ),
 .UNSPECIFIED., .F., .T. ) 
 B_SPLINE_CURVE_WITH_KNOTS ( ( 3, 2, 2, 2, 2, 2, 3 ),
 ( 0.2243589743589743668, 0.2256410256410256443, 0.2282051282051281993, 0.2307692307692307820, 0.2333333333333333370, 0.2358974358974358920, 0.2371794871794871973 ),
 .UNSPECIFIED. ) 
 CURVE ( )  GEOMETRIC_REPRESENTATION_ITEM ( )  RATIONAL_B_SPLINE_CURVE ( ( 0.9755282581475768211, 0.9755282581475768211, 1.000000000000000000, 0.9510565162951535312, 1.000000000000000000, 0.9510565162951535312, 1.000000000000000000, 0.9510565162951535312, 1.000000000000000000, 0.9510565162951535312, 1.000000000000000000, 0.9755282581475764880, 0.9755282581475768211 ) ) 
 REPRESENTATION_ITEM ( '' )  );
#13506 = CARTESIAN_POINT ( 'NONE',  ( 5.779280353836490358E-15, 4.500000000000003553, 32.49999999999999289 ) ) ;
#13507 = CARTESIAN_POINT ( 'NONE',  ( 20.08610463437157279, 59.30000000000001847, -27.64615127144129758 ) ) ;
#13508 = CARTESIAN_POINT ( 'NONE',  ( 32.50000000000000000, 27.50000000546237544, -3.980102097228898626E-15 ) ) ;
#13509 = CARTESIAN_POINT ( 'NONE',  ( -28.01184896238290278, 18.30208333333332860, 7.505752307973363457 ) ) ;
#13510 = CARTESIAN_POINT ( 'NONE',  ( -23.41746825000000598, 17.72499999726881725, 7.608796670333726198 ) ) ;
#13511 = CARTESIAN_POINT ( 'NONE',  ( -27.16883889988623935, 7.575000002731202997, 19.73931689729374739 ) ) ;
#13512 = CARTESIAN_POINT ( 'NONE',  ( -26.29305231718579350, 61.79999999999999716, -19.10302069950537884 ) ) ;
#13513 = CARTESIAN_POINT ( 'NONE',  ( -11.25946833292375793, 78.67500000273119554, -8.180482586598733619 ) ) ;
#13514 = LINE ( 'NONE', #448, #15408 ) ;
#13515 = CARTESIAN_POINT ( 'NONE',  ( 28.00173670424535644, 35.77045166574266943, -7.543491769121920321 ) ) ;
#13516 = CARTESIAN_POINT ( 'NONE',  ( 13.91746824999999887, 78.37500000273116996, -1.704398294459741270E-15 ) ) ;
#13517 = CARTESIAN_POINT ( 'NONE',  ( -26.00068869287340334, 52.53385416666666430, 15.01150461594643559 ) ) ;
#13518 = DIRECTION ( 'NONE',  ( -0.000000000000000000, 1.000000000000000000, -0.000000000000000000 ) ) ;
#13519 = CARTESIAN_POINT ( 'NONE',  ( 20.08610463437157279, 65.29999999999999716, -27.64615127144129758 ) ) ;
#13520 = CARTESIAN_POINT ( 'NONE',  ( -20.08610463437156923, 2.299999999999985612, 27.64615127144130113 ) ) ;
#13521 = CARTESIAN_POINT ( 'NONE',  ( 5.147494310547426899, 17.94874572391552547, -32.50000000000000000 ) ) ;
#13522 = CARTESIAN_POINT ( 'NONE',  ( 19.06425588902558133, 62.98399333240935505, -19.11951029504797006 ) ) ;
#13523 = CARTESIAN_POINT ( 'NONE',  ( -27.16883889988624290, 44.92500000273119554, -19.73931689729374028 ) ) ;
#13524 = CARTESIAN_POINT ( 'NONE',  ( 15.00000000000000355, 73.15000000546237402, 4.873795443493592394 ) ) ;
#13525 = CARTESIAN_POINT ( 'NONE',  ( -33.58253175000000113, 57.37500000273119838, 0.000000000000000000 ) ) ;
#13526 = CARTESIAN_POINT ( 'NONE',  ( -27.16883889988624290, 33.17500000273118843, -19.73931689729374028 ) ) ;
#13527 = CARTESIAN_POINT ( 'NONE',  ( 1.836970198721029589E-15, 74.00000000000001421, -15.00000000000000000 ) ) ;
#13528 = CARTESIAN_POINT ( 'NONE',  ( -27.95245687107223276, 18.44531249999999645, 2.498001805406602216E-13 ) ) ;
#13529 = CARTESIAN_POINT ( 'NONE',  ( -2.375766604868044141, 79.80125428700922896, -14.99999999999999822 ) ) ;
#13530 = ADVANCED_FACE ( 'NONE', ( #10144 ), #23695, .F. ) ;
#13531 = CARTESIAN_POINT ( 'NONE',  ( -1.778240108872766143E-15, 44.00000000546238255, -32.49999999999999289 ) ) ;
#13532 = CARTESIAN_POINT ( 'NONE',  ( -32.50000000000000000, 74.00000000000000000, 0.000000000000000000 ) ) ;
#13533 = CARTESIAN_POINT ( 'NONE',  ( 33.58253175000000113, 8.225000002731182036, -10.91162601494193751 ) ) ;
#13534 = CARTESIAN_POINT ( 'NONE',  ( -14.47279130897152299, 3.924999997268813878, 19.92008829642072243 ) ) ;
#13535 = CARTESIAN_POINT ( 'NONE',  ( 3.445340210940985210E-14, 9.249999994537636994, 24.50000000000000000 ) ) ;
#13536 = CARTESIAN_POINT ( 'NONE',  ( 19.06425588902558133, 25.17149333240934439, -19.11951029504797006 ) ) ;
#13537 = CARTESIAN_POINT ( 'NONE',  ( 0.000000000000000000, -20.99999999999998934, 0.000000000000000000 ) ) ;
#13538 = CARTESIAN_POINT ( 'NONE',  ( -33.58253175000000113, 19.12500000273118062, 0.000000000000000000 ) ) ;
#13539 = CARTESIAN_POINT ( 'NONE',  ( 2.584737979205441561E-13, 48.52343750000000000, 27.95245687107222921 ) ) ;
#13540 = ORIENTED_EDGE ( 'NONE', *, *, #9492, .T. ) ;
#13541 = CARTESIAN_POINT ( 'NONE',  ( -10.37757302488623701, 65.52500000273118985, 31.93888565452638417 ) ) ;
#13542 = VERTEX_POINT ( 'NONE', #28327 ) ;
#13543 = CARTESIAN_POINT ( 'NONE',  ( 30.02300923189239512, 13.28906249999999289, -2.619432448724977703E-13 ) ) ;
#13544 = CARTESIAN_POINT ( 'NONE',  ( 15.04653450569292872, 10.71652750092397888, -25.98046417659857710 ) ) ;
#13545 = CARTESIAN_POINT ( 'NONE',  ( 27.16883889988624290, 7.925000002731205306, 19.73931689729373673 ) ) ;
#13546 = ORIENTED_EDGE ( 'NONE', *, *, #18413, .F. ) ;
#13547 = DIRECTION ( 'NONE',  ( -0.000000000000000000, -1.000000000000000000, -0.000000000000000000 ) ) ;
#13548 = AXIS2_PLACEMENT_3D ( 'NONE', #24237, #708, #32110 ) ;
#13549 = CARTESIAN_POINT ( 'NONE',  ( -33.58253175000000113, 31.37500000273119127, 0.000000000000000000 ) ) ;
#13550 = CARTESIAN_POINT ( 'NONE',  ( 26.29305231718579350, 35.30000000546237970, 19.10302069950537529 ) ) ;
#13551 = CARTESIAN_POINT ( 'NONE',  ( 4.635254915624212657, 72.59999999999999432, 14.26584774442730286 ) ) ;
#13552 = CARTESIAN_POINT ( 'NONE',  ( 32.50000000000000000, 33.60000000546236976, -10.55989012756945833 ) ) ;
#13553 = CARTESIAN_POINT ( 'NONE',  ( 2.445080149700053643E-15, 72.50000000000001421, 15.00000000000000000 ) ) ;
#13554 = CARTESIAN_POINT ( 'NONE',  ( -20.75514604977248112, 43.67500000273119554, 28.56700777964554661 ) ) ;
#13555 =( NAMED_UNIT ( * ) SI_UNIT ( $, .STERADIAN. ) SOLID_ANGLE_UNIT ( ) );
#13556 = EDGE_CURVE ( 'NONE', #24301, #679, #1736, .T. ) ;
#13557 = CIRCLE ( 'NONE', #3143, 4.000000000000014211 ) ;
#13558 = CARTESIAN_POINT ( 'NONE',  ( -26.29305231718578995, 26.19999999999998863, 19.10302069950538595 ) ) ;
#13559 = CARTESIAN_POINT ( 'NONE',  ( -26.29305231718579350, 19.79999999999998295, -19.10302069950537884 ) ) ;
#13560 = CARTESIAN_POINT ( 'NONE',  ( -7.570916362186215665, 3.399999999999986144, 23.30088464923126423 ) ) ;
#13561 = CARTESIAN_POINT ( 'NONE',  ( 20.75514604977249178, 61.82500000273116569, 28.56700777964553950 ) ) ;
#13562 = CARTESIAN_POINT ( 'NONE',  ( -33.02351622650638063, 66.99999999999997158, 4.441931073548307296 ) ) ;
#13563 = CARTESIAN_POINT ( 'NONE',  ( -4.150128892133675862, 74.00000000000002842, -14.13113817901305680 ) ) ;
#13564 = CARTESIAN_POINT ( 'NONE',  ( -10.37757302488624411, 50.97500000273119980, -31.93888565452638417 ) ) ;
#13565 = CARTESIAN_POINT ( 'NONE',  ( -7.236395654485757944, 5.224999997268803043, -22.27133577429736988 ) ) ;
#13566 = EDGE_CURVE ( 'NONE', #27363, #3936, #32244, .T. ) ;
#13567 = CARTESIAN_POINT ( 'NONE',  ( 20.75514604977248467, 6.425000002731179549, -28.56700777964554305 ) ) ;
#13568 = CARTESIAN_POINT ( 'NONE',  ( 14.01125832528286352, 31.34152750092398421, -24.18731323226246843 ) ) ;
#13569 = CARTESIAN_POINT ( 'NONE',  ( 21.34420727114686400, 16.99999999999998934, -9.663798758747949691 ) ) ;
#13570 = CARTESIAN_POINT ( 'NONE',  ( 3.724851327375194643, 52.00000000000000000, 33.24794091741933499 ) ) ;
#13571 = CARTESIAN_POINT ( 'NONE',  ( 6.486482029760649416E-15, 31.62500000273119483, 35.31076352940723240 ) ) ;
#13572 = CARTESIAN_POINT ( 'NONE',  ( 2.445080149700053643E-15, 70.75000000546236834, 15.00000000000000000 ) ) ;
#13573 = CARTESIAN_POINT ( 'NONE',  ( -5.147494310547423346, 58.94874572391553613, 32.50000000000000000 ) ) ;
#13574 = ADVANCED_FACE ( 'NONE', ( #8573 ), #19220, .T. ) ;
#13575 = CARTESIAN_POINT ( 'NONE',  ( -13.91746824999999887, 74.87500000273116996, 0.000000000000000000 ) ) ;
#13576 = CARTESIAN_POINT ( 'NONE',  ( -15.04653450569338524, 45.08034749907603356, -25.98046417659831775 ) ) ;
#13577 = CARTESIAN_POINT ( 'NONE',  ( -32.50000000000000000, 56.40000000546238113, -10.55989012756945478 ) ) ;
#13578 = FACE_OUTER_BOUND ( 'NONE', #17581, .T. ) ;
#13579 = SURFACE_SIDE_STYLE ('',( #342 ) ) ;
#13580 = CARTESIAN_POINT ( 'NONE',  ( 6.988114217768294445, 17.44270833333333215, 26.07999730980477437 ) ) ;
#13581 = CIRCLE ( 'NONE', #2601, 26.50000000000000000 ) ;
#13582 = CARTESIAN_POINT ( 'NONE',  ( -26.29305231718578995, 66.70000000546238539, 19.10302069950538595 ) ) ;
#13583 = CARTESIAN_POINT ( 'NONE',  ( 20.50609665441005092, 24.03124999999999645, 20.50609665440969209 ) ) ;
#13584 = CARTESIAN_POINT ( 'NONE',  ( -7.236395654485757944, 15.72499999726881192, -22.27133577429736988 ) ) ;
#13585 = ORIENTED_EDGE ( 'NONE', *, *, #1215, .F. ) ;
#13586 = CARTESIAN_POINT ( 'NONE',  ( 14.97647472619947351, 39.36236083425731636, 26.02091320914850314 ) ) ;
#13587 = CARTESIAN_POINT ( 'NONE',  ( 20.08610463437157279, 19.80000000546237260, -27.64615127144129758 ) ) ;
#13588 = CARTESIAN_POINT ( 'NONE',  ( 26.00068869287340334, 50.81510416666667140, -15.01150461594642316 ) ) ;
#13589 = CARTESIAN_POINT ( 'NONE',  ( 33.58253175000000113, 48.37500000273120548, -4.112674001490185761E-15 ) ) ;
#13590 = CARTESIAN_POINT ( 'NONE',  ( 26.29305231718579350, 59.30000000546237260, 19.10302069950537529 ) ) ;
#13591 = CARTESIAN_POINT ( 'NONE',  ( 11.25946833292375793, 80.17500000273119554, 8.180482586598731842 ) ) ;
#13592 = CARTESIAN_POINT ( 'NONE',  ( 33.58253175000000113, 34.22500000273117848, -10.91162601494193751 ) ) ;
#13593 = CARTESIAN_POINT ( 'NONE',  ( 15.00000000000000000, 73.35000000546237686, -4.873795443493596835 ) ) ;
#13594 = CARTESIAN_POINT ( 'NONE',  ( -20.75514604977248112, 61.67500000273117422, 28.56700777964554661 ) ) ;
#13595 = CARTESIAN_POINT ( 'NONE',  ( 6.987962563135265093, 74.00000000000002842, 12.07036192619727721 ) ) ;
#13596 = CARTESIAN_POINT ( 'NONE',  ( -27.16883889988624290, 56.92500000273119554, -19.73931689729374028 ) ) ;
#13597 = CARTESIAN_POINT ( 'NONE',  ( 26.00068869287341045, 19.87760416666666430, -15.01150461594642493 ) ) ;
#13598 = CARTESIAN_POINT ( 'NONE',  ( 10.04305231718578817, 41.39999999999999147, -30.90933677959249337 ) ) ;
#13599 = CARTESIAN_POINT ( 'NONE',  ( -14.47279130897151589, 5.324999997268826668, -19.92008829642072598 ) ) ;
#13600 =( BOUNDED_CURVE ( )  B_SPLINE_CURVE ( 2, ( #1892, #27645, #32776, #17353, #19754, #25414, #20272, #25752, #33117, #2236, #4133 ),
 .UNSPECIFIED., .F., .F. ) 
 B_SPLINE_CURVE_WITH_KNOTS ( ( 3, 2, 2, 2, 2, 3 ),
 ( 0.5500000000000000444, 0.5600000000000000533, 0.5799999999999999600, 0.5999999999999999778, 0.6199999999999999956, 0.6250928956683751148 ),
 .UNSPECIFIED. ) 
 CURVE ( )  GEOMETRIC_REPRESENTATION_ITEM ( )  RATIONAL_B_SPLINE_CURVE ( ( 0.9755282581475768211, 0.9755282581475768211, 1.000000000000000000, 0.9510565162951535312, 1.000000000000000000, 0.9510565162951535312, 1.000000000000000000, 0.9510565162951535312, 1.000000000000000000, 0.9875367971922199839, 0.9814209735438224058 ) ) 
 REPRESENTATION_ITEM ( '' )  );
#13601 = CARTESIAN_POINT ( 'NONE',  ( -27.16883889988624290, 5.175000002731189319, -19.73931689729374028 ) ) ;
#13602 = CARTESIAN_POINT ( 'NONE',  ( 32.50000000000000000, 35.50000000546238255, -3.980102097228898626E-15 ) ) ;
#13603 = CARTESIAN_POINT ( 'NONE',  ( 8.601468415847520532, 72.07500000273120122, 11.83890561707634781 ) ) ;
#13604 = CARTESIAN_POINT ( 'NONE',  ( -33.58253175000000113, 71.47500000273120691, 10.91162601494193929 ) ) ;
#13605 = DIRECTION ( 'NONE',  ( 0.000000000000000000, 0.000000000000000000, -1.000000000000000000 ) ) ;
#13606 = CARTESIAN_POINT ( 'NONE',  ( -33.58253175000000113, 69.47500000273116427, 10.91162601494193929 ) ) ;
#13607 = EDGE_LOOP ( 'NONE', ( #25388, #25278, #24580, #31209 ) ) ;
#13608 = CARTESIAN_POINT ( 'NONE',  ( 23.41746825000000243, 17.02499999726880731, 7.608796670333735079 ) ) ;
#13609 = AXIS2_PLACEMENT_3D ( 'NONE', #31973, #13637, #24101 ) ;
#13610 = CARTESIAN_POINT ( 'NONE',  ( -19.09188309203660694, 55.82812499999999289, 19.09188309203694800 ) ) ;
#13611 = CARTESIAN_POINT ( 'NONE',  ( -27.16883889988624290, 50.92500000273118843, -19.73931689729374028 ) ) ;
#13612 = CARTESIAN_POINT ( 'NONE',  ( -33.58253175000000113, 13.37500000273118772, 0.000000000000000000 ) ) ;
#13613 = CARTESIAN_POINT ( 'NONE',  ( 27.16883889988624290, 4.175000002731188431, 19.73931689729373673 ) ) ;
#13614 = CARTESIAN_POINT ( 'NONE',  ( -2.428612866367529427E-13, 36.49218749999999289, -27.95245687107223276 ) ) ;
#13615 = CARTESIAN_POINT ( 'NONE',  ( -0.04044903254990864921, 29.33631916759064850, 30.02300923189239867 ) ) ;
#13616 = CARTESIAN_POINT ( 'NONE',  ( 20.53372385742108008, 15.71836833240935327, 20.47846945139866648 ) ) ;
#13617 = CARTESIAN_POINT ( 'NONE',  ( 10.04305231718579705, 73.10000000546239107, 30.90933677959248982 ) ) ;
#13618 = CARTESIAN_POINT ( 'NONE',  ( 13.91746824999999532, 79.97500000273115006, -4.522059556121118540 ) ) ;
#13619 = CARTESIAN_POINT ( 'NONE',  ( -2.162160676586882350E-15, 40.62500000273120548, -35.31076352940722529 ) ) ;
#13620 = CARTESIAN_POINT ( 'NONE',  ( 27.95245687107223276, 49.66368083240936215, -0.04044903255042905932 ) ) ;
#13621 = CARTESIAN_POINT ( 'NONE',  ( -14.47279130897152122, 13.92499999726881654, 19.92008829642072243 ) ) ;
#13622 = FACE_OUTER_BOUND ( 'NONE', #6742, .T. ) ;
#13623 = ORIENTED_EDGE ( 'NONE', *, *, #8918, .T. ) ;
#13624 = CARTESIAN_POINT ( 'NONE',  ( -2.162160676586881955E-15, 44.87500000273119127, -35.31076352940723240 ) ) ;
#13625 = CARTESIAN_POINT ( 'NONE',  ( -26.29305231718579350, 50.30000000546236549, -19.10302069950537884 ) ) ;
#13626 = ADVANCED_BREP_SHAPE_REPRESENTATION ( '', ( #9785, #1376 ), #33173 ) ;
#13627 = CARTESIAN_POINT ( 'NONE',  ( -19.06425588902591173, 54.68788166759063785, -19.11951029504763611 ) ) ;
#13628 = CARTESIAN_POINT ( 'NONE',  ( 27.16883889988623935, 72.57500000273120122, -19.73931689729374384 ) ) ;
#13629 = EDGE_LOOP ( 'NONE', ( #17159, #17849, #27786, #18779 ) ) ;
#13630 = CARTESIAN_POINT ( 'NONE',  ( -20.75514604977248112, 15.42500000273118843, 28.56700777964554661 ) ) ;
#13631 = CARTESIAN_POINT ( 'NONE',  ( -30.02300923189239512, 21.88281249999999645, 2.654126918244515359E-13 ) ) ;
#13632 = ORIENTED_EDGE ( 'NONE', *, *, #29589, .T. ) ;
#13633 = CARTESIAN_POINT ( 'NONE',  ( 0.000000000000000000, 80.00000000000001421, 0.000000000000000000 ) ) ;
#13634 = CARTESIAN_POINT ( 'NONE',  ( -2.162160676586881955E-15, 54.62500000273116996, -35.31076352940723240 ) ) ;
#13635 = CARTESIAN_POINT ( 'NONE',  ( -30.02300923189239512, 49.38281249999997868, 2.654126918244515359E-13 ) ) ;
#13636 = CARTESIAN_POINT ( 'NONE',  ( -32.50000000000000000, 20.40000000546238113, -10.55989012756945478 ) ) ;
#13637 = DIRECTION ( 'NONE',  ( 0.000000000000000000, -0.000000000000000000, -1.000000000000000000 ) ) ;
#13638 = CARTESIAN_POINT ( 'NONE',  ( -23.41746824999999887, 6.024999997268805529, -7.608796670333730638 ) ) ;
#13639 = CARTESIAN_POINT ( 'NONE',  ( -33.58253175000000113, 27.37500000273118772, 0.000000000000000000 ) ) ;
#13640 = CARTESIAN_POINT ( 'NONE',  ( -12.13525491562421088, 78.05000000546239391, -8.816778784387096835 ) ) ;
#13641 = CARTESIAN_POINT ( 'NONE',  ( 28.02196122052058413, 63.55690999907603356, 7.468012846824272799 ) ) ;
#13642 = CARTESIAN_POINT ( 'NONE',  ( -8.601468415847518756, 80.57500000273118701, -11.83890561707634781 ) ) ;
#13643 = CARTESIAN_POINT ( 'NONE',  ( -32.50000000000000000, 3.899999999999992806, -10.55989012756945300 ) ) ;
#13644 = CARTESIAN_POINT ( 'NONE',  ( -26.29305231718578995, 12.20000000000000284, 19.10302069950538595 ) ) ;
#13645 = CARTESIAN_POINT ( 'NONE',  ( -27.95245687107223276, 63.13281249999999289, 2.498001805406602216E-13 ) ) ;
#13646 = CARTESIAN_POINT ( 'NONE',  ( 15.14183272437241889, 17.44999999453761319, 20.84094480462498211 ) ) ;
#13647 = CARTESIAN_POINT ( 'NONE',  ( 13.91746824999999532, 75.97500000273119269, -4.522059556121118540 ) ) ;
#13648 = CARTESIAN_POINT ( 'NONE',  ( 19.09188309203694800, 30.90624999999999645, 19.09188309203660694 ) ) ;
#13649 = CARTESIAN_POINT ( 'NONE',  ( -33.58253175000000113, 25.22500000273119625, 10.91162601494193929 ) ) ;
#13650 = CARTESIAN_POINT ( 'NONE',  ( 27.16883889988623935, 74.32500000273118701, -19.73931689729374384 ) ) ;
#13651 = CARTESIAN_POINT ( 'NONE',  ( 20.75514604977249178, 32.07500000273117990, 28.56700777964553950 ) ) ;
#13652 = CARTESIAN_POINT ( 'NONE',  ( -27.16883889988623935, 17.57500000273118346, 19.73931689729374739 ) ) ;
#13653 = CARTESIAN_POINT ( 'NONE',  ( 13.94119854578937812, 59.98736083425730925, 24.22776226481240514 ) ) ;
#13654 = CARTESIAN_POINT ( 'NONE',  ( 20.75514604977249178, 67.82500000273118701, 28.56700777964553950 ) ) ;
#13655 = CARTESIAN_POINT ( 'NONE',  ( 0.000000000000000000, 80.00000000000001421, 0.000000000000000000 ) ) ;
#13656 = EDGE_CURVE ( 'NONE', #14202, #6637, #32407, .T. ) ;
#13657 = CARTESIAN_POINT ( 'NONE',  ( 6.277390505771533514E-15, 56.49999999999998579, 34.17252228774368916 ) ) ;
#13658 = CARTESIAN_POINT ( 'NONE',  ( 3.880418787951153803, 7.301254276084462091, 24.49999999999999645 ) ) ;
#13659 = CARTESIAN_POINT ( 'NONE',  ( -20.75514604977248112, 59.42500000273118843, 28.56700777964554661 ) ) ;
#13660 = EDGE_CURVE ( 'NONE', #20850, #22505, #843, .T. ) ;
#13661 = CARTESIAN_POINT ( 'NONE',  ( -23.41746825000000243, 18.02499999726880731, -7.608796670333730638 ) ) ;
#13662 = ORIENTED_EDGE ( 'NONE', *, *, #27334, .T. ) ;
#13663 = CARTESIAN_POINT ( 'NONE',  ( -20.75514604977248823, 65.07500000273118701, -28.56700777964554305 ) ) ;
#13664 = CYLINDRICAL_SURFACE ( 'NONE', #10806, 24.50000000000000000 ) ;
#13665 = CARTESIAN_POINT ( 'NONE',  ( -4.523095164977116484E-15, 6.124999997268802510, 24.62258325217400312 ) ) ;
#13666 = CARTESIAN_POINT ( 'NONE',  ( -13.94119854578936923, 20.45611083425730925, -24.22776226481241224 ) ) ;
#13667 = ORIENTED_EDGE ( 'NONE', *, *, #4651, .F. ) ;
#13668 = CARTESIAN_POINT ( 'NONE',  ( -2.162160676586881955E-15, 34.62500000273119127, -35.31076352940723240 ) ) ;
#13669 = CARTESIAN_POINT ( 'NONE',  ( -32.50000000000000000, 42.40000000546238823, -10.55989012756945300 ) ) ;
#13670 = ORIENTED_EDGE ( 'NONE', *, *, #25723, .T. ) ;
#13671 = CARTESIAN_POINT ( 'NONE',  ( -26.00068869287340334, 55.97135416666665719, 15.01150461594643382 ) ) ;
#13672 = CARTESIAN_POINT ( 'NONE',  ( 1.102182119232617911E-15, 102.0000000000000284, 9.000000000000001776 ) ) ;
#13673 = CARTESIAN_POINT ( 'NONE',  ( 5.779280353836490358E-15, 58.49999999999999289, 32.49999999999999289 ) ) ;
#13674 = CARTESIAN_POINT ( 'NONE',  ( 27.16883889988623935, 74.32500000273117280, -19.73931689729374384 ) ) ;
#13675 = CARTESIAN_POINT ( 'NONE',  ( 20.50609665441005092, 20.59374999999999645, 20.50609665440969209 ) ) ;
#13676 = CARTESIAN_POINT ( 'NONE',  ( 7.570916362186207671, 1.599999999999990319, 23.30088464923126779 ) ) ;
#13677 = CARTESIAN_POINT ( 'NONE',  ( 27.16883889988624290, 12.17500000273119554, 19.73931689729373673 ) ) ;
#13678 = CARTESIAN_POINT ( 'NONE',  ( 20.75514604977248467, 20.42500000273120619, -28.56700777964554305 ) ) ;
#13679 = CARTESIAN_POINT ( 'NONE',  ( 10.04305231718579705, 57.10000000546239107, 30.90933677959248982 ) ) ;
#13680 = DIRECTION ( 'NONE',  ( -1.000000000000000000, 0.000000000000000000, 0.000000000000000000 ) ) ;
#13681 = CARTESIAN_POINT ( 'NONE',  ( 25.98046417659831775, 32.18972249907602645, -15.04653450569338879 ) ) ;
#13682 = CARTESIAN_POINT ( 'NONE',  ( -4.300734207923755825, 73.77500000273118985, 13.23629886949340673 ) ) ;
#13683 = CARTESIAN_POINT ( 'NONE',  ( -7.505752307972844761, 52.10416666666666430, 28.01184896238304134 ) ) ;
#13684 = CARTESIAN_POINT ( 'NONE',  ( -1.778240108872766143E-15, 54.00000000546237544, -32.49999999999999289 ) ) ;
#13685 = CARTESIAN_POINT ( 'NONE',  ( 32.50000000000000000, 49.60000000546239107, -10.55989012756945833 ) ) ;
#13686 = CARTESIAN_POINT ( 'NONE',  ( -19.06425588902558133, 61.26524333240935505, 19.11951029504797006 ) ) ;
#13687 = CARTESIAN_POINT ( 'NONE',  ( -27.16883889988623935, 41.32500000273120122, 19.73931689729374739 ) ) ;
#13688 = CARTESIAN_POINT ( 'NONE',  ( -13.91746824999999532, 78.77500000273117564, -4.522059556121115875 ) ) ;
#13689 = CARTESIAN_POINT ( 'NONE',  ( 33.58253175000000823, 54.27500000273118275, 10.91162601494192863 ) ) ;
#13690 = CARTESIAN_POINT ( 'NONE',  ( 20.75514604977248467, 34.67500000273118843, -28.56700777964554305 ) ) ;
#13691 = CARTESIAN_POINT ( 'NONE',  ( -4.779127830720365289, 16.99999999999998224, 23.70577217035268092 ) ) ;
#13692 = CARTESIAN_POINT ( 'NONE',  ( -24.20753774853756823, 25.60677083333332860, -13.97622843553588723 ) ) ;
#13693 = CARTESIAN_POINT ( 'NONE',  ( -1.778240108872766143E-15, 11.49999999999999112, -32.49999999999999289 ) ) ;
#13694 = CARTESIAN_POINT ( 'NONE',  ( 26.29305231718579350, 30.79999999999999361, 19.10302069950537529 ) ) ;
#13695 = CARTESIAN_POINT ( 'NONE',  ( -26.29305231718579350, 75.80000000000002558, -19.10302069950537884 ) ) ;
#13696 = CARTESIAN_POINT ( 'NONE',  ( 10.37757302488624056, 10.52500000273119696, -31.93888565452638417 ) ) ;
#13697 = CARTESIAN_POINT ( 'NONE',  ( -23.41746824999999887, 1.524999997268801755, -7.608796670333730638 ) ) ;
#13698 =( BOUNDED_CURVE ( )  B_SPLINE_CURVE ( 2, ( #720, #9119, #24738, #11368, #16364, #26819, #14448, #32289, #21678, #8621, #19103, #29541, #29883 ),
 .UNSPECIFIED., .F., .T. ) 
 B_SPLINE_CURVE_WITH_KNOTS ( ( 3, 2, 2, 2, 2, 2, 3 ),
 ( 0.8269230769230769829, 0.8282051282051282604, 0.8307692307692308153, 0.8333333333333333703, 0.8358974358974359253, 0.8384615384615384803, 0.8397435897435897578 ),
 .UNSPECIFIED. ) 
 CURVE ( )  GEOMETRIC_REPRESENTATION_ITEM ( )  RATIONAL_B_SPLINE_CURVE ( ( 0.9755282581475768211, 0.9755282581475778203, 1.000000000000000000, 0.9510565162951535312, 1.000000000000000000, 0.9510565162951535312, 1.000000000000000000, 0.9510565162951535312, 1.000000000000000000, 0.9510565162951535312, 1.000000000000000000, 0.9755282581475768211, 0.9755282581475768211 ) ) 
 REPRESENTATION_ITEM ( '' )  );
#13699 = CARTESIAN_POINT ( 'NONE',  ( -1.778240108872766143E-15, 52.00000000546237544, -32.49999999999999289 ) ) ;
#13700 = CARTESIAN_POINT ( 'NONE',  ( -24.18731323226221974, 27.03347249907602290, 14.01125832528330406 ) ) ;
#13701 = CARTESIAN_POINT ( 'NONE',  ( 27.16883889988623935, 22.32500000273118701, -19.73931689729374384 ) ) ;
#13702 = CARTESIAN_POINT ( 'NONE',  ( -13.97622843553632421, 53.39322916666665009, -24.20753774853731599 ) ) ;
#13703 = VERTEX_POINT ( 'NONE', #6336 ) ;
#13704 = CARTESIAN_POINT ( 'NONE',  ( -33.58253175000000113, 57.22500000273117848, 10.91162601494193929 ) ) ;
#13705 = ORIENTED_EDGE ( 'NONE', *, *, #27503, .T. ) ;
#13706 = CARTESIAN_POINT ( 'NONE',  ( -15.01150461594595775, 28.18489583333332860, 26.00068869287368756 ) ) ;
#13707 = CARTESIAN_POINT ( 'NONE',  ( -28.00173670424549499, 23.46392333425730570, -7.543491769121417612 ) ) ;
#13708 = CARTESIAN_POINT ( 'NONE',  ( -10.37757302488624411, 2.725000002731181592, -31.93888565452638417 ) ) ;
#13709 = ORIENTED_EDGE ( 'NONE', *, *, #17076, .F. ) ;
#13710 = LINE ( 'NONE', #21106, #19063 ) ;
#13711 = CARTESIAN_POINT ( 'NONE',  ( 20.75514604977249178, 30.07500000273118701, 28.56700777964553950 ) ) ;
#13712 = CARTESIAN_POINT ( 'NONE',  ( -32.50000000000000000, 30.50000000546237899, 0.000000000000000000 ) ) ;
#13713 = CARTESIAN_POINT ( 'NONE',  ( -26.29305231718579350, 79.79999999999998295, -19.10302069950537884 ) ) ;
#13714 = CARTESIAN_POINT ( 'NONE',  ( 32.50000000000000000, 52.99999999999999289, -3.980102097228898626E-15 ) ) ;
#13715 = CARTESIAN_POINT ( 'NONE',  ( 9.270509831248421762, 73.29999999999996874, -12.75976212528059861 ) ) ;
#13716 = CARTESIAN_POINT ( 'NONE',  ( -10.37757302488623701, 43.77500000273118275, 31.93888565452638417 ) ) ;
#13717 = CARTESIAN_POINT ( 'NONE',  ( 26.29305231718578995, 61.20000000000000284, -19.10302069950538240 ) ) ;
#13718 =( LENGTH_UNIT ( ) NAMED_UNIT ( * ) SI_UNIT ( .MILLI., .METRE. ) );
#13719 = CARTESIAN_POINT ( 'NONE',  ( -20.08610463437156923, 22.29999999999999716, 27.64615127144130113 ) ) ;
#13720 = CARTESIAN_POINT ( 'NONE',  ( -32.50000000000000000, 22.09999999999999787, 10.55989012756946366 ) ) ;
#13721 = CARTESIAN_POINT ( 'NONE',  ( 15.14183272437242245, 12.29999999999999183, -20.84094480462497856 ) ) ;
#13722 = CARTESIAN_POINT ( 'NONE',  ( 33.58253175000000823, 60.02500000273116854, 10.91162601494192863 ) ) ;
#13723 = CARTESIAN_POINT ( 'NONE',  ( -15.14183272437242600, 5.049999994537627934, 20.84094480462497856 ) ) ;
#13724 = CARTESIAN_POINT ( 'NONE',  ( -10.37757302488624411, 54.97500000273119980, -31.93888565452638417 ) ) ;
#13725 = CARTESIAN_POINT ( 'NONE',  ( 1.507698388325705758E-15, 7.124999997268828267, -24.62258325217400312 ) ) ;
#13726 = CARTESIAN_POINT ( 'NONE',  ( 7.570916362186207671, 3.349999994537639303, 23.30088464923126779 ) ) ;
#13727 = CARTESIAN_POINT ( 'NONE',  ( -10.37757302488623701, 7.525000002731207616, 31.93888565452638417 ) ) ;
#13728 = CARTESIAN_POINT ( 'NONE',  ( -7.025853678916393008, 43.22954833425730925, 26.06988505166735592 ) ) ;
#13729 = CARTESIAN_POINT ( 'NONE',  ( 8.998893468610761559, 16.99999999999998579, -21.61938333025141290 ) ) ;
#13730 = CARTESIAN_POINT ( 'NONE',  ( -33.58253175000000113, 29.12500000273120193, 0.000000000000000000 ) ) ;
#13731 = CARTESIAN_POINT ( 'NONE',  ( -10.04305231718578462, 18.90000000546238113, 30.90933677959249337 ) ) ;
#13732 = CARTESIAN_POINT ( 'NONE',  ( 26.29305231718578995, 61.70000000546237118, -19.10302069950538240 ) ) ;
#13733 = CARTESIAN_POINT ( 'NONE',  ( 32.50000000000000711, 60.89999999999999147, 10.55989012756945122 ) ) ;
#13734 = CARTESIAN_POINT ( 'NONE',  ( -25.98046417659831420, 57.97097249907601935, 15.04653450569339945 ) ) ;
#13735 = CARTESIAN_POINT ( 'NONE',  ( 20.08610463437157279, 49.80000000546238681, -27.64615127144129758 ) ) ;
#13736 =( NAMED_UNIT ( * ) SI_UNIT ( $, .STERADIAN. ) SOLID_ANGLE_UNIT ( ) );
#13737 = CARTESIAN_POINT ( 'NONE',  ( 19.09188309203661049, 23.17187499999999289, -19.09188309203694445 ) ) ;
#13738 = EDGE_LOOP ( 'NONE', ( #5261, #28047, #31609, #5848 ) ) ;
#13739 = CARTESIAN_POINT ( 'NONE',  ( 33.58253175000000113, 74.12500000273118417, -4.112674001490185761E-15 ) ) ;
#13740 = CARTESIAN_POINT ( 'NONE',  ( -7.505752307972844761, 34.91666666666666430, 28.01184896238304134 ) ) ;
#13741 = CARTESIAN_POINT ( 'NONE',  ( 21.64573397815488676, 16.99999999999998579, 8.935324268693841887 ) ) ;
#13742 = ORIENTED_EDGE ( 'NONE', *, *, #16488, .T. ) ;
#13743 = CARTESIAN_POINT ( 'NONE',  ( 0.04044903254992426173, 41.36756916759064495, -30.02300923189239867 ) ) ;
#13744 = CARTESIAN_POINT ( 'NONE',  ( -32.50000000000000000, 16.50000000546238255, 0.000000000000000000 ) ) ;
#13745 = CARTESIAN_POINT ( 'NONE',  ( -7.505752307972844761, 48.66666666666666430, 28.01184896238304134 ) ) ;
#13746 = FACE_OUTER_BOUND ( 'NONE', #23918, .T. ) ;
#13747 = CARTESIAN_POINT ( 'NONE',  ( 20.75514604977249178, 50.07500000273120122, 28.56700777964553950 ) ) ;
#13748 = CARTESIAN_POINT ( 'NONE',  ( 10.04305231718579705, 49.10000000546238397, 30.90933677959248982 ) ) ;
#13749 = PRODUCT_DEFINITION_SHAPE ( 'NONE', 'NONE',  #8255 ) ;
#13750 = CARTESIAN_POINT ( 'NONE',  ( 2.688165632520823219E-15, 79.87500000273114154, 14.63369212191046387 ) ) ;
#13751 = CARTESIAN_POINT ( 'NONE',  ( -2.162160676586881955E-15, 32.62500000273119838, -35.31076352940723240 ) ) ;
#13752 = DIRECTION ( 'NONE',  ( 0.000000000000000000, 1.000000000000000000, 0.000000000000000000 ) ) ;
#13753 = CARTESIAN_POINT ( 'NONE',  ( 20.75514604977249178, 64.07500000273120122, 28.56700777964553950 ) ) ;
#13754 = CARTESIAN_POINT ( 'NONE',  ( 9.189759918205185230, 74.00000000000001421, 10.46186907115101938 ) ) ;
#13755 = CARTESIAN_POINT ( 'NONE',  ( -20.08610463437157989, 37.70000000000000995, -27.64615127144129758 ) ) ;
#13756 = CARTESIAN_POINT ( 'NONE',  ( 14.47279130897151767, 12.92499999726881832, -19.92008829642072598 ) ) ;
#13757 = CARTESIAN_POINT ( 'NONE',  ( 10.37757302488624056, 6.775000002731179194, -31.93888565452638417 ) ) ;
#13758 = CARTESIAN_POINT ( 'NONE',  ( -32.50000000000000000, 70.60000000546236265, 10.55989012756946366 ) ) ;
#13759 = AXIS2_PLACEMENT_3D ( 'NONE', #14008, #22356, #24922 ) ;
#13760 = CARTESIAN_POINT ( 'NONE',  ( -8.960552108402742093E-16, 74.87500000273116996, -14.63369212191046387 ) ) ;
#13761 = CARTESIAN_POINT ( 'NONE',  ( 33.58253175000000113, 70.47500000273119269, -10.91162601494193574 ) ) ;
#13762 = CARTESIAN_POINT ( 'NONE',  ( 0.000000000000000000, 80.00000000000001421, 0.000000000000000000 ) ) ;
#13763 = CARTESIAN_POINT ( 'NONE',  ( 6.486482029760649416E-15, 69.87500000273121259, 35.31076352940723240 ) ) ;
#13764 = EDGE_LOOP ( 'NONE', ( #3400, #7625, #24337, #26406 ) ) ;
#13765 = DIRECTION ( 'NONE',  ( -0.000000000000000000, -1.000000000000000000, -0.000000000000000000 ) ) ;
#13766 = CARTESIAN_POINT ( 'NONE',  ( 6.988114217768294445, 65.56770833333332860, 26.07999730980477437 ) ) ;
#13767 = CARTESIAN_POINT ( 'NONE',  ( 10.72870458603808785, -72.44024934668307480, 1.313887373028906799E-15 ) ) ;
#13768 = CARTESIAN_POINT ( 'NONE',  ( 10.37757302488624056, 44.52500000273119696, -31.93888565452638417 ) ) ;
#13769 = CARTESIAN_POINT ( 'NONE',  ( 27.16883889988623935, 12.57500000273119234, -19.73931689729374384 ) ) ;
#13770 = CARTESIAN_POINT ( 'NONE',  ( 20.75514604977249178, 64.07500000273120122, 28.56700777964553950 ) ) ;
#13771 = CARTESIAN_POINT ( 'NONE',  ( -26.07999730980477437, 52.67708333333333570, 6.988114217768305103 ) ) ;
#13772 = CARTESIAN_POINT ( 'NONE',  ( 26.02091320914851025, 28.19048583425731636, -14.97647472619946463 ) ) ;
#13773 = CARTESIAN_POINT ( 'NONE',  ( 30.02300923189239867, 32.47618083240936215, -0.04044903255044467877 ) ) ;
#13774 = CARTESIAN_POINT ( 'NONE',  ( 6.277390505771533514E-15, 73.00000000546239676, 34.17252228774368916 ) ) ;
#13775 = VECTOR ( 'NONE', #22675, 1000.000000000000000 ) ;
#13776 = EDGE_CURVE ( 'NONE', #6044, #33570, #33528, .T. ) ;
#13777 = CARTESIAN_POINT ( 'NONE',  ( -8.601468415847518756, 78.57500000273120122, -11.83890561707634781 ) ) ;
#13778 = CARTESIAN_POINT ( 'NONE',  ( 33.58253175000000823, 42.02500000273118985, 10.91162601494192685 ) ) ;
#13779 = CARTESIAN_POINT ( 'NONE',  ( -19.11951029504797006, 44.93711833240935505, -19.06425588902558133 ) ) ;
#13780 = CARTESIAN_POINT ( 'NONE',  ( 14.47279130897151589, 18.32499999726882578, 19.92008829642072953 ) ) ;
#13781 = CARTESIAN_POINT ( 'NONE',  ( 5.147494310547426899, 59.44874571845315359, -32.50000000000000000 ) ) ;
#13782 = EDGE_LOOP ( 'NONE', ( #29371, #30134, #29565, #9937 ) ) ;
#13783 = CARTESIAN_POINT ( 'NONE',  ( 33.58253175000000113, 48.37500000273119127, -4.112674001490185761E-15 ) ) ;
#13784 = CARTESIAN_POINT ( 'NONE',  ( 0.000000000000000000, 80.00000000000001421, -32.50000000000000000 ) ) ;
#13785 = VECTOR ( 'NONE', #20658, 1000.000000000000000 ) ;
#13786 = CARTESIAN_POINT ( 'NONE',  ( 26.06988505166735592, 52.68267333425730214, 7.025853678916393896 ) ) ;
#13787 = CARTESIAN_POINT ( 'NONE',  ( -33.58253175000000113, 71.27500000273118985, -10.91162601494193218 ) ) ;
#13788 = VERTEX_POINT ( 'NONE', #13572 ) ;
#13789 = CARTESIAN_POINT ( 'NONE',  ( -27.16883889988624290, 14.92500000273118488, -19.73931689729374028 ) ) ;
#13790 = EDGE_CURVE ( 'NONE', #18447, #9615, #3072, .T. ) ;
#13791 = CARTESIAN_POINT ( 'NONE',  ( 7.505752307972854531, 22.88541666666666430, -28.01184896238303423 ) ) ;
#13792 = VERTEX_POINT ( 'NONE', #19055 ) ;
#13793 =( BOUNDED_CURVE ( )  B_SPLINE_CURVE ( 2, ( #30797, #33018, #22568, #6781, #33374, #4719, #27722, #1453, #9869, #17259, #4210, #28062, #14682 ),
 .UNSPECIFIED., .F., .T. ) 
 B_SPLINE_CURVE_WITH_KNOTS ( ( 3, 2, 2, 2, 2, 2, 3 ),
 ( 0.7243589743589743390, 0.7256410256410256165, 0.7282051282051281715, 0.7307692307692307265, 0.7333333333333332815, 0.7358974358974359475, 0.7371794871794872250 ),
 .UNSPECIFIED. ) 
 CURVE ( )  GEOMETRIC_REPRESENTATION_ITEM ( )  RATIONAL_B_SPLINE_CURVE ( ( 0.9755282581475768211, 0.9755282581475768211, 1.000000000000000000, 0.9510565162951535312, 1.000000000000000000, 0.9510565162951535312, 1.000000000000000000, 0.9510565162951535312, 1.000000000000000000, 0.9510565162951535312, 1.000000000000000000, 0.9755282581475768211, 0.9755282581475768211 ) ) 
 REPRESENTATION_ITEM ( '' )  );
#13794 = ORIENTED_EDGE ( 'NONE', *, *, #2759, .T. ) ;
#13795 = CARTESIAN_POINT ( 'NONE',  ( -5.147494310547430452, 48.05125428700922185, -32.49999999999999289 ) ) ;
#13796 = CARTESIAN_POINT ( 'NONE',  ( 10.37757302488624056, 56.52500000273119696, -31.93888565452638417 ) ) ;
#13797 = CARTESIAN_POINT ( 'NONE',  ( -26.00068869287368756, 59.98177083333332149, -15.01150461594595775 ) ) ;
#13798 = CARTESIAN_POINT ( 'NONE',  ( -20.08610463437156923, 20.80000000546236549, 27.64615127144130113 ) ) ;
#13799 = CARTESIAN_POINT ( 'NONE',  ( -5.147494310547377161, 66.05125428700922896, -32.50000000000002132 ) ) ;
#13800 = CARTESIAN_POINT ( 'NONE',  ( 23.41746824999999887, 11.12499999726881938, 0.000000000000000000 ) ) ;
#13801 = CARTESIAN_POINT ( 'NONE',  ( 33.58253175000000113, 22.37500000273118417, -4.112674001490185761E-15 ) ) ;
#13802 =( NAMED_UNIT ( * ) PLANE_ANGLE_UNIT ( ) SI_UNIT ( $, .RADIAN. ) );
#13803 = CARTESIAN_POINT ( 'NONE',  ( 27.95245687107223276, 15.28868083240935505, -0.04044903255042905932 ) ) ;
#13804 = CARTESIAN_POINT ( 'NONE',  ( -11.25946833292375793, 79.07500000273121543, 8.180482586598737171 ) ) ;
#13805 = CARTESIAN_POINT ( 'NONE',  ( -1.778240108872766143E-15, 28.00000000546237544, -32.49999999999999289 ) ) ;
#13806 = CARTESIAN_POINT ( 'NONE',  ( 32.50000000000000000, 9.100000000000004974, -10.55989012756945833 ) ) ;
#13807 = ORIENTED_EDGE ( 'NONE', *, *, #33913, .T. ) ;
#13808 = CARTESIAN_POINT ( 'NONE',  ( -4.732186688966233175E-15, 17.24999999453762101, 25.76082449383753925 ) ) ;
#13809 = CARTESIAN_POINT ( 'NONE',  ( -4.300734207923759378, 78.47500000273119269, -13.23629886949340495 ) ) ;
#13810 = CARTESIAN_POINT ( 'NONE',  ( 27.95245687107222921, 30.47656250000000355, -2.463307335887066074E-13 ) ) ;
#13811 = CARTESIAN_POINT ( 'NONE',  ( -33.58253175000000113, 23.12500000273118417, 0.000000000000000000 ) ) ;
#13812 = CARTESIAN_POINT ( 'NONE',  ( -27.16883889988624290, 74.92500000273120975, -19.73931689729374028 ) ) ;
#13813 = CIRCLE ( 'NONE', #15459, 10.64101615137753676 ) ;
#13814 = CARTESIAN_POINT ( 'NONE',  ( 6.486482029760649416E-15, 29.87500000273119838, 35.31076352940723240 ) ) ;
#13815 = CARTESIAN_POINT ( 'NONE',  ( 33.58253175000000113, 16.37500000273119127, -4.112674001490185761E-15 ) ) ;
#13816 = CARTESIAN_POINT ( 'NONE',  ( -20.75514604977248112, 13.67500000273118310, 28.56700777964554661 ) ) ;
#13817 = CARTESIAN_POINT ( 'NONE',  ( 0.04044903254993986036, 58.55506916759063785, -27.95245687107223986 ) ) ;
#13818 = CARTESIAN_POINT ( 'NONE',  ( -10.37757302488623701, 69.52500000273120406, 31.93888565452638417 ) ) ;
#13819 = DIRECTION ( 'NONE',  ( 0.000000000000000000, 0.000000000000000000, -1.000000000000000000 ) ) ;
#13820 = CARTESIAN_POINT ( 'NONE',  ( -11.25946833292375793, 77.57500000273121543, 8.180482586598737171 ) ) ;
#13821 = CARTESIAN_POINT ( 'NONE',  ( 32.50000000000000000, 53.00000000000000711, -3.980102097228898626E-15 ) ) ;
#13822 = DIRECTION ( 'NONE',  ( 0.000000000000000000, 0.000000000000000000, -1.000000000000000000 ) ) ;
#13823 = CARTESIAN_POINT ( 'NONE',  ( -33.58253175000000113, 61.22500000273119269, 10.91162601494193929 ) ) ;
#13824 = CARTESIAN_POINT ( 'NONE',  ( 23.41746825000000243, 13.22499999726881192, -7.608796670333727974 ) ) ;
#13825 = ORIENTED_EDGE ( 'NONE', *, *, #16600, .T. ) ;
#13826 = CARTESIAN_POINT ( 'NONE',  ( -33.58253175000000113, 69.37500000273121259, 0.000000000000000000 ) ) ;
#13827 = CARTESIAN_POINT ( 'NONE',  ( -33.58253175000000113, 3.025000002731199622, -10.91162601494193041 ) ) ;
#13828 = CARTESIAN_POINT ( 'NONE',  ( -18.94512977948575738, 9.424999997268812990, -13.76444248337723231 ) ) ;
#13829 = CARTESIAN_POINT ( 'NONE',  ( 7.025853678916403666, 20.88579833425730925, -26.06988505166735237 ) ) ;
#13830 = ORIENTED_EDGE ( 'NONE', *, *, #7366, .T. ) ;
#13831 = CARTESIAN_POINT ( 'NONE',  ( -33.58253175000000113, 37.22500000273119980, 10.91162601494193929 ) ) ;
#13832 = CARTESIAN_POINT ( 'NONE',  ( -32.50000000000000000, 42.60000000546236976, 10.55989012756946366 ) ) ;
#13833 = ORIENTED_EDGE ( 'NONE', *, *, #32348, .F. ) ;
#13834 = CARTESIAN_POINT ( 'NONE',  ( 26.00068869287367335, 47.95052083333331439, 15.01150461594596308 ) ) ;
#13835 = CARTESIAN_POINT ( 'NONE',  ( 20.75514604977248467, 66.67500000273119554, -28.56700777964554305 ) ) ;
#13836 = DIRECTION ( 'NONE',  ( 0.000000000000000000, 0.000000000000000000, 1.000000000000000000 ) ) ;
#13837 = CARTESIAN_POINT ( 'NONE',  ( -10.37757302488623701, 75.52500000273118985, 31.93888565452638417 ) ) ;
#13838 = CARTESIAN_POINT ( 'NONE',  ( 20.50609665441005092, 17.15624999999999645, 20.50609665440969209 ) ) ;
#13839 = CARTESIAN_POINT ( 'NONE',  ( -19.82091636218621389, 3.200000000000008171, 14.40073868116558842 ) ) ;
#13840 = CARTESIAN_POINT ( 'NONE',  ( 20.75514604977249178, 12.07500000273120655, 28.56700777964553950 ) ) ;
#13841 = EDGE_CURVE ( 'NONE', #14813, #24433, #641, .T. ) ;
#13842 = CARTESIAN_POINT ( 'NONE',  ( -10.37757302488623701, 13.52500000273118630, 31.93888565452638417 ) ) ;
#13843 = CARTESIAN_POINT ( 'NONE',  ( -13.91746824999999532, 78.77500000273117564, -4.522059556121115875 ) ) ;
#13844 = CARTESIAN_POINT ( 'NONE',  ( -40.00000000000000711, 52.00000000000000711, -23.09401076758504345 ) ) ;
#13845 = CARTESIAN_POINT ( 'NONE',  ( -25.98046417659831420, 47.65847249907603356, 15.04653450569339945 ) ) ;
#13846 = CARTESIAN_POINT ( 'NONE',  ( -15.00000000000000000, 77.90000000000001990, -4.873795443493594171 ) ) ;
#13847 = CARTESIAN_POINT ( 'NONE',  ( -28.01184896238304134, 49.52604166666666430, -7.505752307972844761 ) ) ;
#13848 = EDGE_CURVE ( 'NONE', #390, #1865, #14234, .T. ) ;
#13849 = DIRECTION ( 'NONE',  ( 0.000000000000000000, 0.000000000000000000, -1.000000000000000000 ) ) ;
#13850 = CARTESIAN_POINT ( 'NONE',  ( -1.778240108872766143E-15, 50.00000000546237544, -32.49999999999999289 ) ) ;
#13851 = CARTESIAN_POINT ( 'NONE',  ( -24.18731323226221974, 57.97097249907601935, 14.01125832528330406 ) ) ;
#13852 = CARTESIAN_POINT ( 'NONE',  ( 27.16883889988624290, 43.92500000273119554, 19.73931689729373673 ) ) ;
#13853 = CARTESIAN_POINT ( 'NONE',  ( 9.270509831248425314, 72.95000000546238539, 12.75976212528059683 ) ) ;
#13854 = CARTESIAN_POINT ( 'NONE',  ( -10.37757302488624411, 46.97500000273117848, -31.93888565452638417 ) ) ;
#13855 = CARTESIAN_POINT ( 'NONE',  ( 6.486482029760648627E-15, 37.87500000273117706, 35.31076352940722529 ) ) ;
#13856 = CARTESIAN_POINT ( 'NONE',  ( -9.065058954415986747, 16.99999999999998579, 22.60608526228350357 ) ) ;
#13857 = AXIS2_PLACEMENT_3D ( 'NONE', #21854, #13463, #32136 ) ;
#13858 = CARTESIAN_POINT ( 'NONE',  ( 24.20753774853731244, 19.87760416666666430, -13.97622843553633132 ) ) ;
#13859 = CARTESIAN_POINT ( 'NONE',  ( 24.50000000000000000, 11.84999999453761710, -7.960532557706203605 ) ) ;
#13860 = LINE ( 'NONE', #11604, #10194 ) ;
#13861 = CARTESIAN_POINT ( 'NONE',  ( -20.08610463437157989, 75.69999999999998863, -27.64615127144129758 ) ) ;
#13862 = CARTESIAN_POINT ( 'NONE',  ( 10.37757302488624056, 8.525000002731195181, -31.93888565452638417 ) ) ;
#13863 = CARTESIAN_POINT ( 'NONE',  ( -14.47279130897151767, 5.324999997268798246, -19.92008829642072598 ) ) ;
#13864 = CARTESIAN_POINT ( 'NONE',  ( 3.880418787951140036, 12.44874571845315714, -24.49999999999999645 ) ) ;
#13865 = CARTESIAN_POINT ( 'NONE',  ( -14.01125832528328985, 24.45534749907602290, -24.18731323226223040 ) ) ;
#13866 = CARTESIAN_POINT ( 'NONE',  ( -32.50000000000000000, 65.89999999999999147, -10.55989012756945300 ) ) ;
#13867 = CARTESIAN_POINT ( 'NONE',  ( 10.37757302488624767, 21.72500000273119980, 31.93888565452638417 ) ) ;
#13868 = CARTESIAN_POINT ( 'NONE',  ( 14.47279130897151767, 5.424999997268823648, -19.92008829642072598 ) ) ;
#13869 = CARTESIAN_POINT ( 'NONE',  ( 19.09188309203661049, 57.54687500000000000, -19.09188309203694445 ) ) ;
#13870 = ORIENTED_EDGE ( 'NONE', *, *, #1325, .F. ) ;
#13871 = CARTESIAN_POINT ( 'NONE',  ( 27.16883889988623935, 56.32500000273120122, -19.73931689729374384 ) ) ;
#13872 = EDGE_LOOP ( 'NONE', ( #32606, #3895, #23668, #12040 ) ) ;
#13873 = CARTESIAN_POINT ( 'NONE',  ( 28.01184896238304134, 23.74479166666666430, 7.505752307972846538 ) ) ;
#13874 = CARTESIAN_POINT ( 'NONE',  ( 25.98046417659858420, 21.88840250092397710, 15.04653450569292872 ) ) ;
#13875 = VECTOR ( 'NONE', #12846, 1000.000000000000000 ) ;
#13876 = CARTESIAN_POINT ( 'NONE',  ( 26.29305231718578995, 39.20000000000000995, -19.10302069950538240 ) ) ;
#13877 = AXIS2_PLACEMENT_3D ( 'NONE', #8842, #19325, #30101 ) ;
#13878 = CARTESIAN_POINT ( 'NONE',  ( -23.41746824999999887, 7.624999997268816720, -2.867812753649727150E-15 ) ) ;
#13879 = CARTESIAN_POINT ( 'NONE',  ( -10.37757302488623701, 27.77500000273119696, 31.93888565452638417 ) ) ;
#13880 = CARTESIAN_POINT ( 'NONE',  ( 10.04305231718578817, 33.90000000546239534, -30.90933677959249337 ) ) ;
#13881 = ADVANCED_FACE ( 'NONE', ( #25028 ), #30677, .T. ) ;
#13882 = CARTESIAN_POINT ( 'NONE',  ( 10.04305231718579705, 76.59999999999999432, 30.90933677959248982 ) ) ;
#13883 = CARTESIAN_POINT ( 'NONE',  ( 10.04305231718578817, 33.90000000546239534, -30.90933677959249337 ) ) ;
#13884 = CARTESIAN_POINT ( 'NONE',  ( 2.375766604868046361, 72.55125428154683220, 14.99999999999999822 ) ) ;
#13885 = CARTESIAN_POINT ( 'NONE',  ( 33.58253175000000113, 44.47500000273119269, -10.91162601494193751 ) ) ;
#13886 = EDGE_CURVE ( 'NONE', #27323, #30686, #12330, .T. ) ;
#13887 = CARTESIAN_POINT ( 'NONE',  ( -10.04305231718578462, 22.39999999999998792, 30.90933677959249337 ) ) ;
#13888 = CARTESIAN_POINT ( 'NONE',  ( 32.50000000000000711, 22.90000000000000568, 10.55989012756945122 ) ) ;
#13889 = CARTESIAN_POINT ( 'NONE',  ( 15.14183272437241889, 11.70000000000000995, 20.84094480462498211 ) ) ;
#13890 = CARTESIAN_POINT ( 'NONE',  ( 33.58253175000000113, 66.22500000273120691, -10.91162601494193751 ) ) ;
#13891 = CARTESIAN_POINT ( 'NONE',  ( 33.58253175000000823, 56.27500000273117564, 10.91162601494192685 ) ) ;
#13892 = CARTESIAN_POINT ( 'NONE',  ( -23.41746824999999887, 13.62499999726882116, -2.867812753649727150E-15 ) ) ;
#13893 = CARTESIAN_POINT ( 'NONE',  ( -24.50000000000000000, 16.99999999999998579, -3.000384657911015469E-15 ) ) ;
#13894 = CARTESIAN_POINT ( 'NONE',  ( 20.75514604977249178, 3.825000002731174575, 28.56700777964553950 ) ) ;
#13895 = CARTESIAN_POINT ( 'NONE',  ( 24.18731323226247554, 35.63840250092398065, 14.01125832528285997 ) ) ;
#13896 = CARTESIAN_POINT ( 'NONE',  ( 31.92269207768545058, 66.99999999999998579, -6.710300343870453155 ) ) ;
#13897 = CARTESIAN_POINT ( 'NONE',  ( 7.570916362186213000, 2.149999994537632464, -23.30088464923126423 ) ) ;
#13898 = CARTESIAN_POINT ( 'NONE',  ( 6.486482029760649416E-15, 27.62500000273118062, 35.31076352940723240 ) ) ;
#13899 = DIRECTION ( 'NONE',  ( -0.000000000000000000, 1.000000000000000000, -0.000000000000000000 ) ) ;
#13900 = CARTESIAN_POINT ( 'NONE',  ( -4.223320258572819786E-15, 15.24999999453762278, 24.50000000000000000 ) ) ;
#13901 = VECTOR ( 'NONE', #9074, 1000.000000000000000 ) ;
#13902 = LINE ( 'NONE', #24693, #25822 ) ;
#13903 = CARTESIAN_POINT ( 'NONE',  ( 20.47846945139867003, 52.67149333240935505, -20.53372385742107653 ) ) ;
#13904 = CARTESIAN_POINT ( 'NONE',  ( 32.50000000000000000, 47.60000000546239818, -10.55989012756945833 ) ) ;
#13905 = CARTESIAN_POINT ( 'NONE',  ( -13.91746824999999532, 73.27500000273118985, -4.522059556121115875 ) ) ;
#13906 = CARTESIAN_POINT ( 'NONE',  ( -7.570916362186210335, 16.60000000000000497, -23.30088464923126779 ) ) ;
#13907 = CARTESIAN_POINT ( 'NONE',  ( 27.95245687107222921, 23.60156250000000000, -2.463307335887066074E-13 ) ) ;
#13908 = CARTESIAN_POINT ( 'NONE',  ( -20.75514604977248823, 76.82500000273120122, -28.56700777964554305 ) ) ;
#13909 = CARTESIAN_POINT ( 'NONE',  ( 7.505752307973351023, 31.19270833333333215, 28.01184896238290278 ) ) ;
#13910 = FACE_OUTER_BOUND ( 'NONE', #25813, .T. ) ;
#13911 = ORIENTED_EDGE ( 'NONE', *, *, #21409, .F. ) ;
#13912 = CARTESIAN_POINT ( 'NONE',  ( -30.02300923189239867, 50.82069416759063785, -0.04044903254991731589 ) ) ;
#13913 = CARTESIAN_POINT ( 'NONE',  ( 32.50000000000000000, 17.50000000546238255, -3.980102097228898626E-15 ) ) ;
#13914 = CARTESIAN_POINT ( 'NONE',  ( 20.50609665441005092, 54.96875000000000000, 20.50609665440969209 ) ) ;
#13915 = DIRECTION ( 'NONE',  ( 0.000000000000000000, 0.000000000000000000, -1.000000000000000000 ) ) ;
#13916 = CARTESIAN_POINT ( 'NONE',  ( 33.58253175000000113, 46.37500000273120548, -4.112674001490185761E-15 ) ) ;
#13917 = CARTESIAN_POINT ( 'NONE',  ( 32.50000000000000000, 51.50000000546239676, -3.980102097228898626E-15 ) ) ;
#13918 = CARTESIAN_POINT ( 'NONE',  ( -8.960552108402742093E-16, 78.87500000273118417, -14.63369212191046387 ) ) ;
#13919 = CARTESIAN_POINT ( 'NONE',  ( 33.58253175000000113, 38.12500000273119838, -4.112674001490185761E-15 ) ) ;
#13920 = DIRECTION ( 'NONE',  ( 1.000000000000000000, 0.000000000000000000, 0.000000000000000000 ) ) ;
#13921 = VECTOR ( 'NONE', #30850, 1000.000000000000000 ) ;
#13922 = CARTESIAN_POINT ( 'NONE',  ( -10.37757302488624411, 60.97500000273120691, -31.93888565452638417 ) ) ;
#13923 = AXIS2_PLACEMENT_3D ( 'NONE', #13257, #10351, #23224 ) ;
#13924 = CARTESIAN_POINT ( 'NONE',  ( -26.29305231718578995, 40.20000000000001705, 19.10302069950538595 ) ) ;
#13925 = CARTESIAN_POINT ( 'NONE',  ( -14.47279130897152122, 13.92499999726881654, 19.92008829642072243 ) ) ;
#13926 = CARTESIAN_POINT ( 'NONE',  ( 33.58253175000000113, 6.475000002731178483, -10.91162601494193751 ) ) ;
#13927 = CARTESIAN_POINT ( 'NONE',  ( 5.147494310547434893, 12.55125428154683753, 32.49999999999999289 ) ) ;
#13928 = CARTESIAN_POINT ( 'NONE',  ( -13.91746824999999887, 71.37500000273119838, 0.000000000000000000 ) ) ;
#13929 = CARTESIAN_POINT ( 'NONE',  ( 33.58253175000000113, 74.47500000273117848, -10.91162601494193574 ) ) ;
#13930 = CARTESIAN_POINT ( 'NONE',  ( -3.880418787951124493, 5.448745718453149145, 24.50000000000000355 ) ) ;
#13931 = CARTESIAN_POINT ( 'NONE',  ( -33.58253175000000113, 67.27500000273117564, -10.91162601494193218 ) ) ;
#13932 = VERTEX_POINT ( 'NONE', #14908 ) ;
#13933 = CARTESIAN_POINT ( 'NONE',  ( 19.82091636218621389, 1.949999994537626735, -14.40073868116559197 ) ) ;
#13934 = CARTESIAN_POINT ( 'NONE',  ( 19.06425588902592239, 11.71913166759064318, 19.11951029504763611 ) ) ;
#13935 = CARTESIAN_POINT ( 'NONE',  ( -1.778240108872766143E-15, 43.50000000000000000, -32.49999999999999289 ) ) ;
#13936 = CARTESIAN_POINT ( 'NONE',  ( -33.58253175000000113, 47.22500000273117138, 10.91162601494193929 ) ) ;
#13937 = CARTESIAN_POINT ( 'NONE',  ( -27.16883889988624290, 11.17500000273118133, -19.73931689729374028 ) ) ;
#13938 = CARTESIAN_POINT ( 'NONE',  ( 33.58253175000000113, 62.37500000273120548, -4.112674001490185761E-15 ) ) ;
#13939 = CARTESIAN_POINT ( 'NONE',  ( -6.988114217767819270, 52.10416666666666430, 26.07999730980490583 ) ) ;
#13940 = CARTESIAN_POINT ( 'NONE',  ( -15.04653450569291984, 43.37277750092397355, 25.98046417659859486 ) ) ;
#13941 = CARTESIAN_POINT ( 'NONE',  ( -14.97647472619899389, 26.74701416574268720, 26.02091320914878025 ) ) ;
#13942 = CARTESIAN_POINT ( 'NONE',  ( 32.50000000000000711, 67.40000000546237402, 10.55989012756945122 ) ) ;
#13943 =( GEOMETRIC_REPRESENTATION_CONTEXT ( 3 ) GLOBAL_UNCERTAINTY_ASSIGNED_CONTEXT ( ( #24689 ) ) GLOBAL_UNIT_ASSIGNED_CONTEXT ( ( #5485, #21286, #24019 ) ) REPRESENTATION_CONTEXT ( 'NONE', 'WORKASPACE' ) );
#13944 = CARTESIAN_POINT ( 'NONE',  ( 2.688165632520823219E-15, 79.37500000273116996, 14.63369212191046387 ) ) ;
#13945 = CARTESIAN_POINT ( 'NONE',  ( -7.025853678916861966, 58.97357666574269786, -26.06988505166722803 ) ) ;
#13946 = CARTESIAN_POINT ( 'NONE',  ( 7.236395654485755280, 14.22499999726881192, 22.27133577429736988 ) ) ;
#13947 = DIRECTION ( 'NONE',  ( 0.000000000000000000, 0.000000000000000000, -1.000000000000000000 ) ) ;
#13948 = VERTEX_POINT ( 'NONE', #22130 ) ;
#13949 = CARTESIAN_POINT ( 'NONE',  ( -27.16883889988623935, 47.57500000273119412, 19.73931689729374739 ) ) ;
#13950 = CARTESIAN_POINT ( 'NONE',  ( -4.223320258572819786E-15, 5.249999994537629888, 24.50000000000000000 ) ) ;
#13951 = CARTESIAN_POINT ( 'NONE',  ( -26.09010956794232428, 54.11496500092397355, 6.950374756619732253 ) ) ;
#13952 = CARTESIAN_POINT ( 'NONE',  ( 6.486482029760649416E-15, 69.87500000273121259, 35.31076352940723240 ) ) ;
#13953 = ORIENTED_EDGE ( 'NONE', *, *, #20502, .F. ) ;
#13954 = CARTESIAN_POINT ( 'NONE',  ( 27.16883889988624290, 19.92500000273118843, 19.73931689729373673 ) ) ;
#13955 = CARTESIAN_POINT ( 'NONE',  ( -20.50609665441004736, 25.74999999999999645, -20.50609665440969565 ) ) ;
#13956 = ORIENTED_EDGE ( 'NONE', *, *, #846, .T. ) ;
#13957 = DIRECTION ( 'NONE',  ( 0.000000000000000000, 0.000000000000000000, -1.000000000000000000 ) ) ;
#13958 = CARTESIAN_POINT ( 'NONE',  ( -27.16883889988623935, 53.32500000273118701, 19.73931689729374739 ) ) ;
#13959 = CARTESIAN_POINT ( 'NONE',  ( 15.01150461594643204, 55.11197916666664298, 26.00068869287340334 ) ) ;
#13960 = CARTESIAN_POINT ( 'NONE',  ( -10.04305231718578462, 14.90000000546237757, 30.90933677959249337 ) ) ;
#13961 = CARTESIAN_POINT ( 'NONE',  ( 19.82091636218621389, 15.94999999453763984, -14.40073868116559197 ) ) ;
#13962 = CARTESIAN_POINT ( 'NONE',  ( 1.507698388325705758E-15, 17.62499999726881938, -24.62258325217400312 ) ) ;
#13963 = PRESENTATION_LAYER_ASSIGNMENT (  '', '', ( #28758 ) ) ;
#13964 = CARTESIAN_POINT ( 'NONE',  ( 20.75514604977249178, 26.07500000273119767, 28.56700777964553950 ) ) ;
#13965 = CARTESIAN_POINT ( 'NONE',  ( 7.025853678916867295, 16.00482666574268720, 26.06988505166722803 ) ) ;
#13966 = FACE_OUTER_BOUND ( 'NONE', #7081, .T. ) ;
#13967 = CARTESIAN_POINT ( 'NONE',  ( 7.428728520588063561E-18, -23.06066017177981564, 0.000000000000000000 ) ) ;
#13968 = EDGE_CURVE ( 'NONE', #6049, #16699, #20061, .T. ) ;
#13969 = CARTESIAN_POINT ( 'NONE',  ( -26.29305231718579350, 7.800000000000014921, -19.10302069950537884 ) ) ;
#13970 = VERTEX_POINT ( 'NONE', #25372 ) ;
#13971 = CARTESIAN_POINT ( 'NONE',  ( -24.50000000000000355, 16.64999999453763735, -7.960532557706207157 ) ) ;
#13972 = CARTESIAN_POINT ( 'NONE',  ( -13.91746824999999532, 74.97500000273115006, 4.522059556121122093 ) ) ;
#13973 = CARTESIAN_POINT ( 'NONE',  ( -19.09188309203694445, 39.49999999999999289, -19.09188309203661049 ) ) ;
#13974 = CARTESIAN_POINT ( 'NONE',  ( 6.486482029760649416E-15, 25.62500000273118772, 35.31076352940723240 ) ) ;
#13975 = CARTESIAN_POINT ( 'NONE',  ( 33.58253175000000113, 66.12500000273118417, -4.112674001490185761E-15 ) ) ;
#13976 = CARTESIAN_POINT ( 'NONE',  ( 20.75514604977249178, 30.07500000273118701, 28.56700777964553950 ) ) ;
#13977 = CARTESIAN_POINT ( 'NONE',  ( 33.58253175000000823, 18.27500000273118275, 10.91162601494192863 ) ) ;
#13978 = CARTESIAN_POINT ( 'NONE',  ( 27.16883889988624290, 8.175000002731191984, 19.73931689729373673 ) ) ;
#13979 = CARTESIAN_POINT ( 'NONE',  ( -24.22776226481240514, 64.28423583425730214, 13.94119854578937812 ) ) ;
#13980 = ADVANCED_FACE ( 'NONE', ( #1851, #4094 ), #27777, .T. ) ;
#13981 = CARTESIAN_POINT ( 'NONE',  ( -2.162160676586882350E-15, 70.62500000273118417, -35.31076352940722529 ) ) ;
#13982 = CARTESIAN_POINT ( 'NONE',  ( 7.505752307972854531, 57.26041666666666430, -28.01184896238303423 ) ) ;
#13983 = CARTESIAN_POINT ( 'NONE',  ( 0.000000000000000000, 102.0000000000000284, 14.00000000000000178 ) ) ;
#13984 = CARTESIAN_POINT ( 'NONE',  ( -13.91746824999999887, 75.37500000273116996, 0.000000000000000000 ) ) ;
#13985 = CARTESIAN_POINT ( 'NONE',  ( -2.092463501923844636E-15, 47.49999999999997868, -34.17252228774368916 ) ) ;
#13986 = CARTESIAN_POINT ( 'NONE',  ( -2.375766604868041476, 72.69874572391553613, 14.99999999999999822 ) ) ;
#13987 = CARTESIAN_POINT ( 'NONE',  ( 10.37757302488624767, 51.72500000273119980, 31.93888565452638417 ) ) ;
#13988 = CARTESIAN_POINT ( 'NONE',  ( -14.47279130897151589, 13.82499999726882045, -19.92008829642072598 ) ) ;
#13989 = ADVANCED_FACE ( 'NONE', ( #1165 ), #9441, .F. ) ;
#13990 = ORIENTED_EDGE ( 'NONE', *, *, #28667, .F. ) ;
#13991 = CARTESIAN_POINT ( 'NONE',  ( -27.16883889988624290, 69.17500000273118133, -19.73931689729374028 ) ) ;
#13992 =( BOUNDED_CURVE ( )  B_SPLINE_CURVE ( 2, ( #4946, #2891, #7860, #26231, #18350, #28622, #15604, #23321, #31539, #15254, #7693, #7347, #28289 ),
 .UNSPECIFIED., .F., .T. ) 
 B_SPLINE_CURVE_WITH_KNOTS ( ( 3, 2, 2, 2, 2, 2, 3 ),
 ( 0.5833333333333333703, 0.5888888888888889062, 0.5999999999999999778, 0.6111111111111111605, 0.6222222222222222321, 0.6333333333333333037, 0.6388888888888889506 ),
 .UNSPECIFIED. ) 
 CURVE ( )  GEOMETRIC_REPRESENTATION_ITEM ( )  RATIONAL_B_SPLINE_CURVE ( ( 0.9755282581475768211, 0.9755282581475770431, 1.000000000000000000, 0.9510565162951535312, 1.000000000000000000, 0.9510565162951535312, 1.000000000000000000, 0.9510565162951535312, 1.000000000000000000, 0.9510565162951535312, 1.000000000000000000, 0.9755282581475765991, 0.9755282581475768211 ) ) 
 REPRESENTATION_ITEM ( '' )  );
#13993 = CARTESIAN_POINT ( 'NONE',  ( 0.000000000000000000, 16.99999999999998579, 0.000000000000000000 ) ) ;
#13994 = CARTESIAN_POINT ( 'NONE',  ( -23.41746825000000243, 5.524999997268821517, -7.608796670333730638 ) ) ;
#13995 = CARTESIAN_POINT ( 'NONE',  ( -6.950374756619716266, 20.59934000092397355, -26.09010956794232428 ) ) ;
#13996 = VERTEX_POINT ( 'NONE', #19554 ) ;
#13997 = CARTESIAN_POINT ( 'NONE',  ( 33.58253175000000113, 38.22500000273119269, -10.91162601494193751 ) ) ;
#13998 = ORIENTED_EDGE ( 'NONE', *, *, #427, .T. ) ;
#13999 = CARTESIAN_POINT ( 'NONE',  ( -28.01184896238290278, 49.23958333333332860, 7.505752307973363457 ) ) ;
#14000 = CARTESIAN_POINT ( 'NONE',  ( 6.486482029760649416E-15, 61.87500000273117706, 35.31076352940723240 ) ) ;
#14001 = CARTESIAN_POINT ( 'NONE',  ( 10.04305231718578817, 69.90000000546237402, -30.90933677959249337 ) ) ;
#14002 = CARTESIAN_POINT ( 'NONE',  ( -33.58253175000000113, 71.22500000273117848, 10.91162601494193929 ) ) ;
#14003 = CARTESIAN_POINT ( 'NONE',  ( 20.50609665441005092, 34.34374999999999289, 20.50609665440969209 ) ) ;
#14004 = CARTESIAN_POINT ( 'NONE',  ( -15.14183272437242600, 9.299999999999998934, 20.84094480462497856 ) ) ;
#14005 = CARTESIAN_POINT ( 'NONE',  ( 33.58253175000000113, 6.475000002731178483, -10.91162601494193751 ) ) ;
#14006 = CARTESIAN_POINT ( 'NONE',  ( -10.37757302488624411, 18.72500000273119625, -31.93888565452638417 ) ) ;
#14007 = CARTESIAN_POINT ( 'NONE',  ( 11.25946833292375793, 73.67500000273119554, 8.180482586598731842 ) ) ;
#14008 = CARTESIAN_POINT ( 'NONE',  ( 0.000000000000000000, 82.00000000000001421, 0.000000000000000000 ) ) ;
#14009 = CARTESIAN_POINT ( 'NONE',  ( 28.02196122052058413, 39.49440999907601224, 7.468012846824272799 ) ) ;
#14010 = CARTESIAN_POINT ( 'NONE',  ( -4.635254915624211769, 77.60000000000000853, -14.26584774442730286 ) ) ;
#14011 = CARTESIAN_POINT ( 'NONE',  ( 28.01184896238304134, 47.80729166666666430, 7.505752307972846538 ) ) ;
#14012 = FACE_OUTER_BOUND ( 'NONE', #11252, .T. ) ;
#14013 = CARTESIAN_POINT ( 'NONE',  ( -1.778240108872766143E-15, 54.00000000546237544, -32.49999999999999289 ) ) ;
#14014 = CARTESIAN_POINT ( 'NONE',  ( -24.18731323226221974, 68.28347249907602645, 14.01125832528330406 ) ) ;
#14015 = CARTESIAN_POINT ( 'NONE',  ( 33.58253175000000113, 46.12500000273117706, -4.112674001490185761E-15 ) ) ;
#14016 = CARTESIAN_POINT ( 'NONE',  ( 4.300734207923757602, 76.27500000273118985, -13.23629886949340673 ) ) ;
#14017 = CARTESIAN_POINT ( 'NONE',  ( 33.58253175000000823, 46.27500000273120406, 10.91162601494192863 ) ) ;
#14018 = CARTESIAN_POINT ( 'NONE',  ( -27.16883889988624290, 27.17500000273118133, -19.73931689729374028 ) ) ;
#14019 = CARTESIAN_POINT ( 'NONE',  ( 5.411497909691496133, 16.99999999999998934, 23.34105529868805817 ) ) ;
#14020 = CARTESIAN_POINT ( 'NONE',  ( 2.584737979205442066E-13, 21.02343750000000000, 27.95245687107223276 ) ) ;
#14021 = CARTESIAN_POINT ( 'NONE',  ( 5.334720326618300005E-14, 73.50000000000001421, -32.50000000000000000 ) ) ;
#14022 = CARTESIAN_POINT ( 'NONE',  ( -12.13525491562421088, 79.80000000000003979, -8.816778784387096835 ) ) ;
#14023 = CARTESIAN_POINT ( 'NONE',  ( -32.50000000000000000, 76.00000000000000000, 0.000000000000000000 ) ) ;
#14024 = CIRCLE ( 'NONE', #33183, 15.00000000000000000 ) ;
#14025 = CARTESIAN_POINT ( 'NONE',  ( -20.75514604977248112, 11.42500000273117955, 28.56700777964554661 ) ) ;
#14026 = CARTESIAN_POINT ( 'NONE',  ( 14.47279130897151944, 6.924999997268805885, -19.92008829642072598 ) ) ;
#14027 = CARTESIAN_POINT ( 'NONE',  ( -3.712076227271900841E-14, 10.24999999453763344, -24.50000000000000000 ) ) ;
#14028 = CARTESIAN_POINT ( 'NONE',  ( 24.18731323226221974, 32.18972249907602645, -14.01125832528328985 ) ) ;
#14029 = EDGE_CURVE ( 'NONE', #13792, #17050, #24856, .T. ) ;
#14030 = CARTESIAN_POINT ( 'NONE',  ( -1.778240108872766143E-15, 65.50000000000000000, -32.49999999999999289 ) ) ;
#14031 = CARTESIAN_POINT ( 'NONE',  ( -20.75514604977248112, 17.42500000273117777, 28.56700777964554661 ) ) ;
#14032 = CARTESIAN_POINT ( 'NONE',  ( 23.41746825000000243, 5.024999997268808194, 7.608796670333735079 ) ) ;
#14033 = CARTESIAN_POINT ( 'NONE',  ( 26.07999730980490227, 54.68229166666665719, 6.988114217767821046 ) ) ;
#14034 = ORIENTED_EDGE ( 'NONE', *, *, #16488, .F. ) ;
#14035 = CARTESIAN_POINT ( 'NONE',  ( -20.75514604977248823, 56.82500000273117990, -28.56700777964554305 ) ) ;
#14036 = CARTESIAN_POINT ( 'NONE',  ( -33.58253175000000113, 27.47500000273118204, 10.91162601494193929 ) ) ;
#14037 = ORIENTED_EDGE ( 'NONE', *, *, #30596, .T. ) ;
#14038 = CARTESIAN_POINT ( 'NONE',  ( -15.01150461594642138, 25.89322916666666430, -26.00068869287340334 ) ) ;
#14039 = CARTESIAN_POINT ( 'NONE',  ( -25.98046417659859486, 27.04465250092397000, -15.04653450569291628 ) ) ;
#14040 = CARTESIAN_POINT ( 'NONE',  ( 10.37757302488624767, 1.725000002731180704, 31.93888565452638417 ) ) ;
#14041 = CARTESIAN_POINT ( 'NONE',  ( -19.82091636218621034, 16.54999999453762882, -14.40073868116559552 ) ) ;
#14042 = CARTESIAN_POINT ( 'NONE',  ( 14.47279130897151767, 4.924999997268811214, -19.92008829642072598 ) ) ;
#14043 = CARTESIAN_POINT ( 'NONE',  ( 27.16883889988624290, 26.17500000273118133, 19.73931689729373673 ) ) ;
#14044 = CARTESIAN_POINT ( 'NONE',  ( -32.50000000000000000, 30.40000000546238823, -10.55989012756945478 ) ) ;
#14045 = AXIS2_PLACEMENT_3D ( 'NONE', #9301, #9480, #19785 ) ;
#14046 = CARTESIAN_POINT ( 'NONE',  ( -32.50000000000000000, 69.90000000000000568, -10.55989012756945478 ) ) ;
#14047 = CARTESIAN_POINT ( 'NONE',  ( 32.50000000000000711, 52.89999999999999147, 10.55989012756945122 ) ) ;
#14048 = CARTESIAN_POINT ( 'NONE',  ( 9.270509831248425314, 72.70000000000000284, 12.75976212528059683 ) ) ;
#14049 = CARTESIAN_POINT ( 'NONE',  ( 0.04044903254992426173, 51.68006916759063785, -30.02300923189239867 ) ) ;
#14050 = CARTESIAN_POINT ( 'NONE',  ( -10.37757302488624411, 44.97500000273119269, -31.93888565452638417 ) ) ;
#14051 = FILL_AREA_STYLE ('',( #3579 ) ) ;
#14052 = CARTESIAN_POINT ( 'NONE',  ( -23.41746825000000598, 12.22499999726881370, 7.608796670333726198 ) ) ;
#14053 = CARTESIAN_POINT ( 'NONE',  ( -26.29305231718578995, 14.19999999999999041, 19.10302069950538595 ) ) ;
#14054 = CARTESIAN_POINT ( 'NONE',  ( 24.50000000000000355, 14.09999999999999254, -7.960532557706203605 ) ) ;
#14055 = CARTESIAN_POINT ( 'NONE',  ( -19.11951029504797006, 44.93711833240935505, -19.06425588902558133 ) ) ;
#14056 = CARTESIAN_POINT ( 'NONE',  ( 10.37757302488624056, 64.52500000273120406, -31.93888565452638417 ) ) ;
#14057 = CARTESIAN_POINT ( 'NONE',  ( -27.16883889988624290, 49.17500000273117422, -19.73931689729374028 ) ) ;
#14058 = CARTESIAN_POINT ( 'NONE',  ( 7.236395654485755280, 8.224999997268806595, 22.27133577429736988 ) ) ;
#14059 = CARTESIAN_POINT ( 'NONE',  ( -3.880418787951156023, 8.551254281546841085, -24.49999999999999645 ) ) ;
#14060 = CARTESIAN_POINT ( 'NONE',  ( -27.16883889988623935, 3.325000002731171023, 19.73931689729374739 ) ) ;
#14061 = CARTESIAN_POINT ( 'NONE',  ( -14.01125832528285109, 36.49777750092397355, 24.18731323226248264 ) ) ;
#14062 = CARTESIAN_POINT ( 'NONE',  ( 32.52223864317537050, 66.99999999999998579, -1.355835680407735611 ) ) ;
#14063 = CARTESIAN_POINT ( 'NONE',  ( 6.410174973103799800, 51.99999999999999289, 32.88179426022558260 ) ) ;
#14064 = UNCERTAINTY_MEASURE_WITH_UNIT (LENGTH_MEASURE( 1.000000000000000082E-05 ), #361, 'distance_accuracy_value', 'NONE');
#14065 = CARTESIAN_POINT ( 'NONE',  ( 33.58253175000000113, 26.12500000273119838, -4.112674001490185761E-15 ) ) ;
#14066 = DIRECTION ( 'NONE',  ( -0.000000000000000000, -1.000000000000000000, -0.000000000000000000 ) ) ;
#14067 = DIRECTION ( 'NONE',  ( -1.000000000000000000, 0.000000000000000000, 0.000000000000000000 ) ) ;
#14068 = CARTESIAN_POINT ( 'NONE',  ( 32.50000000000000000, 61.09999999999998721, -10.55989012756945833 ) ) ;
#14069 = CARTESIAN_POINT ( 'NONE',  ( 20.53372385742108008, 53.53086833240935505, 20.47846945139866648 ) ) ;
#14070 = CARTESIAN_POINT ( 'NONE',  ( 10.04305231718578817, 49.90000000546239534, -30.90933677959249337 ) ) ;
#14071 = EDGE_CURVE ( 'NONE', #10540, #2121, #30001, .T. ) ;
#14072 = CARTESIAN_POINT ( 'NONE',  ( 0.000000000000000000, 80.00000000000001421, 0.000000000000000000 ) ) ;
#14073 = CARTESIAN_POINT ( 'NONE',  ( 0.000000000000000000, 82.00000000000001421, 0.000000000000000000 ) ) ;
#14074 = CARTESIAN_POINT ( 'NONE',  ( 19.09188309203661049, 26.60937499999999645, -19.09188309203694445 ) ) ;
#14075 = ADVANCED_FACE ( 'NONE', ( #9233 ), #1337, .T. ) ;
#14076 = CARTESIAN_POINT ( 'NONE',  ( -20.75514604977248112, 75.42500000273120975, 28.56700777964554661 ) ) ;
#14077 = CARTESIAN_POINT ( 'NONE',  ( 28.01184896238304134, 27.18229166666666430, 7.505752307972846538 ) ) ;
#14078 = CYLINDRICAL_SURFACE ( 'NONE', #18560, 15.00000000000000000 ) ;
#14079 = ORIENTED_EDGE ( 'NONE', *, *, #5392, .F. ) ;
#14080 = CARTESIAN_POINT ( 'NONE',  ( 20.47846945139902530, 52.96913166759063785, 20.53372385742071771 ) ) ;
#14081 = CARTESIAN_POINT ( 'NONE',  ( 6.277390505771533514E-15, 11.00000000546237544, 34.17252228774368916 ) ) ;
#14082 = AXIS2_PLACEMENT_3D ( 'NONE', #30347, #30690, #17845 ) ;
#14083 = CARTESIAN_POINT ( 'NONE',  ( -28.01184896238290278, 62.98958333333332149, 7.505752307973363457 ) ) ;
#14084 = CARTESIAN_POINT ( 'NONE',  ( -20.08610463437156923, 64.80000000546237970, 27.64615127144130113 ) ) ;
#14085 = CARTESIAN_POINT ( 'NONE',  ( -33.58253175000000113, 45.47500000273119980, 10.91162601494193929 ) ) ;
#14086 = CARTESIAN_POINT ( 'NONE',  ( 6.277390505771533514E-15, 49.00000000546238965, 34.17252228774368916 ) ) ;
#14087 =( BOUNDED_CURVE ( )  B_SPLINE_CURVE ( 2, ( #18539, #8216, #18709, #29146, #4974, #23167, #5651, #23346, #26588, #12697, #33807, #33629, #20610 ),
 .UNSPECIFIED., .F., .T. ) 
 B_SPLINE_CURVE_WITH_KNOTS ( ( 3, 2, 2, 2, 2, 2, 3 ),
 ( 0.3269230769230769273, 0.3282051282051282048, 0.3307692307692307598, 0.3333333333333333148, 0.3358974358974358698, 0.3384615384615384803, 0.3397435898119063880 ),
 .UNSPECIFIED. ) 
 CURVE ( )  GEOMETRIC_REPRESENTATION_ITEM ( )  RATIONAL_B_SPLINE_CURVE ( ( 0.9755282581475768211, 0.9755282581475768211, 1.000000000000000000, 0.9510565162951535312, 1.000000000000000000, 0.9510565162951535312, 1.000000000000000000, 0.9510565162951535312, 1.000000000000000000, 0.9510565162951535312, 1.000000000000000000, 0.9755282568435517110, 0.9755282581475768211 ) ) 
 REPRESENTATION_ITEM ( '' )  );
#14088 = CARTESIAN_POINT ( 'NONE',  ( 2.688165632520823219E-15, 73.87500000273116996, 14.63369212191046387 ) ) ;
#14089 = CARTESIAN_POINT ( 'NONE',  ( 27.16883889988623935, 34.32500000273120122, -19.73931689729374384 ) ) ;
#14090 = CARTESIAN_POINT ( 'NONE',  ( -26.29305231718579350, 62.30000000546238681, -19.10302069950537884 ) ) ;
#14091 = CARTESIAN_POINT ( 'NONE',  ( 10.37757302488624767, 59.97500000273120691, 31.93888565452638417 ) ) ;
#14092 = SURFACE_STYLE_FILL_AREA ( #27293 ) ;
#14093 = CARTESIAN_POINT ( 'NONE',  ( 20.08610463437158344, 36.70000000000000995, 27.64615127144129403 ) ) ;
#14094 = CARTESIAN_POINT ( 'NONE',  ( 10.04305231718578817, 37.39999999999999147, -30.90933677959249337 ) ) ;
#14095 = CARTESIAN_POINT ( 'NONE',  ( 23.41746824999999887, 8.624999997268817609, 0.000000000000000000 ) ) ;
#14096 = CARTESIAN_POINT ( 'NONE',  ( -20.75514604977248112, 1.675000002731184434, 28.56700777964554661 ) ) ;
#14097 = CARTESIAN_POINT ( 'NONE',  ( 32.50000000000000711, 12.90000000000000036, 10.55989012756945122 ) ) ;
#14098 = CARTESIAN_POINT ( 'NONE',  ( -8.601468415847518756, 81.07500000273117280, -11.83890561707634603 ) ) ;
#14099 = CARTESIAN_POINT ( 'NONE',  ( -10.37757302488624411, 74.97500000273119269, -31.93888565452638417 ) ) ;
#14100 = CARTESIAN_POINT ( 'NONE',  ( -24.50000000000000000, 18.64999999453763380, -7.960532557706207157 ) ) ;
#14101 = CARTESIAN_POINT ( 'NONE',  ( 27.16883889988623935, 66.57500000273118701, -19.73931689729374384 ) ) ;
#14102 = ORIENTED_EDGE ( 'NONE', *, *, #16824, .T. ) ;
#14103 = CARTESIAN_POINT ( 'NONE',  ( -4.732186688966233175E-15, 5.249999994537621895, 25.76082449383753925 ) ) ;
#14104 = CARTESIAN_POINT ( 'NONE',  ( -0.04044903254992426173, 15.58631916759064495, 27.95245687107223276 ) ) ;
#14105 = CARTESIAN_POINT ( 'NONE',  ( 9.270509831248421762, 75.30000000000001137, -12.75976212528059861 ) ) ;
#14106 = CARTESIAN_POINT ( 'NONE',  ( 10.37757302488624767, 45.72500000273120691, 31.93888565452638417 ) ) ;
#14107 = CARTESIAN_POINT ( 'NONE',  ( 33.58253175000000823, 8.275000002731191628, 10.91162601494192863 ) ) ;
#14108 = CARTESIAN_POINT ( 'NONE',  ( -10.37757302488624411, 60.97500000273119269, -31.93888565452638417 ) ) ;
#14109 = CARTESIAN_POINT ( 'NONE',  ( 6.988114217767829928, 46.94791666666666430, -26.07999730980489872 ) ) ;
#14110 = CARTESIAN_POINT ( 'NONE',  ( -15.04653450569291984, 39.93527750092397355, 25.98046417659859486 ) ) ;
#14111 = CARTESIAN_POINT ( 'NONE',  ( 20.53372385742108008, 29.46836833240935505, 20.47846945139866648 ) ) ;
#14112 = CARTESIAN_POINT ( 'NONE',  ( -32.50000000000000000, 70.40000000546237402, -10.55989012756945478 ) ) ;
#14113 = CARTESIAN_POINT ( 'NONE',  ( -13.91746824999999532, 78.97500000273117848, 4.522059556121122093 ) ) ;
#14114 = CARTESIAN_POINT ( 'NONE',  ( 26.09010956794244507, 60.11940999907602645, 6.950374756619249084 ) ) ;
#14115 = CARTESIAN_POINT ( 'NONE',  ( -23.41746824999999887, 17.62499999726882649, -2.867812753649727150E-15 ) ) ;
#14116 = EDGE_CURVE ( 'NONE', #26616, #3774, #19717, .T. ) ;
#14117 = ADVANCED_FACE ( 'NONE', ( #27603 ), #16619, .T. ) ;
#14118 = ORIENTED_EDGE ( 'NONE', *, *, #26858, .F. ) ;
#14119 = CARTESIAN_POINT ( 'NONE',  ( 10.37757302488624767, 43.97500000273117848, 31.93888565452638417 ) ) ;
#14120 = CARTESIAN_POINT ( 'NONE',  ( -10.04305231718578462, 76.39999999999999147, 30.90933677959249337 ) ) ;
#14121 = CARTESIAN_POINT ( 'NONE',  ( 24.22776226481241224, 55.69048583425730925, -13.94119854578936923 ) ) ;
#14122 = CARTESIAN_POINT ( 'NONE',  ( 26.29305231718578995, 31.70000000546237118, -19.10302069950538240 ) ) ;
#14123 = ORIENTED_EDGE ( 'NONE', *, *, #19915, .T. ) ;
#14124 = CARTESIAN_POINT ( 'NONE',  ( -20.75514604977248823, 20.82500000273119412, -28.56700777964554305 ) ) ;
#14125 = CARTESIAN_POINT ( 'NONE',  ( -7.505752307972844761, 34.91666666666666430, 28.01184896238304134 ) ) ;
#14126 = ORIENTED_EDGE ( 'NONE', *, *, #6826, .F. ) ;
#14127 = ORIENTED_EDGE ( 'NONE', *, *, #19722, .F. ) ;
#14128 = CARTESIAN_POINT ( 'NONE',  ( 20.08610463437158344, 65.20000000546235697, 27.64615127144129403 ) ) ;
#14129 = CARTESIAN_POINT ( 'NONE',  ( -33.58253175000000113, 53.02500000273118985, -10.91162601494193218 ) ) ;
#14130 = CARTESIAN_POINT ( 'NONE',  ( -15.01150461594595775, 55.68489583333332860, 26.00068869287368756 ) ) ;
#14131 = CARTESIAN_POINT ( 'NONE',  ( -20.08610463437156923, 14.80000000546238503, 27.64615127144130113 ) ) ;
#14132 = CARTESIAN_POINT ( 'NONE',  ( -26.29305231718579350, 66.30000000546237970, -19.10302069950537884 ) ) ;
#14133 = CARTESIAN_POINT ( 'NONE',  ( 23.41746824999999887, 15.02499999726881086, 7.608796670333735079 ) ) ;
#14134 = CARTESIAN_POINT ( 'NONE',  ( 20.08610463437157279, 57.29999999999999005, -27.64615127144129758 ) ) ;
#14135 = CARTESIAN_POINT ( 'NONE',  ( 33.58253175000000113, 22.47500000273119625, -10.91162601494193751 ) ) ;
#14136 = CARTESIAN_POINT ( 'NONE',  ( 0.04044903255045854962, 67.71055583240935505, 30.02300923189239867 ) ) ;
#14137 = CARTESIAN_POINT ( 'NONE',  ( 4.300734207923757602, 76.27500000273118985, -13.23629886949340673 ) ) ;
#14138 = CARTESIAN_POINT ( 'NONE',  ( 15.14183272437242422, 16.30000000000000782, -20.84094480462497856 ) ) ;
#14139 = CARTESIAN_POINT ( 'NONE',  ( 10.04305231718578817, 15.39999999999999680, -30.90933677959249337 ) ) ;
#14140 = CARTESIAN_POINT ( 'NONE',  ( -26.29305231718579350, 11.80000000000001847, -19.10302069950537884 ) ) ;
#14141 = ORIENTED_EDGE ( 'NONE', *, *, #3157, .F. ) ;
#14142 = CARTESIAN_POINT ( 'NONE',  ( -4.523095164977116484E-15, 4.624999997268820273, 24.62258325217400312 ) ) ;
#14143 = CARTESIAN_POINT ( 'NONE',  ( 4.300734207923757602, 78.27500000273118985, -13.23629886949340673 ) ) ;
#14144 = CARTESIAN_POINT ( 'NONE',  ( 26.07999730980490227, 44.36979166666666430, 6.988114217767821046 ) ) ;
#14145 = CARTESIAN_POINT ( 'NONE',  ( 10.37757302488624056, 16.52500000273118985, -31.93888565452638417 ) ) ;
#14146 = CARTESIAN_POINT ( 'NONE',  ( -27.16883889988624290, 68.92500000273120975, -19.73931689729374028 ) ) ;
#14147 = CARTESIAN_POINT ( 'NONE',  ( -20.75514604977248112, 27.67500000273118133, 28.56700777964554661 ) ) ;
#14148 = CARTESIAN_POINT ( 'NONE',  ( -27.16883889988623935, 15.57500000273119589, 19.73931689729374739 ) ) ;
#14149 = CARTESIAN_POINT ( 'NONE',  ( 10.37757302488624056, 8.775000002731180970, -31.93888565452638417 ) ) ;
#14150 = CARTESIAN_POINT ( 'NONE',  ( -26.09010956794232428, 64.42746500092397355, 6.950374756619732253 ) ) ;
#14151 = CARTESIAN_POINT ( 'NONE',  ( 15.01150461594643204, 58.54947916666665009, 26.00068869287340334 ) ) ;
#14152 = CARTESIAN_POINT ( 'NONE',  ( 13.91746824999999532, 80.47500000273119269, -4.522059556121118540 ) ) ;
#14153 = CARTESIAN_POINT ( 'NONE',  ( 26.29305231718578995, 45.20000000000000284, -19.10302069950538240 ) ) ;
#14154 = CARTESIAN_POINT ( 'NONE',  ( 26.29305231718578995, 63.20000000000000284, -19.10302069950538240 ) ) ;
#14155 = CARTESIAN_POINT ( 'NONE',  ( 27.16883889988624290, 53.92500000273120264, 19.73931689729373673 ) ) ;
#14156 = CARTESIAN_POINT ( 'NONE',  ( -7.236395654485757944, 15.72499999726881192, -22.27133577429736988 ) ) ;
#14157 = CIRCLE ( 'NONE', #11333, 0.9999999999999988898 ) ;
#14158 = EDGE_LOOP ( 'NONE', ( #16449, #10959, #7249, #306 ) ) ;
#14159 = CARTESIAN_POINT ( 'NONE',  ( 33.58253175000000113, 64.37500000273121259, -4.112674001490185761E-15 ) ) ;
#14160 = FACE_OUTER_BOUND ( 'NONE', #10919, .T. ) ;
#14161 = CARTESIAN_POINT ( 'NONE',  ( -23.41746825000000598, 5.724999997268815477, 7.608796670333726198 ) ) ;
#14162 = CARTESIAN_POINT ( 'NONE',  ( 24.22776226481241224, 28.19048583425731636, -13.94119854578936923 ) ) ;
#14163 = VERTEX_POINT ( 'NONE', #30336 ) ;
#14164 = CARTESIAN_POINT ( 'NONE',  ( 20.75514604977248467, 38.42500000273118133, -28.56700777964554305 ) ) ;
#14165 = CARTESIAN_POINT ( 'NONE',  ( 0.000000000000000000, 80.00000000000001421, -32.50000000000000000 ) ) ;
#14166 = ORIENTED_EDGE ( 'NONE', *, *, #11970, .F. ) ;
#14167 = CARTESIAN_POINT ( 'NONE',  ( 28.01184896238290278, 50.95833333333332860, -7.505752307973347470 ) ) ;
#14168 = CARTESIAN_POINT ( 'NONE',  ( 20.75514604977248467, 60.67500000273118133, -28.56700777964554305 ) ) ;
#14169 = CARTESIAN_POINT ( 'NONE',  ( -20.08610463437156923, 0.8000000054623763734, 27.64615127144130113 ) ) ;
#14170 = CARTESIAN_POINT ( 'NONE',  ( -33.58253175000000113, 75.02500000273117564, -10.91162601494193218 ) ) ;
#14171 = CARTESIAN_POINT ( 'NONE',  ( 26.00068869287340334, 33.62760416666665719, -15.01150461594642316 ) ) ;
#14172 = CARTESIAN_POINT ( 'NONE',  ( -15.14183272437241889, 6.699999999999991296, -20.84094480462497856 ) ) ;
#14173 = CARTESIAN_POINT ( 'NONE',  ( -27.16883889988624290, 3.175000002731187543, -19.73931689729374028 ) ) ;
#14174 = CARTESIAN_POINT ( 'NONE',  ( -27.16883889988624290, 16.92500000273117067, -19.73931689729374028 ) ) ;
#14175 = CARTESIAN_POINT ( 'NONE',  ( -11.25946833292375793, 71.07500000273120122, 8.180482586598737171 ) ) ;
#14176 = CARTESIAN_POINT ( 'NONE',  ( -28.00173670424535644, 40.92670166574268364, 7.543491769121936308 ) ) ;
#14177 = CARTESIAN_POINT ( 'NONE',  ( 15.00000000000000000, 79.00000000000001421, -1.836970198721029589E-15 ) ) ;
#14178 = CARTESIAN_POINT ( 'NONE',  ( 15.01150461594643382, 61.98697916666665719, 26.00068869287340334 ) ) ;
#14179 = CARTESIAN_POINT ( 'NONE',  ( -17.29030653276319995, 16.99999999999998579, 17.35785989121602668 ) ) ;
#14180 = CARTESIAN_POINT ( 'NONE',  ( -5.147494310547423346, 38.94874572391552192, 32.50000000000000000 ) ) ;
#14181 = CARTESIAN_POINT ( 'NONE',  ( -26.07999730980490583, 15.15104166666666252, -6.988114217767815717 ) ) ;
#14182 = CARTESIAN_POINT ( 'NONE',  ( -27.16883889988624290, 36.92500000273118843, -19.73931689729374028 ) ) ;
#14183 = CARTESIAN_POINT ( 'NONE',  ( 2.688165632520823219E-15, 75.37500000273118417, 14.63369212191046387 ) ) ;
#14184 = CARTESIAN_POINT ( 'NONE',  ( -33.58253175000000113, 51.47500000273118559, 10.91162601494193929 ) ) ;
#14185 = CARTESIAN_POINT ( 'NONE',  ( -33.58253175000000113, 25.47500000273118914, 10.91162601494193929 ) ) ;
#14186 = CARTESIAN_POINT ( 'NONE',  ( 1.555960095263670572E-15, 16.24999999453762101, -24.50000000000000000 ) ) ;
#14187 = CARTESIAN_POINT ( 'NONE',  ( 2.584737979205442066E-13, 34.77343750000000000, 27.95245687107223276 ) ) ;
#14188 = CYLINDRICAL_SURFACE ( 'NONE', #10320, 32.50000000000000000 ) ;
#14189 = CARTESIAN_POINT ( 'NONE',  ( -4.223320258572821363E-15, 80.50000000000001421, 15.00000000000000355 ) ) ;
#14190 =( BOUNDED_CURVE ( )  B_SPLINE_CURVE ( 2, ( #21093, #8033, #18519, #297, #28965, #5461, #15942, #26398, #19020, #13697, #21919, #5631, #18850, #29298, #3723, #32036, #14193, #802, #24162, #16770, #632, #8534, #1122, #8362, #16115, #11122, #26567, #29461, #32369, #3063, #5796, #8863, #21590, #13534, #19348, #19182, #23997, #5964, #3393, #11284, #16442, #21762, #26894, #16278, #3229, #8198, #26736, #13863, #8699, #24328, #32205, #29620, #6123, #468, #11442, #10951, #21427, #16607, #29790, #27060, #3553, #6294, #29128, #14026, #24489, #31868, #962, #24648, #27229, #21261, #31706, #18689, #27735, #6465, #30464, #27564, #6962, #16939, #32698, #1468, #27396, #11944, #4223, #25155, #19839, #9710, #14697, #20018, #14525, #25506, #17612, #17272, #1631, #20192, #22413, #12109, #14864, #22581, #14358, #28074, #24985, #30292, #30635, #17447, #6793, #4050, #33032, #11775, #9536, #7132, #27908, #4390, #4563, #25329, #1807, #22255, #12283, #19512, #19677, #22757, #33207, #3885, #9192, #32861, #24816, #9358, #32533, #9033, #11607, #15041, #22089, #29960, #1293, #30123, #6626, #17105, #23615, #2155, #15733, #26187, #7303, #12460, #20718, #30809, #12975, #31499, #17966, #31159, #17787, #21050, #12805, #2683, #30986, #33386, #7486, #20541, #28415, #12629, #13142, #33562, #1985, #28247, #4905, #15211, #28581, #84, #18137, #15386, #10571, #10401, #25842, #10061, #7991, #15563, #20880, #26015, #33742, #10237, #2330, #18476, #20362 ),
 .UNSPECIFIED., .F., .T. ) 
 B_SPLINE_CURVE_WITH_KNOTS ( ( 3, 2, 2, 2, 2, 2, 2, 2, 2, 2, 2, 2, 2, 2, 2, 2, 2, 2, 2, 2, 2, 2, 2, 2, 2, 2, 2, 2, 2, 2, 2, 2, 2, 2, 2, 2, 2, 2, 2, 2, 2, 2, 2, 2, 2, 2, 2, 2, 2, 2, 2, 2, 2, 2, 2, 2, 2, 2, 2, 2, 2, 2, 2, 2, 2, 2, 2, 2, 2, 2, 2, 2, 2, 2, 2, 2, 2, 2, 2, 2, 2, 2, 2, 2, 2, 2, 2, 2, 2, 2, 3 ),
 ( 0.000000000000000000, 0.01111111111111111154, 0.02222222222222222307, 0.03333333333333333287, 0.04444444444444444614, 0.05555555555555555247, 0.06666666666666666574, 0.07777777777777777901, 0.08888888888888889228, 0.1000000000000000056, 0.1111111111111111049, 0.1222222222222222182, 0.1333333333333333315, 0.1444444444444444309, 0.1555555555555555580, 0.1666666666666666574, 0.1777777777777777846, 0.1888888888888888840, 0.2000000000000000111, 0.2111111111111111105, 0.2222222222222222099, 0.2333333333333333370, 0.2444444444444444364, 0.2555555555555555358, 0.2666666666666666630, 0.2777777777777777901, 0.2888888888888888618, 0.2999999999999999889, 0.3111111111111111160, 0.3222222222222222432, 0.3333333333333333148, 0.3444444444444444420, 0.3555555555555555691, 0.3666666666666666408, 0.3777777777777777679, 0.3888888888888888951, 0.4000000000000000222, 0.4111111111111110938, 0.4222222222222222210, 0.4333333333333333481, 0.4444444444444444198, 0.4555555555555555469, 0.4666666666666666741, 0.4777777777777778012, 0.4888888888888888729, 0.5000000000000000000, 0.5111111111111110716, 0.5222222222222222543, 0.5333333333333333259, 0.5444444444444443976, 0.5555555555555555802, 0.5666666666666666519, 0.5777777777777777235, 0.5888888888888889062, 0.5999999999999999778, 0.6111111111111111605, 0.6222222222222222321, 0.6333333333333333037, 0.6444444444444444864, 0.6555555555555555580, 0.6666666666666666297, 0.6777777777777778123, 0.6888888888888888840, 0.6999999999999999556, 0.7111111111111111382, 0.7222222222222222099, 0.7333333333333332815, 0.7444444444444444642, 0.7555555555555555358, 0.7666666666666667185, 0.7777777777777777901, 0.7888888888888888618, 0.8000000000000000444, 0.8111111111111111160, 0.8222222222222221877, 0.8333333333333333703, 0.8444444444444444420, 0.8555555555555555136, 0.8666666666666666963, 0.8777777777777777679, 0.8888888888888888395, 0.9000000000000000222, 0.9111111111111110938, 0.9222222222222222765, 0.9333333333333333481, 0.9444444444444444198, 0.9555555555555556024, 0.9666666666666666741, 0.9777777777777777457, 0.9888888888888889284, 1.000000000000000000 ),
 .UNSPECIFIED. ) 
 CURVE ( )  GEOMETRIC_REPRESENTATION_ITEM ( )  RATIONAL_B_SPLINE_CURVE ( ( 1.000000000000000000, 0.9510565162951535312, 1.000000000000000000, 0.9510565162951535312, 1.000000000000000000, 0.9510565162951535312, 1.000000000000000000, 0.9510565162951535312, 1.000000000000000000, 0.9510565162951535312, 1.000000000000000000, 0.9510565162951535312, 1.000000000000000000, 0.9510565162951535312, 1.000000000000000000, 0.9510565162951535312, 1.000000000000000000, 0.9510565162951535312, 1.000000000000000000, 0.9510565162951535312, 1.000000000000000000, 0.9510565162951535312, 1.000000000000000000, 0.9510565162951535312, 1.000000000000000000, 0.9510565162951535312, 1.000000000000000000, 0.9510565162951535312, 1.000000000000000000, 0.9510565162951535312, 1.000000000000000000, 0.9510565162951535312, 1.000000000000000000, 0.9510565162951535312, 1.000000000000000000, 0.9510565162951535312, 1.000000000000000000, 0.9510565162951535312, 1.000000000000000000, 0.9510565162951535312, 1.000000000000000000, 0.9510565162951535312, 1.000000000000000000, 0.9510565162951535312, 1.000000000000000000, 0.9510565162951535312, 1.000000000000000000, 0.9510565162951535312, 1.000000000000000000, 0.9510565162951535312, 1.000000000000000000, 0.9510565162951535312, 1.000000000000000000, 0.9510565162951535312, 1.000000000000000000, 0.9510565162951535312, 1.000000000000000000, 0.9510565162951535312, 1.000000000000000000, 0.9510565162951535312, 1.000000000000000000, 0.9510565162951535312, 1.000000000000000000, 0.9510565162951535312, 1.000000000000000000, 0.9510565162951535312, 1.000000000000000000, 0.9510565162951535312, 1.000000000000000000, 0.9510565162951535312, 1.000000000000000000, 0.9510565162951535312, 1.000000000000000000, 0.9510565162951535312, 1.000000000000000000, 0.9510565162951535312, 1.000000000000000000, 0.9510565162951535312, 1.000000000000000000, 0.9510565162951535312, 1.000000000000000000, 0.9510565162951535312, 1.000000000000000000, 0.9510565162951535312, 1.000000000000000000, 0.9510565162951535312, 1.000000000000000000, 0.9510565162951535312, 1.000000000000000000, 0.9510565162951535312, 1.000000000000000000, 0.9510565162951535312, 1.000000000000000000, 0.9510565162951535312, 1.000000000000000000, 0.9510565162951535312, 1.000000000000000000, 0.9510565162951535312, 1.000000000000000000, 0.9510565162951535312, 1.000000000000000000, 0.9510565162951535312, 1.000000000000000000, 0.9510565162951535312, 1.000000000000000000, 0.9510565162951535312, 1.000000000000000000, 0.9510565162951535312, 1.000000000000000000, 0.9510565162951535312, 1.000000000000000000, 0.9510565162951535312, 1.000000000000000000, 0.9510565162951535312, 1.000000000000000000, 0.9510565162951535312, 1.000000000000000000, 0.9510565162951535312, 1.000000000000000000, 0.9510565162951535312, 1.000000000000000000, 0.9510565162951535312, 1.000000000000000000, 0.9510565162951535312, 1.000000000000000000, 0.9510565162951535312, 1.000000000000000000, 0.9510565162951535312, 1.000000000000000000, 0.9510565162951535312, 1.000000000000000000, 0.9510565162951535312, 1.000000000000000000, 0.9510565162951535312, 1.000000000000000000, 0.9510565162951535312, 1.000000000000000000, 0.9510565162951535312, 1.000000000000000000, 0.9510565162951535312, 1.000000000000000000, 0.9510565162951535312, 1.000000000000000000, 0.9510565162951535312, 1.000000000000000000, 0.9510565162951535312, 1.000000000000000000, 0.9510565162951535312, 1.000000000000000000, 0.9510565162951535312, 1.000000000000000000, 0.9510565162951535312, 1.000000000000000000, 0.9510565162951535312, 1.000000000000000000, 0.9510565162951535312, 1.000000000000000000, 0.9510565162951535312, 1.000000000000000000, 0.9510565162951535312, 1.000000000000000000, 0.9510565162951535312, 1.000000000000000000, 0.9510565162951535312, 1.000000000000000000, 0.9510565162951535312, 1.000000000000000000, 0.9510565162951535312, 1.000000000000000000, 0.9510565162951535312, 1.000000000000000000, 0.9510565162951535312, 1.000000000000000000, 0.9510565162951535312, 1.000000000000000000, 0.9510565162951535312, 1.000000000000000000, 0.9510565162951535312, 1.000000000000000000, 0.9510565162951535312, 1.000000000000000000 ) ) 
 REPRESENTATION_ITEM ( '' )  );
#14191 = CARTESIAN_POINT ( 'NONE',  ( -26.29305231718578995, 64.20000000000001705, 19.10302069950538595 ) ) ;
#14192 = CARTESIAN_POINT ( 'NONE',  ( 10.37757302488624056, 6.525000002731193405, -31.93888565452638417 ) ) ;
#14193 = CARTESIAN_POINT ( 'NONE',  ( 7.236395654485755280, 2.224999997268800378, 22.27133577429736988 ) ) ;
#14194 = CARTESIAN_POINT ( 'NONE',  ( 26.02091320914876960, 29.32513916574269075, 14.97647472619900455 ) ) ;
#14195 = CARTESIAN_POINT ( 'NONE',  ( -5.485892052525789174E-07, 66.99999999999998579, 32.49999999999999289 ) ) ;
#14196 = CARTESIAN_POINT ( 'NONE',  ( -19.11951029504797006, 31.18711833240935150, -19.06425588902558133 ) ) ;
#14197 = EDGE_CURVE ( 'NONE', #33960, #10375, #11184, .T. ) ;
#14198 = CYLINDRICAL_SURFACE ( 'NONE', #10149, 32.50000000000000000 ) ;
#14199 = CARTESIAN_POINT ( 'NONE',  ( 20.75514604977249178, 21.82500000273118346, 28.56700777964553950 ) ) ;
#14200 = CARTESIAN_POINT ( 'NONE',  ( -18.94512977948575738, 3.924999997268807661, -13.76444248337723231 ) ) ;
#14201 = CARTESIAN_POINT ( 'NONE',  ( -27.95245687107222921, 49.38281249999997868, 2.498001805406602216E-13 ) ) ;
#14202 = VERTEX_POINT ( 'NONE', #17831 ) ;
#14203 = CARTESIAN_POINT ( 'NONE',  ( 33.58253175000000113, 54.22500000273117848, -10.91162601494193751 ) ) ;
#14204 = CARTESIAN_POINT ( 'NONE',  ( -10.37757302488623701, 29.77500000273118630, 31.93888565452638417 ) ) ;
#14205 = VERTEX_POINT ( 'NONE', #33950 ) ;
#14206 = CARTESIAN_POINT ( 'NONE',  ( 7.505752307972854531, 22.88541666666666430, -28.01184896238303423 ) ) ;
#14207 = CARTESIAN_POINT ( 'NONE',  ( -20.47846945139902175, 27.18788166759063785, -20.53372385742072481 ) ) ;
#14208 = CARTESIAN_POINT ( 'NONE',  ( -20.08610463437156923, 10.29999999999999361, 27.64615127144130113 ) ) ;
#14209 = CARTESIAN_POINT ( 'NONE',  ( 7.570916362186207671, 13.34999999453762065, 23.30088464923126779 ) ) ;
#14210 = CARTESIAN_POINT ( 'NONE',  ( -4.523095164977116484E-15, 4.124999997268806951, 24.62258325217400312 ) ) ;
#14211 = CARTESIAN_POINT ( 'NONE',  ( -10.37757302488623701, 23.77500000273119340, 31.93888565452638417 ) ) ;
#14212 = CARTESIAN_POINT ( 'NONE',  ( 26.29305231718579350, 31.30000000546237615, 19.10302069950537529 ) ) ;
#14213 = CARTESIAN_POINT ( 'NONE',  ( 20.08610463437158344, 74.70000000000000284, 27.64615127144129403 ) ) ;
#14214 = CARTESIAN_POINT ( 'NONE',  ( 32.50000000000000000, 47.50000000546239676, -3.980102097228898626E-15 ) ) ;
#14215 = CARTESIAN_POINT ( 'NONE',  ( 0.000000000000000000, 80.00000000000001421, 0.000000000000000000 ) ) ;
#14216 = CARTESIAN_POINT ( 'NONE',  ( 14.97647472619947351, 59.98736083425730925, 26.02091320914850314 ) ) ;
#14217 = CARTESIAN_POINT ( 'NONE',  ( 10.37757302488624767, 37.97500000273118559, 31.93888565452638417 ) ) ;
#14218 = CARTESIAN_POINT ( 'NONE',  ( -10.37757302488623701, 55.52500000273118275, 31.93888565452638417 ) ) ;
#14219 = CARTESIAN_POINT ( 'NONE',  ( -26.00068869287368756, 25.60677083333332860, -15.01150461594595775 ) ) ;
#14220 =( NAMED_UNIT ( * ) PLANE_ANGLE_UNIT ( ) SI_UNIT ( $, .RADIAN. ) );
#14221 = CARTESIAN_POINT ( 'NONE',  ( -18.94512977948575738, 11.92499999726881477, -13.76444248337723231 ) ) ;
#14222 = CARTESIAN_POINT ( 'NONE',  ( 26.29305231718579350, 16.79999999999998295, 19.10302069950537529 ) ) ;
#14223 = CARTESIAN_POINT ( 'NONE',  ( -24.50000000000000355, 10.90000000000000568, -7.960532557706207157 ) ) ;
#14224 = CARTESIAN_POINT ( 'NONE',  ( -13.94119854578892514, 47.37201416574269786, 24.22776226481266448 ) ) ;
#14225 = CARTESIAN_POINT ( 'NONE',  ( -27.16883889988624290, 60.92500000273118133, -19.73931689729374028 ) ) ;
#14226 = CARTESIAN_POINT ( 'NONE',  ( -33.58253175000000113, 45.47500000273119980, 10.91162601494193929 ) ) ;
#14227 = CARTESIAN_POINT ( 'NONE',  ( -7.236395654485757944, 11.22499999726880837, -22.27133577429736988 ) ) ;
#14228 = CARTESIAN_POINT ( 'NONE',  ( 24.50000000000000000, 3.849999994537637082, -7.960532557706203605 ) ) ;
#14229 = CARTESIAN_POINT ( 'NONE',  ( -33.58253175000000113, 5.225000002731188253, 10.91162601494193929 ) ) ;
#14230 = CARTESIAN_POINT ( 'NONE',  ( 6.950374756619721595, 39.50559000092398065, 26.09010956794232428 ) ) ;
#14231 = CARTESIAN_POINT ( 'NONE',  ( 32.50000000000000000, 25.60000000546239107, -10.55989012756945833 ) ) ;
#14232 = CARTESIAN_POINT ( 'NONE',  ( -32.50000000000000000, 41.89999999999998437, -10.55989012756945300 ) ) ;
#14233 = CARTESIAN_POINT ( 'NONE',  ( 27.16883889988624290, 29.92500000273119909, 19.73931689729373673 ) ) ;
#14234 = LINE ( 'NONE', #3927, #20444 ) ;
#14235 = CARTESIAN_POINT ( 'NONE',  ( 0.000000000000000000, 11.99999999999999645, 27.00000000000000000 ) ) ;
#14236 = CARTESIAN_POINT ( 'NONE',  ( 5.147494310547434893, 60.55125428154683220, 32.49999999999999289 ) ) ;
#14237 = CARTESIAN_POINT ( 'NONE',  ( 30.02300923189239867, 56.53868083240936215, -0.04044903255044467877 ) ) ;
#14238 = CARTESIAN_POINT ( 'NONE',  ( 32.50000000000000711, 49.40000000546236691, 10.55989012756945122 ) ) ;
#14239 = LINE ( 'NONE', #27275, #13437 ) ;
#14240 = CARTESIAN_POINT ( 'NONE',  ( 24.20753774853756113, 23.88802083333331794, 13.97622843553589789 ) ) ;
#14241 = VERTEX_POINT ( 'NONE', #15774 ) ;
#14242 = CARTESIAN_POINT ( 'NONE',  ( -10.37757302488624411, 72.72500000273117848, -31.93888565452638417 ) ) ;
#14243 = CARTESIAN_POINT ( 'NONE',  ( 7.505752307972854531, 29.76041666666666430, -28.01184896238303423 ) ) ;
#14244 = DIRECTION ( 'NONE',  ( 0.000000000000000000, 0.000000000000000000, 1.000000000000000000 ) ) ;
#14245 = EDGE_LOOP ( 'NONE', ( #33003, #28629, #1263, #16525, #19460, #30393, #4000, #9720 ) ) ;
#14246 = CARTESIAN_POINT ( 'NONE',  ( 14.97647472619947351, 53.11236083425731636, 26.02091320914850314 ) ) ;
#14247 = CARTESIAN_POINT ( 'NONE',  ( 32.50000000000000711, 11.40000000546237580, 10.55989012756945122 ) ) ;
#14248 = CARTESIAN_POINT ( 'NONE',  ( 2.740863092043355209E-13, 58.83593750000000000, 30.02300923189239512 ) ) ;
#14249 = CARTESIAN_POINT ( 'NONE',  ( 5.147494310547434893, 56.55125428154683220, 32.49999999999999289 ) ) ;
#14250 = CARTESIAN_POINT ( 'NONE',  ( 20.75514604977249178, 46.07500000273117280, 28.56700777964553950 ) ) ;
#14251 = CARTESIAN_POINT ( 'NONE',  ( 26.29305231718578995, 51.70000000546237828, -19.10302069950538240 ) ) ;
#14252 = CARTESIAN_POINT ( 'NONE',  ( -8.601468415847515203, 73.67500000273118133, 11.83890561707634959 ) ) ;
#14253 = CARTESIAN_POINT ( 'NONE',  ( 20.75514604977248467, 28.42500000273118133, -28.56700777964554305 ) ) ;
#14254 = CARTESIAN_POINT ( 'NONE',  ( 24.50000000000000000, 12.09999999999999609, -7.960532557706203605 ) ) ;
#14255 = CARTESIAN_POINT ( 'NONE',  ( 6.486482029760649416E-15, 59.87500000273117706, 35.31076352940723240 ) ) ;
#14256 = CARTESIAN_POINT ( 'NONE',  ( -10.04305231718579172, 35.60000000000000853, -30.90933677959248982 ) ) ;
#14257 = CARTESIAN_POINT ( 'NONE',  ( 32.50000000000000711, 36.89999999999999858, 10.55989012756945122 ) ) ;
#14258 = CARTESIAN_POINT ( 'NONE',  ( 23.41746824999999887, 14.62499999726882294, 0.000000000000000000 ) ) ;
#14259 = EDGE_CURVE ( 'NONE', #1603, #32300, #25379, .T. ) ;
#14260 = CARTESIAN_POINT ( 'NONE',  ( 10.37757302488624056, 2.775000002731176085, -31.93888565452638417 ) ) ;
#14261 = DIRECTION ( 'NONE',  ( -0.000000000000000000, -1.000000000000000000, -0.000000000000000000 ) ) ;
#14262 = CARTESIAN_POINT ( 'NONE',  ( 13.91746825000000065, 78.27500000273120406, 4.522059556121115875 ) ) ;
#14263 = CARTESIAN_POINT ( 'NONE',  ( 6.486482029760648627E-15, 65.87500000273119838, 35.31076352940722529 ) ) ;
#14264 = CARTESIAN_POINT ( 'NONE',  ( 3.445340210940985210E-14, 5.499999999999997335, 24.50000000000000000 ) ) ;
#14265 = EDGE_CURVE ( 'NONE', #26368, #19609, #18349, .T. ) ;
#14266 = CARTESIAN_POINT ( 'NONE',  ( 6.486482029760649416E-15, 59.87500000273117706, 35.31076352940723240 ) ) ;
#14267 = ORIENTED_EDGE ( 'NONE', *, *, #9791, .T. ) ;
#14268 = CARTESIAN_POINT ( 'NONE',  ( 15.14183272437241889, 7.449999994537639836, 20.84094480462498211 ) ) ;
#14269 = CARTESIAN_POINT ( 'NONE',  ( 13.94119854578937812, 11.86236083425730925, 24.22776226481240514 ) ) ;
#14270 = DIRECTION ( 'NONE',  ( -0.000000000000000000, -1.000000000000000000, -0.000000000000000000 ) ) ;
#14271 = CARTESIAN_POINT ( 'NONE',  ( -20.75514604977248823, 48.82500000273117280, -28.56700777964554305 ) ) ;
#14272 = CARTESIAN_POINT ( 'NONE',  ( -2.162160676586881955E-15, 8.875000002731189497, -35.31076352940723240 ) ) ;
#14273 = CARTESIAN_POINT ( 'NONE',  ( -27.16883889988623935, 59.57500000273117990, 19.73931689729374739 ) ) ;
#14274 = CARTESIAN_POINT ( 'NONE',  ( 13.97622843553589966, 50.52864583333332149, -24.20753774853756113 ) ) ;
#14275 = CARTESIAN_POINT ( 'NONE',  ( 7.543491769121427382, 38.07329833425730925, -28.00173670424548433 ) ) ;
#14276 = CARTESIAN_POINT ( 'NONE',  ( -28.02196122052058413, 30.90065999907601579, -7.468012846824272799 ) ) ;
#14277 = CARTESIAN_POINT ( 'NONE',  ( 32.50000000000000711, 65.40000000546237402, 10.55989012756945122 ) ) ;
#14278 = CARTESIAN_POINT ( 'NONE',  ( -8.960552108402742093E-16, 78.37500000273119838, -14.63369212191046387 ) ) ;
#14279 = CARTESIAN_POINT ( 'NONE',  ( 19.11951029504797006, 56.96836833240936215, 19.06425588902558133 ) ) ;
#14280 = DIRECTION ( 'NONE',  ( 0.000000000000000000, 0.000000000000000000, -1.000000000000000000 ) ) ;
#14281 = CARTESIAN_POINT ( 'NONE',  ( 5.779280353836490358E-15, 53.00000000546238255, 32.49999999999999289 ) ) ;
#14282 = ORIENTED_EDGE ( 'NONE', *, *, #21552, .T. ) ;
#14283 = CARTESIAN_POINT ( 'NONE',  ( -20.75514604977248112, 39.67500000273118133, 28.56700777964554661 ) ) ;
#14284 =( BOUNDED_CURVE ( )  B_SPLINE_CURVE ( 2, ( #23193, #2600, #10325, #18227, #2078, #31246, #28840, #4824, #23537, #25931, #26103, #25425, #12553 ),
 .UNSPECIFIED., .F., .T. ) 
 B_SPLINE_CURVE_WITH_KNOTS ( ( 3, 2, 2, 2, 2, 2, 3 ),
 ( 0.3269230769230769273, 0.3282051282051282048, 0.3307692307692307598, 0.3333333333333333148, 0.3358974358974358698, 0.3384615384615384803, 0.3397435897435897578 ),
 .UNSPECIFIED. ) 
 CURVE ( )  GEOMETRIC_REPRESENTATION_ITEM ( )  RATIONAL_B_SPLINE_CURVE ( ( 0.9755282581475768211, 0.9755282581475768211, 1.000000000000000000, 0.9510565162951535312, 1.000000000000000000, 0.9510565162951535312, 1.000000000000000000, 0.9510565162951535312, 1.000000000000000000, 0.9510565162951535312, 1.000000000000000000, 0.9755282581475768211, 0.9755282581475768211 ) ) 
 REPRESENTATION_ITEM ( '' )  );
#14285 = CARTESIAN_POINT ( 'NONE',  ( 7.236395654485755280, 4.724999997268803043, 22.27133577429736988 ) ) ;
#14286 = CARTESIAN_POINT ( 'NONE',  ( 6.277390505771533514E-15, 31.00000000546236834, 34.17252228774368916 ) ) ;
#14287 = ORIENTED_EDGE ( 'NONE', *, *, #17553, .F. ) ;
#14288 = CARTESIAN_POINT ( 'NONE',  ( -26.00068869287340334, 35.34635416666666430, 15.01150461594643382 ) ) ;
#14289 = ORIENTED_EDGE ( 'NONE', *, *, #24568, .T. ) ;
#14290 = ORIENTED_EDGE ( 'NONE', *, *, #4893, .T. ) ;
#14291 = CARTESIAN_POINT ( 'NONE',  ( -2.571758278209442450E-15, -1.999999999999998224, 0.000000000000000000 ) ) ;
#14292 = CARTESIAN_POINT ( 'NONE',  ( -10.37757302488624411, 52.72500000273119980, -31.93888565452638417 ) ) ;
#14293 = CARTESIAN_POINT ( 'NONE',  ( -30.02300923189239512, 59.69531250000000711, 2.654126918244515359E-13 ) ) ;
#14294 = CARTESIAN_POINT ( 'NONE',  ( -10.04305231718578462, 8.900000005462372243, 30.90933677959249337 ) ) ;
#14295 = LINE ( 'NONE', #569, #2654 ) ;
#14296 = CARTESIAN_POINT ( 'NONE',  ( -23.41746825000000243, 14.22499999726880837, 7.608796670333725309 ) ) ;
#14297 = CARTESIAN_POINT ( 'NONE',  ( -32.50000000000000000, 56.10000000000000853, 10.55989012756946366 ) ) ;
#14298 = ADVANCED_FACE ( 'NONE', ( #15427, #7692 ), #25880, .F. ) ;
#14299 = CARTESIAN_POINT ( 'NONE',  ( 27.16883889988623935, 26.57500000273119056, -19.73931689729374384 ) ) ;
#14300 = CARTESIAN_POINT ( 'NONE',  ( 32.50000000000000000, 5.500000005462357677, -3.980102097228898626E-15 ) ) ;
#14301 = CARTESIAN_POINT ( 'NONE',  ( -0.04044903255042732459, 17.86680583240935860, -27.95245687107223986 ) ) ;
#14302 = CARTESIAN_POINT ( 'NONE',  ( 2.688165632520823219E-15, 75.37500000273118417, 14.63369212191046387 ) ) ;
#14303 = CARTESIAN_POINT ( 'NONE',  ( -4.223320258572819786E-15, 13.50000000000000355, 24.50000000000000000 ) ) ;
#14304 = DIRECTION ( 'NONE',  ( 0.000000000000000000, -1.000000000000000000, 0.000000000000000000 ) ) ;
#14305 = CARTESIAN_POINT ( 'NONE',  ( -20.08610463437157989, 7.699999999999988631, -27.64615127144129758 ) ) ;
#14306 = VERTEX_POINT ( 'NONE', #2373 ) ;
#14307 = CARTESIAN_POINT ( 'NONE',  ( -23.41746825000000243, 6.024999997268805529, -7.608796670333730638 ) ) ;
#14308 = CARTESIAN_POINT ( 'NONE',  ( 11.25946833292375793, 71.67500000273119554, 8.180482586598731842 ) ) ;
#14309 = VECTOR ( 'NONE', #8156, 1000.000000000000227 ) ;
#14310 = CARTESIAN_POINT ( 'NONE',  ( -13.97622843553588901, 38.49739583333332860, 24.20753774853756823 ) ) ;
#14311 = CARTESIAN_POINT ( 'NONE',  ( 20.75514604977249178, 67.82500000273120122, 28.56700777964553950 ) ) ;
#14312 = CARTESIAN_POINT ( 'NONE',  ( -10.37757302488624411, 32.97500000273119269, -31.93888565452638417 ) ) ;
#14313 = CARTESIAN_POINT ( 'NONE',  ( -20.75514604977248823, 15.07500000273116747, -28.56700777964554305 ) ) ;
#14314 = CARTESIAN_POINT ( 'NONE',  ( 33.58253175000000113, 10.47500000273119802, -10.91162601494193574 ) ) ;
#14315 = CARTESIAN_POINT ( 'NONE',  ( 24.18731323226247554, 63.13840250092397355, 14.01125832528285997 ) ) ;
#14316 = CARTESIAN_POINT ( 'NONE',  ( -7.505752307972844761, 55.54166666666667140, 28.01184896238304134 ) ) ;
#14317 = CARTESIAN_POINT ( 'NONE',  ( 4.300734207923757602, 78.77500000273118985, -13.23629886949340673 ) ) ;
#14318 = CARTESIAN_POINT ( 'NONE',  ( 20.08610463437157279, 47.29999999999999005, -27.64615127144129758 ) ) ;
#14319 = VECTOR ( 'NONE', #30264, 1000.000000000000000 ) ;
#14320 = CARTESIAN_POINT ( 'NONE',  ( -1.778240108872766143E-15, 63.50000000000000000, -32.49999999999999289 ) ) ;
#14321 = CARTESIAN_POINT ( 'NONE',  ( 27.16883889988623935, 52.32500000273118701, -19.73931689729374384 ) ) ;
#14322 = CARTESIAN_POINT ( 'NONE',  ( -18.94512977948576093, 1.824999997268816898, 13.76444248337722698 ) ) ;
#14323 = ORIENTED_EDGE ( 'NONE', *, *, #7038, .T. ) ;
#14324 = CARTESIAN_POINT ( 'NONE',  ( 20.75514604977248467, 58.67500000273118843, -28.56700777964554305 ) ) ;
#14325 = CARTESIAN_POINT ( 'NONE',  ( 20.08610463437158344, 16.69999999999999574, 27.64615127144129403 ) ) ;
#14326 = CARTESIAN_POINT ( 'NONE',  ( -18.94512977948575738, 3.424999997268807217, -13.76444248337723231 ) ) ;
#14327 = CARTESIAN_POINT ( 'NONE',  ( -19.11951029504763611, 29.76600666759063429, 19.06425588902592239 ) ) ;
#14328 = ORIENTED_EDGE ( 'NONE', *, *, #32304, .T. ) ;
#14329 = CARTESIAN_POINT ( 'NONE',  ( 27.16883889988623935, 28.32500000273117990, -19.73931689729374384 ) ) ;
#14330 = FACE_OUTER_BOUND ( 'NONE', #25984, .T. ) ;
#14331 = ORIENTED_EDGE ( 'NONE', *, *, #9080, .T. ) ;
#14332 = CARTESIAN_POINT ( 'NONE',  ( 15.01150461594596308, 50.52864583333333570, -26.00068869287367335 ) ) ;
#14333 = CARTESIAN_POINT ( 'NONE',  ( 33.58253175000000113, 60.47500000273118559, -10.91162601494193751 ) ) ;
#14334 = CARTESIAN_POINT ( 'NONE',  ( 5.779280353836490358E-15, 17.00000000546237899, 32.49999999999999289 ) ) ;
#14335 = CARTESIAN_POINT ( 'NONE',  ( 20.75514604977249178, 73.82500000273121543, 28.56700777964553950 ) ) ;
#14336 = CARTESIAN_POINT ( 'NONE',  ( 20.50609665441005092, 27.46875000000000000, 20.50609665440969209 ) ) ;
#14337 = CARTESIAN_POINT ( 'NONE',  ( -4.732186688966233175E-15, 5.500000000000000888, 25.76082449383753925 ) ) ;
#14338 = CARTESIAN_POINT ( 'NONE',  ( -27.16883889988623935, 5.575000002731201221, 19.73931689729374739 ) ) ;
#14339 = CARTESIAN_POINT ( 'NONE',  ( -33.58253175000000113, 15.12500000273120371, 0.000000000000000000 ) ) ;
#14340 = CARTESIAN_POINT ( 'NONE',  ( 4.300734207923757602, 72.27500000273117564, -13.23629886949340673 ) ) ;
#14341 = CARTESIAN_POINT ( 'NONE',  ( -0.04044903255044120238, 41.92930583240936215, -30.02300923189239867 ) ) ;
#14342 = CIRCLE ( 'NONE', #32957, 10.69578794377714104 ) ;
#14343 = CARTESIAN_POINT ( 'NONE',  ( -15.00000000000000000, 80.10000000000000853, 4.873795443493597723 ) ) ;
#14344 = CARTESIAN_POINT ( 'NONE',  ( -26.00068869287340334, 55.97135416666665719, 15.01150461594643559 ) ) ;
#14345 = PRODUCT_RELATED_PRODUCT_CATEGORY ( 'part', '', ( #18127 ) ) ;
#14346 = CARTESIAN_POINT ( 'NONE',  ( 0.000000000000000000, 82.00000000000001421, 0.000000000000000000 ) ) ;
#14347 = CARTESIAN_POINT ( 'NONE',  ( -4.732186688966233175E-15, 9.249999994537640546, 25.76082449383753925 ) ) ;
#14348 = CARTESIAN_POINT ( 'NONE',  ( -13.97622843553588901, 14.43489583333332682, 24.20753774853756823 ) ) ;
#14349 = CARTESIAN_POINT ( 'NONE',  ( -2.162160676586881955E-15, 40.62500000273120548, -35.31076352940723240 ) ) ;
#14350 = CARTESIAN_POINT ( 'NONE',  ( -8.601468415847515203, 75.17500000273118133, 11.83890561707634959 ) ) ;
#14351 = CARTESIAN_POINT ( 'NONE',  ( 27.16883889988624290, 52.17500000273118843, 19.73931689729373673 ) ) ;
#14352 = CARTESIAN_POINT ( 'NONE',  ( -33.58253175000000113, 29.47500000273117848, 10.91162601494193929 ) ) ;
#14353 = CARTESIAN_POINT ( 'NONE',  ( -17.29030653276320351, 16.99999999999998579, 17.35785989121602668 ) ) ;
#14354 = CARTESIAN_POINT ( 'NONE',  ( 6.988114217768294445, 31.19270833333333215, 26.07999730980477437 ) ) ;
#14355 = CARTESIAN_POINT ( 'NONE',  ( -3.880418787951136483, 14.30125427608446920, -24.50000000000000000 ) ) ;
#14356 = CARTESIAN_POINT ( 'NONE',  ( -23.09401076758502924, 96.00000000000002842, 5.354274672883389237E-15 ) ) ;
#14357 = CARTESIAN_POINT ( 'NONE',  ( -10.04305231718579172, 69.59999999999998010, -30.90933677959248982 ) ) ;
#14358 = CARTESIAN_POINT ( 'NONE',  ( 18.94512977948575738, 10.42499999726881299, 13.76444248337723408 ) ) ;
#14359 = CARTESIAN_POINT ( 'NONE',  ( 15.04653450569339945, 29.61159749907602290, 25.98046417659831775 ) ) ;
#14360 = CARTESIAN_POINT ( 'NONE',  ( -19.82091636218621034, 10.54999999453762349, -14.40073868116559552 ) ) ;
#14361 = CARTESIAN_POINT ( 'NONE',  ( -19.11951029504797006, 41.49961833240934794, -19.06425588902558133 ) ) ;
#14362 = CARTESIAN_POINT ( 'NONE',  ( 0.000000000000000000, 80.00000000000001421, 0.000000000000000000 ) ) ;
#14363 = CARTESIAN_POINT ( 'NONE',  ( -20.75514604977248112, 15.42500000273118665, 28.56700777964554661 ) ) ;
#14364 = CARTESIAN_POINT ( 'NONE',  ( 1.507698388325705758E-15, 7.624999997268814056, -24.62258325217400312 ) ) ;
#14365 = CARTESIAN_POINT ( 'NONE',  ( 26.07999730980477437, 57.83333333333333570, -6.988114217768290004 ) ) ;
#14366 = ORIENTED_EDGE ( 'NONE', *, *, #15463, .F. ) ;
#14367 = CARTESIAN_POINT ( 'NONE',  ( -33.58253175000000113, 57.02500000273118275, -10.91162601494193218 ) ) ;
#14368 = CARTESIAN_POINT ( 'NONE',  ( 33.58253175000000823, 26.27500000273119340, 10.91162601494192863 ) ) ;
#14369 = VERTEX_POINT ( 'NONE', #31028 ) ;
#14370 = CARTESIAN_POINT ( 'NONE',  ( -30.02300923189239512, 28.75781249999999645, 2.654126918244515359E-13 ) ) ;
#14371 = CARTESIAN_POINT ( 'NONE',  ( 30.02300923189239867, 21.60194416759064495, 0.04044903254992252006 ) ) ;
#14372 = CARTESIAN_POINT ( 'NONE',  ( 7.570916362186207671, 19.34999999453762598, 23.30088464923126779 ) ) ;
#14373 = CARTESIAN_POINT ( 'NONE',  ( 1.507698388325705758E-15, 5.124999997268805174, -24.62258325217400312 ) ) ;
#14374 = CARTESIAN_POINT ( 'NONE',  ( -27.16883889988623935, 23.57500000273119056, 19.73931689729374739 ) ) ;
#14375 = CARTESIAN_POINT ( 'NONE',  ( 32.50000000000000000, 29.60000000546238041, -10.55989012756945833 ) ) ;
#14376 = CARTESIAN_POINT ( 'NONE',  ( -10.04305231718579172, 71.59999999999999432, -30.90933677959248982 ) ) ;
#14377 = CARTESIAN_POINT ( 'NONE',  ( 0.000000000000000000, 70.00000000000000000, 0.000000000000000000 ) ) ;
#14378 = CARTESIAN_POINT ( 'NONE',  ( -8.749005742281003251, 74.00000000000004263, 11.56706244653782001 ) ) ;
#14379 = CARTESIAN_POINT ( 'NONE',  ( -14.97647472619946285, 54.83111083425730214, -26.02091320914851025 ) ) ;
#14380 = CARTESIAN_POINT ( 'NONE',  ( 6.486482029760649416E-15, 33.87500000273118417, 35.31076352940723240 ) ) ;
#14381 = CARTESIAN_POINT ( 'NONE',  ( -33.58253175000000113, 57.12500000273116996, 0.000000000000000000 ) ) ;
#14382 = CARTESIAN_POINT ( 'NONE',  ( 7.505752307973351023, 31.19270833333333215, 28.01184896238290278 ) ) ;
#14383 =( BOUNDED_CURVE ( )  B_SPLINE_CURVE ( 2, ( #2006, #22951, #7671, #28268, #4754, #15231, #18157, #25694, #28599, #33930, #7504, #7840, #10421 ),
 .UNSPECIFIED., .F., .T. ) 
 B_SPLINE_CURVE_WITH_KNOTS ( ( 3, 2, 2, 2, 2, 2, 3 ),
 ( 0.2500000000000000000, 0.2600000000000000089, 0.2800000000000000266, 0.2999999999999999889, 0.3200000000000000067, 0.3400000000000000244, 0.3500000000000000333 ),
 .UNSPECIFIED. ) 
 CURVE ( )  GEOMETRIC_REPRESENTATION_ITEM ( )  RATIONAL_B_SPLINE_CURVE ( ( 0.9755282581475768211, 0.9755282581475768211, 1.000000000000000000, 0.9510565162951535312, 1.000000000000000000, 0.9510565162951535312, 1.000000000000000000, 0.9510565162951535312, 1.000000000000000000, 0.9510565162951535312, 1.000000000000000000, 0.9755282581475767101, 0.9755282581475768211 ) ) 
 REPRESENTATION_ITEM ( '' )  );
#14384 = SURFACE_STYLE_USAGE ( .BOTH. , #26756 ) ;
#14385 = CONICAL_SURFACE ( 'NONE', #3970, 24.50000000000000000, 0.7853981633974463916 ) ;
#14386 = CARTESIAN_POINT ( 'NONE',  ( -7.236395654485763274, 8.524999997268800200, 22.27133577429736633 ) ) ;
#14387 = CARTESIAN_POINT ( 'NONE',  ( 20.08610463437158344, 12.70000000000000639, 27.64615127144129403 ) ) ;
#14388 = CARTESIAN_POINT ( 'NONE',  ( 7.570916362186207671, 11.59999999999999964, 23.30088464923126779 ) ) ;
#14389 = CARTESIAN_POINT ( 'NONE',  ( -26.09010956794245217, 48.08815999907601935, -6.950374756619243755 ) ) ;
#14390 =( BOUNDED_CURVE ( )  B_SPLINE_CURVE ( 2, ( #18078, #22162, #3626, #6194, #32605, #29368, #29525, #16506, #24556, #6538, #8937, #13930, #14264 ),
 .UNSPECIFIED., .F., .T. ) 
 B_SPLINE_CURVE_WITH_KNOTS ( ( 3, 2, 2, 2, 2, 2, 3 ),
 ( 0.2499999999999999722, 0.2555555555555555358, 0.2666666666666666630, 0.2777777777777777901, 0.2888888888888888618, 0.2999999999999999889, 0.3055555555555555802 ),
 .UNSPECIFIED. ) 
 CURVE ( )  GEOMETRIC_REPRESENTATION_ITEM ( )  RATIONAL_B_SPLINE_CURVE ( ( 0.9755282581475768211, 0.9755282581475768211, 1.000000000000000000, 0.9510565162951535312, 1.000000000000000000, 0.9510565162951535312, 1.000000000000000000, 0.9510565162951535312, 1.000000000000000000, 0.9510565162951535312, 1.000000000000000000, 0.9755282581475765991, 0.9755282581475767101 ) ) 
 REPRESENTATION_ITEM ( '' )  );
#14391 = CARTESIAN_POINT ( 'NONE',  ( 27.16883889988624290, 59.92500000273118133, 19.73931689729373673 ) ) ;
#14392 = CARTESIAN_POINT ( 'NONE',  ( -27.16883889988623935, 45.57500000273117990, 19.73931689729374739 ) ) ;
#14393 = CARTESIAN_POINT ( 'NONE',  ( 18.94512977948576093, 8.824999997268822227, -13.76444248337722875 ) ) ;
#14394 = ADVANCED_FACE ( 'NONE', ( #20757 ), #28661, .T. ) ;
#14395 = DIRECTION ( 'NONE',  ( 0.000000000000000000, -1.000000000000000000, 0.000000000000000000 ) ) ;
#14396 = CARTESIAN_POINT ( 'NONE',  ( -1.778240108872766143E-15, 49.50000000000000000, -32.49999999999999289 ) ) ;
#14397 = CARTESIAN_POINT ( 'NONE',  ( -7.025853678916393008, 36.35454833425730925, 26.06988505166735592 ) ) ;
#14398 = CARTESIAN_POINT ( 'NONE',  ( -8.705037036007741591, 16.99999999999998224, -22.19839023265693356 ) ) ;
#14399 = CARTESIAN_POINT ( 'NONE',  ( -10.04305231718578462, 42.39999999999999147, 30.90933677959249337 ) ) ;
#14400 = CARTESIAN_POINT ( 'NONE',  ( -27.16883889988623935, 29.32500000273117990, 19.73931689729374739 ) ) ;
#14401 = CARTESIAN_POINT ( 'NONE',  ( 3.980102097228898626E-15, 80.00000000000001421, 32.50000000000000000 ) ) ;
#14402 = CARTESIAN_POINT ( 'NONE',  ( 10.04305231718579705, 55.10000000546237686, 30.90933677959248982 ) ) ;
#14403 = EDGE_CURVE ( 'NONE', #29888, #9319, #6560, .T. ) ;
#14404 = CARTESIAN_POINT ( 'NONE',  ( -32.50000000000000000, 30.50000000546237899, 0.000000000000000000 ) ) ;
#14405 = ADVANCED_FACE ( 'NONE', ( #15603 ), #4604, .T. ) ;
#14406 = CARTESIAN_POINT ( 'NONE',  ( 14.97647472619900455, 52.52826416574268364, -26.02091320914876960 ) ) ;
#14407 = CARTESIAN_POINT ( 'NONE',  ( 20.08610463437157279, 47.80000000546239391, -27.64615127144129758 ) ) ;
#14408 = CARTESIAN_POINT ( 'NONE',  ( 10.37757302488624767, 33.72500000273117848, 31.93888565452638417 ) ) ;
#14409 = CARTESIAN_POINT ( 'NONE',  ( 26.07999730980477437, 30.33333333333332860, -6.988114217768290004 ) ) ;
#14410 = AXIS2_PLACEMENT_3D ( 'NONE', #33574, #15745, #12299 ) ;
#14411 = EDGE_CURVE ( 'NONE', #29507, #2692, #26058, .T. ) ;
#14412 = CARTESIAN_POINT ( 'NONE',  ( -20.75514604977248112, 73.42500000273118133, 28.56700777964554661 ) ) ;
#14413 = CARTESIAN_POINT ( 'NONE',  ( 26.00068869287340334, 26.75260416666666430, -15.01150461594642316 ) ) ;
#14414 = DIRECTION ( 'NONE',  ( -1.000000000000000000, 0.000000000000000000, 0.000000000000000000 ) ) ;
#14415 = VERTEX_POINT ( 'NONE', #23320 ) ;
#14416 = CARTESIAN_POINT ( 'NONE',  ( 25.98046417659858420, 49.38840250092398776, 15.04653450569292872 ) ) ;
#14417 = CARTESIAN_POINT ( 'NONE',  ( -2.092463501923844636E-15, 10.00000000546237722, -34.17252228774368916 ) ) ;
#14418 = CARTESIAN_POINT ( 'NONE',  ( 28.01184896238304134, 64.99479166666665719, 7.505752307972846538 ) ) ;
#14419 = CARTESIAN_POINT ( 'NONE',  ( 20.08610463437157279, 21.29999999999999716, -27.64615127144129758 ) ) ;
#14420 = CARTESIAN_POINT ( 'NONE',  ( -10.37757302488623701, 43.77500000273118275, 31.93888565452638417 ) ) ;
#14421 = CARTESIAN_POINT ( 'NONE',  ( -26.29305231718579350, 48.30000000546236549, -19.10302069950537884 ) ) ;
#14422 = CARTESIAN_POINT ( 'NONE',  ( -12.13525491562420910, 80.19999999999998863, 8.816778784387098611 ) ) ;
#14423 = CARTESIAN_POINT ( 'NONE',  ( -33.58253175000000113, 31.12500000273119127, 0.000000000000000000 ) ) ;
#14424 = CARTESIAN_POINT ( 'NONE',  ( -5.147494310547430452, 62.05125428700922185, -32.49999999999999289 ) ) ;
#14425 = CARTESIAN_POINT ( 'NONE',  ( 20.75514604977249178, 54.07500000273118701, 28.56700777964553950 ) ) ;
#14426 = CARTESIAN_POINT ( 'NONE',  ( -10.04305231718578462, 34.39999999999999858, 30.90933677959249337 ) ) ;
#14427 = CARTESIAN_POINT ( 'NONE',  ( -10.04305231718579172, 35.59999999999999432, -30.90933677959248982 ) ) ;
#14428 = CARTESIAN_POINT ( 'NONE',  ( 23.41746825000000243, 8.724999997268806595, -7.608796670333727974 ) ) ;
#14429 = CARTESIAN_POINT ( 'NONE',  ( 10.37757302488624767, 73.72500000273119269, 31.93888565452638417 ) ) ;
#14430 = LINE ( 'NONE', #8934, #23905 ) ;
#14431 = CARTESIAN_POINT ( 'NONE',  ( 11.25946833292375793, 80.57500000273121543, -8.180482586598735395 ) ) ;
#14432 = CARTESIAN_POINT ( 'NONE',  ( 27.16883889988624290, 64.17500000273118133, 19.73931689729373673 ) ) ;
#14433 = CARTESIAN_POINT ( 'NONE',  ( -9.657523855033125146E-16, 79.75000000546238255, -15.77193336357400710 ) ) ;
#14434 = EDGE_LOOP ( 'NONE', ( #10859, #5769, #30515, #1214 ) ) ;
#14435 = CARTESIAN_POINT ( 'NONE',  ( -33.58253175000000113, 1.250000002731177506, 0.000000000000000000 ) ) ;
#14436 = CARTESIAN_POINT ( 'NONE',  ( 7.025853678916403666, 10.57329833425730747, -26.06988505166735237 ) ) ;
#14437 = CARTESIAN_POINT ( 'NONE',  ( 0.000000000000000000, 74.00000000000001421, 0.000000000000000000 ) ) ;
#14438 = CARTESIAN_POINT ( 'NONE',  ( 20.75514604977248467, 48.42500000273119554, -28.56700777964554305 ) ) ;
#14439 = CARTESIAN_POINT ( 'NONE',  ( -27.16883889988623935, 1.575000002731183457, 19.73931689729374739 ) ) ;
#14440 = CARTESIAN_POINT ( 'NONE',  ( -33.58253175000000113, 59.27500000273119696, -10.91162601494193041 ) ) ;
#14441 = CARTESIAN_POINT ( 'NONE',  ( 13.97622843553633842, 51.67447916666665719, 24.20753774853730889 ) ) ;
#14442 = CARTESIAN_POINT ( 'NONE',  ( 26.02091320914851025, 38.50298583425730925, -14.97647472619946463 ) ) ;
#14443 = CARTESIAN_POINT ( 'NONE',  ( 25.98046417659831775, 25.31472249907601579, -15.04653450569338879 ) ) ;
#14444 = CARTESIAN_POINT ( 'NONE',  ( 20.08610463437158344, 67.20000000546235697, 27.64615127144129403 ) ) ;
#14445 = CARTESIAN_POINT ( 'NONE',  ( 11.25946833292375793, 72.07500000273120122, -8.180482586598735395 ) ) ;
#14446 = CARTESIAN_POINT ( 'NONE',  ( -14.01125832528328985, 58.83034749907602645, -24.18731323226223040 ) ) ;
#14447 = CARTESIAN_POINT ( 'NONE',  ( -32.50000000000000000, 54.10000000000000853, 10.55989012756946366 ) ) ;
#14448 = CARTESIAN_POINT ( 'NONE',  ( 32.50000000000000000, 13.50000000546236478, -3.980102097228898626E-15 ) ) ;
#14449 = ORIENTED_EDGE ( 'NONE', *, *, #9343, .F. ) ;
#14450 = EDGE_CURVE ( 'NONE', #33174, #17621, #9873, .T. ) ;
#14451 = CARTESIAN_POINT ( 'NONE',  ( -33.58253175000000113, 43.27500000273117564, -10.91162601494193218 ) ) ;
#14452 = CYLINDRICAL_SURFACE ( 'NONE', #16829, 32.50000000000000000 ) ;
#14453 = CARTESIAN_POINT ( 'NONE',  ( 20.08610463437158344, 31.20000000546238894, 27.64615127144129403 ) ) ;
#14454 = VERTEX_POINT ( 'NONE', #12765 ) ;
#14455 = VECTOR ( 'NONE', #16565, 1000.000000000000114 ) ;
#14456 = CARTESIAN_POINT ( 'NONE',  ( 15.01150461594643204, 31.04947916666666075, 26.00068869287340334 ) ) ;
#14457 = ORIENTED_EDGE ( 'NONE', *, *, #805, .T. ) ;
#14458 = CARTESIAN_POINT ( 'NONE',  ( -24.50000000000000000, 12.74999999453763166, -3.000384657911015469E-15 ) ) ;
#14459 = CARTESIAN_POINT ( 'NONE',  ( 6.486482029760649416E-15, 47.62500000273118417, 35.31076352940723240 ) ) ;
#14460 = CARTESIAN_POINT ( 'NONE',  ( 15.01150461594596308, 60.84114583333332860, -26.00068869287367335 ) ) ;
#14461 = APPLICATION_CONTEXT ( 'automotive_design' ) ;
#14462 = CARTESIAN_POINT ( 'NONE',  ( 20.08610463437158344, 9.200000005462387165, 27.64615127144129403 ) ) ;
#14463 = CARTESIAN_POINT ( 'NONE',  ( 6.486482029760648627E-15, 65.62500000273116996, 35.31076352940722529 ) ) ;
#14464 = CARTESIAN_POINT ( 'NONE',  ( 23.41746824999999887, 13.02499999726881619, 7.608796670333735079 ) ) ;
#14465 = CARTESIAN_POINT ( 'NONE',  ( -32.50000000000000000, 51.99999999999999289, 0.000000000000000000 ) ) ;
#14466 = CARTESIAN_POINT ( 'NONE',  ( 27.16883889988624290, 22.17500000273120264, 19.73931689729373673 ) ) ;
#14467 = CARTESIAN_POINT ( 'NONE',  ( 5.779280353836490358E-15, 25.00000000546237899, 32.49999999999999289 ) ) ;
#14468 = CARTESIAN_POINT ( 'NONE',  ( -14.01125832528328985, 17.58034749907602290, -24.18731323226223040 ) ) ;
#14469 = CARTESIAN_POINT ( 'NONE',  ( 13.91746824999999887, 75.87500000273116996, -1.704398294459741270E-15 ) ) ;
#14470 = LINE ( 'NONE', #17047, #20079 ) ;
#14471 = CARTESIAN_POINT ( 'NONE',  ( -26.29305231718579350, 33.79999999999999716, -19.10302069950537884 ) ) ;
#14472 = CARTESIAN_POINT ( 'NONE',  ( -26.29305231718578995, 2.199999999999993516, 19.10302069950538595 ) ) ;
#14473 = EDGE_LOOP ( 'NONE', ( #4703, #22141, #22100, #13324 ) ) ;
#14474 = CARTESIAN_POINT ( 'NONE',  ( 7.236395654485760609, 5.524999997268825958, -22.27133577429736633 ) ) ;
#14475 = CARTESIAN_POINT ( 'NONE',  ( 26.29305231718578995, 71.70000000546239960, -19.10302069950538240 ) ) ;
#14476 = CARTESIAN_POINT ( 'NONE',  ( -19.09188309203694445, 42.93750000000000000, -19.09188309203661049 ) ) ;
#14477 = CARTESIAN_POINT ( 'NONE',  ( -33.58253175000000113, 65.12500000273118417, 0.000000000000000000 ) ) ;
#14478 = CARTESIAN_POINT ( 'NONE',  ( 10.37757302488624767, 25.97500000273118914, 31.93888565452638417 ) ) ;
#14479 = VECTOR ( 'NONE', #11979, 1000.000000000000000 ) ;
#14480 = CARTESIAN_POINT ( 'NONE',  ( -33.58253175000000113, 17.47500000273117848, 10.91162601494193929 ) ) ;
#14481 = CARTESIAN_POINT ( 'NONE',  ( 10.37757302488624056, 10.77500000273118275, -31.93888565452638417 ) ) ;
#14482 = CARTESIAN_POINT ( 'NONE',  ( -28.00173670424549499, 13.15142333425730925, -7.543491769121417612 ) ) ;
#14483 = CARTESIAN_POINT ( 'NONE',  ( -28.01184896238290278, 56.11458333333332860, 7.505752307973363457 ) ) ;
#14484 =( BOUNDED_CURVE ( )  B_SPLINE_CURVE ( 2, ( #14186, #27730, #22752, #14520, #4218, #12279, #23093, #27903, #14692, #33027, #6621, #33556, #1627 ),
 .UNSPECIFIED., .F., .T. ) 
 B_SPLINE_CURVE_WITH_KNOTS ( ( 3, 2, 2, 2, 2, 2, 3 ),
 ( 0.8055555555555555802, 0.8111111111111111160, 0.8222222222222221877, 0.8333333333333333703, 0.8444444444444444420, 0.8555555555555555136, 0.8611111111111111605 ),
 .UNSPECIFIED. ) 
 CURVE ( )  GEOMETRIC_REPRESENTATION_ITEM ( )  RATIONAL_B_SPLINE_CURVE ( ( 0.9755282581475768211, 0.9755282581475768211, 1.000000000000000000, 0.9510565162951535312, 1.000000000000000000, 0.9510565162951535312, 1.000000000000000000, 0.9510565162951535312, 1.000000000000000000, 0.9510565162951535312, 1.000000000000000000, 0.9755282581475765991, 0.9755282581475768211 ) ) 
 REPRESENTATION_ITEM ( '' )  );
#14485 = CARTESIAN_POINT ( 'NONE',  ( 11.25946833292375793, 80.17500000273119554, 8.180482586598731842 ) ) ;
#14486 = CARTESIAN_POINT ( 'NONE',  ( 6.277390505771533514E-15, 48.50000000000000711, 34.17252228774368916 ) ) ;
#14487 = CARTESIAN_POINT ( 'NONE',  ( 10.04305231718578817, 63.40000000000001279, -30.90933677959249337 ) ) ;
#14488 = CARTESIAN_POINT ( 'NONE',  ( 33.58253175000000823, 54.02500000273118985, 10.91162601494192685 ) ) ;
#14489 = CARTESIAN_POINT ( 'NONE',  ( 23.41746824999999887, 19.12499999726882649, 0.000000000000000000 ) ) ;
#14490 = ORIENTED_EDGE ( 'NONE', *, *, #24987, .F. ) ;
#14491 = CARTESIAN_POINT ( 'NONE',  ( -33.58253175000000113, 63.27500000273118985, -10.91162601494193218 ) ) ;
#14492 = DIRECTION ( 'NONE',  ( -0.000000000000000000, -1.000000000000000000, -0.000000000000000000 ) ) ;
#14493 = CARTESIAN_POINT ( 'NONE',  ( 14.47279130897151589, 12.32499999726880802, 19.92008829642072953 ) ) ;
#14494 = CARTESIAN_POINT ( 'NONE',  ( 24.22776226481241224, 31.62798583425730925, -13.94119854578936923 ) ) ;
#14495 = EDGE_CURVE ( 'NONE', #33570, #8435, #12420, .T. ) ;
#14496 = VERTEX_POINT ( 'NONE', #25116 ) ;
#14497 = CARTESIAN_POINT ( 'NONE',  ( 10.37757302488624056, 32.52500000273118985, -31.93888565452638417 ) ) ;
#14498 = CARTESIAN_POINT ( 'NONE',  ( 5.779280353836490358E-15, 35.00000000546238255, 32.49999999999999289 ) ) ;
#14499 = ORIENTED_EDGE ( 'NONE', *, *, #3289, .F. ) ;
#14500 = CARTESIAN_POINT ( 'NONE',  ( -20.50609665441004736, 56.68749999999998579, -20.50609665440969565 ) ) ;
#14501 = CARTESIAN_POINT ( 'NONE',  ( 33.58253175000000113, 62.37500000273119127, -4.112674001490185761E-15 ) ) ;
#14502 = CARTESIAN_POINT ( 'NONE',  ( 1.836970198721029589E-15, 82.00000000000001421, 15.00000000000000000 ) ) ;
#14503 = CARTESIAN_POINT ( 'NONE',  ( -33.58253175000000113, 69.02500000273118985, -10.91162601494193218 ) ) ;
#14504 = CARTESIAN_POINT ( 'NONE',  ( -20.50609665440969209, 31.76562499999999289, 20.50609665441005092 ) ) ;
#14505 = CARTESIAN_POINT ( 'NONE',  ( -24.50000000000000355, 14.89999999999999680, -7.960532557706207157 ) ) ;
#14506 = CARTESIAN_POINT ( 'NONE',  ( 0.000000000000000000, 74.00000000000001421, 0.000000000000000000 ) ) ;
#14507 = CARTESIAN_POINT ( 'NONE',  ( -33.58253175000000113, 19.12500000273118062, 0.000000000000000000 ) ) ;
#14508 = CARTESIAN_POINT ( 'NONE',  ( 13.91746825000000065, 71.77500000273120406, 4.522059556121115875 ) ) ;
#14509 = CARTESIAN_POINT ( 'NONE',  ( 26.02091320914876960, 46.51263916574269786, 14.97647472619900455 ) ) ;
#14510 = CARTESIAN_POINT ( 'NONE',  ( 9.270509831248425314, 78.70000000000000284, 12.75976212528059683 ) ) ;
#14511 = CARTESIAN_POINT ( 'NONE',  ( 20.50609665441005092, 58.40625000000000711, 20.50609665440969209 ) ) ;
#14512 = CARTESIAN_POINT ( 'NONE',  ( 4.349545668204547685E-15, -58.51673569255127205, 0.000000000000000000 ) ) ;
#14513 = CARTESIAN_POINT ( 'NONE',  ( 24.50000000000000355, 3.649999994537613812, 7.960532557706212486 ) ) ;
#14514 = CARTESIAN_POINT ( 'NONE',  ( 15.00000000000000355, 75.15000000546237402, 4.873795443493592394 ) ) ;
#14515 = CARTESIAN_POINT ( 'NONE',  ( 26.07999730980477437, 16.58333333333333215, -6.988114217768290004 ) ) ;
#14516 = CARTESIAN_POINT ( 'NONE',  ( 20.75514604977249178, 37.82500000273117280, 28.56700777964553950 ) ) ;
#14517 = CARTESIAN_POINT ( 'NONE',  ( 4.300734207923761154, 75.47500000273116427, 13.23629886949340495 ) ) ;
#14518 = CARTESIAN_POINT ( 'NONE',  ( 33.58253175000000113, 52.47500000273117138, -10.91162601494193751 ) ) ;
#14519 = CARTESIAN_POINT ( 'NONE',  ( 33.58253175000000113, 30.37500000273119127, -4.112674001490185761E-15 ) ) ;
#14520 = CARTESIAN_POINT ( 'NONE',  ( -15.14183272437242067, 16.44999999453761674, -20.84094480462497856 ) ) ;
#14521 = CARTESIAN_POINT ( 'NONE',  ( -32.50000000000000000, 8.500000005462361230, 0.000000000000000000 ) ) ;
#14522 =( BOUNDED_CURVE ( )  B_SPLINE_CURVE ( 2, ( #4697, #17932, #7447, #4871, #11043, #8452, #26655, #31461, #20844, #18942, #21509, #29387, #18610 ),
 .UNSPECIFIED., .F., .T. ) 
 B_SPLINE_CURVE_WITH_KNOTS ( ( 3, 2, 2, 2, 2, 2, 3 ),
 ( 0.7500000000000000000, 0.7555555555555555358, 0.7666666666666667185, 0.7777777777777777901, 0.7888888888888888618, 0.8000000000000000444, 0.8055555555555555802 ),
 .UNSPECIFIED. ) 
 CURVE ( )  GEOMETRIC_REPRESENTATION_ITEM ( )  RATIONAL_B_SPLINE_CURVE ( ( 0.9755282581475768211, 0.9755282581475768211, 1.000000000000000000, 0.9510565162951535312, 1.000000000000000000, 0.9510565162951535312, 1.000000000000000000, 0.9510565162951535312, 1.000000000000000000, 0.9510565162951535312, 1.000000000000000000, 0.9755282581475768211, 0.9755282581475768211 ) ) 
 REPRESENTATION_ITEM ( '' )  );
#14523 = CARTESIAN_POINT ( 'NONE',  ( 9.270509831248421762, 81.29999999999999716, -12.75976212528059861 ) ) ;
#14524 = CARTESIAN_POINT ( 'NONE',  ( 10.04305231718579705, 68.59999999999998010, 30.90933677959248982 ) ) ;
#14525 = CARTESIAN_POINT ( 'NONE',  ( -18.94512977948575738, 9.424999997268812990, -13.76444248337723231 ) ) ;
#14526 = CARTESIAN_POINT ( 'NONE',  ( -26.02091320914878025, 24.16888916574269075, -14.97647472619899389 ) ) ;
#14527 = CARTESIAN_POINT ( 'NONE',  ( -2.375766604868048137, 78.44874571845311095, 14.99999999999999822 ) ) ;
#14528 = CARTESIAN_POINT ( 'NONE',  ( -24.22776226481266448, 34.48138916574268364, -13.94119854578892514 ) ) ;
#14529 =( NAMED_UNIT ( * ) SI_UNIT ( $, .STERADIAN. ) SOLID_ANGLE_UNIT ( ) );
#14530 = CARTESIAN_POINT ( 'NONE',  ( 20.75514604977248467, 16.42500000273118133, -28.56700777964554305 ) ) ;
#14531 = CARTESIAN_POINT ( 'NONE',  ( 14.47279130897151589, 10.82499999726880091, 19.92008829642072953 ) ) ;
#14532 = CARTESIAN_POINT ( 'NONE',  ( -27.95245687107222921, 63.13281250000000000, 2.498001805406602216E-13 ) ) ;
#14533 = ORIENTED_EDGE ( 'NONE', *, *, #33247, .T. ) ;
#14534 = CARTESIAN_POINT ( 'NONE',  ( -27.16883889988623935, 47.32500000273119412, 19.73931689729374739 ) ) ;
#14535 = CARTESIAN_POINT ( 'NONE',  ( 10.37757302488624056, 20.77500000273117919, -31.93888565452638417 ) ) ;
#14536 = EDGE_CURVE ( 'NONE', #30261, #10957, #4154, .T. ) ;
#14537 = EDGE_CURVE ( 'NONE', #7360, #11875, #14687, .T. ) ;
#14538 = ORIENTED_EDGE ( 'NONE', *, *, #10848, .F. ) ;
#14539 = CARTESIAN_POINT ( 'NONE',  ( -7.505752307973343918, 32.91145833333332860, -28.01184896238290989 ) ) ;
#14540 = CARTESIAN_POINT ( 'NONE',  ( 7.468012846824777284, 29.19309000092397000, 28.02196122052045268 ) ) ;
#14541 = AXIS2_PLACEMENT_3D ( 'NONE', #13176, #2545, #18171 ) ;
#14542 = CARTESIAN_POINT ( 'NONE',  ( -26.29305231718579350, 9.800000000000002487, -19.10302069950537884 ) ) ;
#14543 = CARTESIAN_POINT ( 'NONE',  ( -15.14183272437242600, 17.04999999453762527, 20.84094480462497856 ) ) ;
#14544 = CARTESIAN_POINT ( 'NONE',  ( 23.41746825000000243, 4.724999997268818142, -7.608796670333727974 ) ) ;
#14545 = CARTESIAN_POINT ( 'NONE',  ( 27.16883889988624290, 20.17500000273120264, 19.73931689729373673 ) ) ;
#14546 = CARTESIAN_POINT ( 'NONE',  ( -2.092463501923844636E-15, 24.00000000546238610, -34.17252228774368916 ) ) ;
#14547 = CARTESIAN_POINT ( 'NONE',  ( -32.50000000000000000, 72.09999999999999432, 10.55989012756946366 ) ) ;
#14548 = CARTESIAN_POINT ( 'NONE',  ( 5.147494310547434893, 33.05125428700922185, 32.49999999999999289 ) ) ;
#14549 = DIRECTION ( 'NONE',  ( -0.4999999999999997224, 0.000000000000000000, 0.8660254037844388186 ) ) ;
#14550 = CARTESIAN_POINT ( 'NONE',  ( -30.02300923189239867, 57.69569416759065206, -0.04044903254991731589 ) ) ;
#14551 = CARTESIAN_POINT ( 'NONE',  ( -27.16883889988624290, 39.17500000273118843, -19.73931689729374028 ) ) ;
#14552 = CARTESIAN_POINT ( 'NONE',  ( 33.58253175000000823, 56.02500000273118275, 10.91162601494192685 ) ) ;
#14553 = CARTESIAN_POINT ( 'NONE',  ( -20.50609665440969209, 35.20312500000000000, 20.50609665441005092 ) ) ;
#14554 = CARTESIAN_POINT ( 'NONE',  ( 23.41746825000000243, 13.22499999726881192, -7.608796670333727974 ) ) ;
#14555 = CARTESIAN_POINT ( 'NONE',  ( -20.08610463437156923, 14.29999999999998472, 27.64615127144130113 ) ) ;
#14556 = CARTESIAN_POINT ( 'NONE',  ( -24.50000000000000355, 16.89999999999998437, -7.960532557706207157 ) ) ;
#14557 = EDGE_CURVE ( 'NONE', #5893, #5805, #30597, .T. ) ;
#14558 = CARTESIAN_POINT ( 'NONE',  ( 14.01125832528330051, 43.36159749907602645, 24.18731323226221974 ) ) ;
#14559 = CARTESIAN_POINT ( 'NONE',  ( -33.58253175000000113, 55.12500000273118417, 0.000000000000000000 ) ) ;
#14560 = AXIS2_PLACEMENT_3D ( 'NONE', #9826, #4334, #14807 ) ;
#14561 = CARTESIAN_POINT ( 'NONE',  ( 33.58253175000000113, 48.37500000273120548, -4.112674001490185761E-15 ) ) ;
#14562 = CARTESIAN_POINT ( 'NONE',  ( 14.47279130897151767, 8.324999997268818674, 19.92008829642072953 ) ) ;
#14563 = CARTESIAN_POINT ( 'NONE',  ( 0.000000000000000000, 52.00000000000000711, 32.50000000000000000 ) ) ;
#14564 = CARTESIAN_POINT ( 'NONE',  ( -40.00000000000000711, 66.99999999999998579, -23.09401076758504345 ) ) ;
#14565 = CARTESIAN_POINT ( 'NONE',  ( -24.18731323226248264, 51.10715250092397355, -14.01125832528284931 ) ) ;
#14566 = CARTESIAN_POINT ( 'NONE',  ( -10.52618891537850310, 16.99999999999997868, -21.44545275267361006 ) ) ;
#14567 = CARTESIAN_POINT ( 'NONE',  ( -33.58253175000000113, 19.02500000273118630, -10.91162601494193218 ) ) ;
#14568 = CARTESIAN_POINT ( 'NONE',  ( 10.04305231718579705, 66.59999999999999432, 30.90933677959248982 ) ) ;
#14569 = CARTESIAN_POINT ( 'NONE',  ( 32.50000000000000000, 55.60000000546237686, -10.55989012756945833 ) ) ;
#14570 = CARTESIAN_POINT ( 'NONE',  ( -20.08610463437157989, 78.20000000546235697, -27.64615127144129758 ) ) ;
#14571 = CARTESIAN_POINT ( 'NONE',  ( -30.02300923189239867, 61.69493083240936926, 0.04044903255044988294 ) ) ;
#14572 = CARTESIAN_POINT ( 'NONE',  ( 26.29305231718579350, 41.30000000546237260, 19.10302069950537529 ) ) ;
#14573 = CARTESIAN_POINT ( 'NONE',  ( 15.00000000000000355, 71.15000000546237402, 4.873795443493592394 ) ) ;
#14574 = CARTESIAN_POINT ( 'NONE',  ( -27.16883889988623935, 33.32500000273120122, 19.73931689729374739 ) ) ;
#14575 = CARTESIAN_POINT ( 'NONE',  ( 24.20753774853756113, 30.76302083333332504, 13.97622843553589789 ) ) ;
#14576 = ORIENTED_EDGE ( 'NONE', *, *, #8939, .F. ) ;
#14577 = CARTESIAN_POINT ( 'NONE',  ( 33.58253175000000113, 66.12500000273118417, -4.112674001490185761E-15 ) ) ;
#14578 = CARTESIAN_POINT ( 'NONE',  ( 28.01184896238290278, 44.08333333333332860, -7.505752307973347470 ) ) ;
#14579 = CARTESIAN_POINT ( 'NONE',  ( 3.980102097228898626E-15, 80.00000000000001421, 32.50000000000000000 ) ) ;
#14580 = EDGE_LOOP ( 'NONE', ( #2339, #26238, #2727, #28172 ) ) ;
#14581 = CARTESIAN_POINT ( 'NONE',  ( -7.468012846824771955, 51.53684000092397355, -28.02196122052045624 ) ) ;
#14582 = AXIS2_PLACEMENT_3D ( 'NONE', #5200, #24074, #21168 ) ;
#14583 = CARTESIAN_POINT ( 'NONE',  ( 10.04305231718578817, 9.900000005462358033, -30.90933677959249337 ) ) ;
#14584 =( BOUNDED_CURVE ( )  B_SPLINE_CURVE ( 2, ( #3389, #10947, #24324, #30120, #32695, #6623, #25326, #11769, #1804, #3882, #19674, #9029, #12280 ),
 .UNSPECIFIED., .F., .T. ) 
 B_SPLINE_CURVE_WITH_KNOTS ( ( 3, 2, 2, 2, 2, 2, 3 ),
 ( 0.7884615384615384359, 0.7897435897435897134, 0.7923076923076922684, 0.7948717948717948234, 0.7974358974358974894, 0.8000000000000000444, 0.8012820512820513219 ),
 .UNSPECIFIED. ) 
 CURVE ( )  GEOMETRIC_REPRESENTATION_ITEM ( )  RATIONAL_B_SPLINE_CURVE ( ( 0.9755282581475768211, 0.9755282581475768211, 1.000000000000000000, 0.9510565162951535312, 1.000000000000000000, 0.9510565162951535312, 1.000000000000000000, 0.9510565162951535312, 1.000000000000000000, 0.9510565162951535312, 1.000000000000000000, 0.9755282581475768211, 0.9755282581475768211 ) ) 
 REPRESENTATION_ITEM ( '' )  );
#14585 = CARTESIAN_POINT ( 'NONE',  ( -7.505752307972844761, 58.97916666666666430, 28.01184896238304134 ) ) ;
#14586 = CARTESIAN_POINT ( 'NONE',  ( 32.50000000000000000, 57.10000000000000142, -10.55989012756945833 ) ) ;
#14587 = CARTESIAN_POINT ( 'NONE',  ( 27.16883889988624290, 44.17500000273119554, 19.73931689729373673 ) ) ;
#14588 = CARTESIAN_POINT ( 'NONE',  ( -10.04305231718578462, 46.90000000546238113, 30.90933677959249337 ) ) ;
#14589 =( BOUNDED_CURVE ( )  B_SPLINE_CURVE ( 2, ( #20960, #18221, #2755, #23529, #13220, #23186, #18556, #10145, #7564, #18048, #28492, #4989, #10482 ),
 .UNSPECIFIED., .F., .T. ) 
 B_SPLINE_CURVE_WITH_KNOTS ( ( 3, 2, 2, 2, 2, 2, 3 ),
 ( 0.7756410256410256610, 0.7769230769230769384, 0.7794871794871794934, 0.7820512820512820484, 0.7846153846153846034, 0.7871794871794871584, 0.7884615384615384359 ),
 .UNSPECIFIED. ) 
 CURVE ( )  GEOMETRIC_REPRESENTATION_ITEM ( )  RATIONAL_B_SPLINE_CURVE ( ( 0.9755282581475768211, 0.9755282581475768211, 1.000000000000000000, 0.9510565162951535312, 1.000000000000000000, 0.9510565162951535312, 1.000000000000000000, 0.9510565162951535312, 1.000000000000000000, 0.9510565162951535312, 1.000000000000000000, 0.9755282581475768211, 0.9755282581475768211 ) ) 
 REPRESENTATION_ITEM ( '' )  );
#14590 = CARTESIAN_POINT ( 'NONE',  ( 4.635254915624212657, 80.60000000000000853, 14.26584774442730286 ) ) ;
#14591 = CARTESIAN_POINT ( 'NONE',  ( 6.486482029760649416E-15, 31.62500000273119483, 35.31076352940723240 ) ) ;
#14592 = CARTESIAN_POINT ( 'NONE',  ( 32.50000000000000711, 31.40000000546238468, 10.55989012756945122 ) ) ;
#14593 = CARTESIAN_POINT ( 'NONE',  ( 20.75514604977248467, 58.67500000273118843, -28.56700777964554305 ) ) ;
#14594 = PRESENTATION_STYLE_ASSIGNMENT (( #1020 ) ) ;
#14595 = EDGE_CURVE ( 'NONE', #927, #30177, #19213, .T. ) ;
#14596 = CARTESIAN_POINT ( 'NONE',  ( 32.50000000000000000, 33.10000000000000853, -10.55989012756945833 ) ) ;
#14597 = CARTESIAN_POINT ( 'NONE',  ( -20.08610463437157989, 35.70000000000000995, -27.64615127144129758 ) ) ;
#14598 = CARTESIAN_POINT ( 'NONE',  ( 24.50000000000000000, 2.000000000000001776, 0.000000000000000000 ) ) ;
#14599 = CARTESIAN_POINT ( 'NONE',  ( -10.37757302488623701, 75.52500000273118985, 31.93888565452638417 ) ) ;
#14600 = CARTESIAN_POINT ( 'NONE',  ( -15.01861347032170180, 66.99999999999998579, 29.12398716250626407 ) ) ;
#14601 = CARTESIAN_POINT ( 'NONE',  ( -8.601468415847518756, 77.07500000273118701, -11.83890561707634603 ) ) ;
#14602 = CARTESIAN_POINT ( 'NONE',  ( 10.37757302488624056, 68.77500000273117564, -31.93888565452638417 ) ) ;
#14603 = CARTESIAN_POINT ( 'NONE',  ( 12.13525491562421088, 79.05000000546236549, 8.816778784387095058 ) ) ;
#14604 = ADVANCED_FACE ( 'NONE', ( #15522 ), #2467, .T. ) ;
#14605 = ORIENTED_EDGE ( 'NONE', *, *, #24113, .T. ) ;
#14606 = CARTESIAN_POINT ( 'NONE',  ( -24.50000000000000000, 4.749999994537623671, -3.000384657911015469E-15 ) ) ;
#14607 = CARTESIAN_POINT ( 'NONE',  ( -6.950374756619716266, 17.16184000092397000, -26.09010956794232428 ) ) ;
#14608 = CARTESIAN_POINT ( 'NONE',  ( -26.29305231718579350, 25.79999999999999005, -19.10302069950537884 ) ) ;
#14609 = CARTESIAN_POINT ( 'NONE',  ( -10.37757302488624411, 38.72500000273119980, -31.93888565452638417 ) ) ;
#14610 = CARTESIAN_POINT ( 'NONE',  ( 33.58253175000000113, 6.475000002731178483, -10.91162601494193751 ) ) ;
#14611 = CARTESIAN_POINT ( 'NONE',  ( -33.58253175000000113, 57.47500000273118559, 10.91162601494193929 ) ) ;
#14612 = CARTESIAN_POINT ( 'NONE',  ( 6.988114217768294445, 55.25520833333333570, 26.07999730980477437 ) ) ;
#14613 = CARTESIAN_POINT ( 'NONE',  ( 14.97647472619947351, 42.79986083425731636, 26.02091320914850314 ) ) ;
#14614 = CARTESIAN_POINT ( 'NONE',  ( 25.98046417659831775, 39.06472249907601935, -15.04653450569338879 ) ) ;
#14615 = CARTESIAN_POINT ( 'NONE',  ( -20.08610463437157989, 70.20000000546237118, -27.64615127144129758 ) ) ;
#14616 = CARTESIAN_POINT ( 'NONE',  ( -11.25946833292375793, 81.17500000273119554, -8.180482586598733619 ) ) ;
#14617 = CARTESIAN_POINT ( 'NONE',  ( 0.04044903255044120238, 53.96055583240936926, 27.95245687107223276 ) ) ;
#14618 = CARTESIAN_POINT ( 'NONE',  ( -32.50000000000000000, 0.5000000054623809920, 0.000000000000000000 ) ) ;
#14619 = CARTESIAN_POINT ( 'NONE',  ( -15.01150461594642138, 12.14322916666666430, -26.00068869287340334 ) ) ;
#14620 = CARTESIAN_POINT ( 'NONE',  ( -27.16883889988623935, 39.57500000273118701, 19.73931689729374739 ) ) ;
#14621 = CARTESIAN_POINT ( 'NONE',  ( -7.236395654485763274, 2.524999997268823293, 22.27133577429736633 ) ) ;
#14622 = ORIENTED_EDGE ( 'NONE', *, *, #11354, .T. ) ;
#14623 = CARTESIAN_POINT ( 'NONE',  ( -32.50000000000000000, 30.60000000546238041, 10.55989012756946366 ) ) ;
#14624 = ORIENTED_EDGE ( 'NONE', *, *, #9791, .F. ) ;
#14625 = CARTESIAN_POINT ( 'NONE',  ( 28.01184896238304134, 34.05729166666666430, 7.505752307972846538 ) ) ;
#14626 = CARTESIAN_POINT ( 'NONE',  ( 10.04305231718579705, 65.10000000546240528, 30.90933677959248982 ) ) ;
#14627 = ORIENTED_EDGE ( 'NONE', *, *, #5280, .F. ) ;
#14628 = CARTESIAN_POINT ( 'NONE',  ( 20.08610463437157279, 27.29999999999997939, -27.64615127144129758 ) ) ;
#14629 = CARTESIAN_POINT ( 'NONE',  ( -27.16883889988623935, 51.32500000273118701, 19.73931689729374739 ) ) ;
#14630 = CARTESIAN_POINT ( 'NONE',  ( 32.50000000000000711, 55.40000000546238113, 10.55989012756945122 ) ) ;
#14631 = CARTESIAN_POINT ( 'NONE',  ( 28.01184896238290278, 64.70833333333334281, -7.505752307973347470 ) ) ;
#14632 = CARTESIAN_POINT ( 'NONE',  ( 32.50000000000000711, 11.40000000546237580, 10.55989012756945122 ) ) ;
#14633 = AXIS2_PLACEMENT_3D ( 'NONE', #28579, #23448, #26185 ) ;
#14634 = CARTESIAN_POINT ( 'NONE',  ( -14.47279130897151767, 17.82499999726881157, -19.92008829642072598 ) ) ;
#14635 = CARTESIAN_POINT ( 'NONE',  ( 32.50000000000000711, 54.90000000000001279, 10.55989012756945122 ) ) ;
#14636 = CARTESIAN_POINT ( 'NONE',  ( 3.880418787951139592, 1.551254281546846192, 24.50000000000000000 ) ) ;
#14637 = CARTESIAN_POINT ( 'NONE',  ( 10.37757302488624056, 16.77500000273118985, -31.93888565452638417 ) ) ;
#14638 = LINE ( 'NONE', #1234, #33747 ) ;
#14639 = CARTESIAN_POINT ( 'NONE',  ( 0.04044903255044120238, 23.02305583240935860, 27.95245687107223276 ) ) ;
#14640 = CARTESIAN_POINT ( 'NONE',  ( -8.960552108402742093E-16, 72.37500000273116996, -14.63369212191046387 ) ) ;
#14641 = CARTESIAN_POINT ( 'NONE',  ( 3.880418787951153803, 7.551254281546842861, 24.49999999999999645 ) ) ;
#14642 = CARTESIAN_POINT ( 'NONE',  ( -26.29305231718578995, 22.19999999999999574, 19.10302069950538595 ) ) ;
#14643 = AXIS2_PLACEMENT_3D ( 'NONE', #11659, #1008, #32585 ) ;
#14644 = B_SPLINE_CURVE_WITH_KNOTS ( 'NONE', 3,
 ( #11816, #4601, #33427, #9924, #25369, #30674, #32898, #17485, #17147, #20400, #9397, #22292, #27600, #22797, #33252, #19880, #30333, #9748, #7343, #20234, #19714, #14566, #17828, #3924, #14398, #6830, #21258, #13015, #23486, #21090, #26226, #294, #33947, #5289, #13354, #10439 ),
 .UNSPECIFIED., .F., .F.,
 ( 4, 2, 2, 2, 2, 2, 2, 2, 2, 2, 2, 2, 2, 2, 2, 2, 2, 4 ),
 ( 0.000000000000000000, 0.001481992817026406284, 0.002963985634052812568, 0.005927971268105625136, 0.008891956902158437703, 0.01037394971918484572, 0.01185594253621125548, 0.01778391380431686847, 0.02074789943836967063, 0.02371188507242247626, 0.02667587070647528535, 0.02815786352350169164, 0.02963985634052809445, 0.03556782760863372306, 0.04149579887673936207, 0.04297779169376576835, 0.04445978451079217464, 0.04742377014484498721 ),
 .UNSPECIFIED. ) ;
#14645 = CARTESIAN_POINT ( 'NONE',  ( -32.50000000000000000, 4.000000000000003553, 0.000000000000000000 ) ) ;
#14646 = ORIENTED_EDGE ( 'NONE', *, *, #3287, .T. ) ;
#14647 = CARTESIAN_POINT ( 'NONE',  ( -23.41746824999999887, 4.124999997268813168, -2.867812753649727150E-15 ) ) ;
#14648 = CARTESIAN_POINT ( 'NONE',  ( 26.29305231718579350, 71.30000000546237970, 19.10302069950537529 ) ) ;
#14649 = CARTESIAN_POINT ( 'NONE',  ( 13.97622843553589966, 53.96614583333333570, -24.20753774853756113 ) ) ;
#14650 = CARTESIAN_POINT ( 'NONE',  ( -33.58253175000000113, 59.12500000273116996, 0.000000000000000000 ) ) ;
#14651 = CARTESIAN_POINT ( 'NONE',  ( 27.16883889988624290, 22.17500000273119198, 19.73931689729373673 ) ) ;
#14652 = CARTESIAN_POINT ( 'NONE',  ( 10.37757302488624767, 11.97500000273120335, 31.93888565452638417 ) ) ;
#14653 = CARTESIAN_POINT ( 'NONE',  ( 33.58253175000000823, 4.275000002731189852, 10.91162601494192685 ) ) ;
#14654 = CARTESIAN_POINT ( 'NONE',  ( -7.543491769121417612, 15.72954833425730925, 28.00173670424549499 ) ) ;
#14655 = CARTESIAN_POINT ( 'NONE',  ( 7.468012846824281681, 14.57253499907601935, -28.02196122052058058 ) ) ;
#14656 = CARTESIAN_POINT ( 'NONE',  ( -8.960552108402744065E-16, 72.87500000273115575, -14.63369212191046209 ) ) ;
#14657 = CARTESIAN_POINT ( 'NONE',  ( 10.04305231718578817, 45.40000000000001279, -30.90933677959249337 ) ) ;
#14658 = CARTESIAN_POINT ( 'NONE',  ( -27.16883889988623935, 51.32500000273118701, 19.73931689729374739 ) ) ;
#14659 = CARTESIAN_POINT ( 'NONE',  ( -18.94512977948576093, 5.824999997268820451, 13.76444248337722698 ) ) ;
#14660 = ORIENTED_EDGE ( 'NONE', *, *, #29841, .F. ) ;
#14661 = CARTESIAN_POINT ( 'NONE',  ( -10.37757302488624411, 58.97500000273119269, -31.93888565452638417 ) ) ;
#14662 = CARTESIAN_POINT ( 'NONE',  ( -20.08610463437156923, 2.299999999999985612, 27.64615127144130113 ) ) ;
#14663 = CARTESIAN_POINT ( 'NONE',  ( 7.236395654485755280, 10.22499999726880837, 22.27133577429736988 ) ) ;
#14664 = CARTESIAN_POINT ( 'NONE',  ( 19.11951029504763611, 34.92225666759063074, -19.06425588902591173 ) ) ;
#14665 = VERTEX_POINT ( 'NONE', #5210 ) ;
#14666 = CARTESIAN_POINT ( 'NONE',  ( 20.75514604977248467, 28.42500000273118133, -28.56700777964554305 ) ) ;
#14667 = CARTESIAN_POINT ( 'NONE',  ( -26.29305231718578995, 34.70000000546239249, 19.10302069950538595 ) ) ;
#14668 = ORIENTED_EDGE ( 'NONE', *, *, #31598, .T. ) ;
#14669 = CARTESIAN_POINT ( 'NONE',  ( 7.505752307972854531, 64.13541666666667140, -28.01184896238303423 ) ) ;
#14670 = CARTESIAN_POINT ( 'NONE',  ( -33.58253175000000113, 59.47500000273118559, 10.91162601494193929 ) ) ;
#14671 = CARTESIAN_POINT ( 'NONE',  ( -15.00000000000000000, 76.09999999999998010, 4.873795443493597723 ) ) ;
#14672 = CARTESIAN_POINT ( 'NONE',  ( -20.75514604977248823, 68.82500000273118701, -28.56700777964554305 ) ) ;
#14673 = CARTESIAN_POINT ( 'NONE',  ( 28.01184896238304134, 30.61979166666666075, 7.505752307972846538 ) ) ;
#14674 = CARTESIAN_POINT ( 'NONE',  ( -24.50000000000000355, 12.90000000000000036, -7.960532557706207157 ) ) ;
#14675 = CARTESIAN_POINT ( 'NONE',  ( -33.58253175000000113, 3.275000002731191628, -10.91162601494193218 ) ) ;
#14676 = CARTESIAN_POINT ( 'NONE',  ( 20.75514604977249178, 11.82500000273118346, 28.56700777964553950 ) ) ;
#14677 = CARTESIAN_POINT ( 'NONE',  ( 4.300734207923761154, 71.47500000273119269, 13.23629886949340495 ) ) ;
#14678 = CARTESIAN_POINT ( 'NONE',  ( 30.02300923189239867, 53.10118083240936215, -0.04044903255044467877 ) ) ;
#14679 = CARTESIAN_POINT ( 'NONE',  ( -15.00000000000000000, 76.00000000000001421, 0.000000000000000000 ) ) ;
#14680 = CARTESIAN_POINT ( 'NONE',  ( 15.01150461594596486, 57.40364583333332860, -26.00068869287367690 ) ) ;
#14681 = DIRECTION ( 'NONE',  ( 0.000000000000000000, 0.000000000000000000, -1.000000000000000000 ) ) ;
#14682 = CARTESIAN_POINT ( 'NONE',  ( 5.779280353836490358E-15, 22.49999999999999645, 32.49999999999999289 ) ) ;
#14683 = CARTESIAN_POINT ( 'NONE',  ( 15.14183272437241889, 7.449999994537639836, 20.84094480462498211 ) ) ;
#14684 = CARTESIAN_POINT ( 'NONE',  ( 15.00000000000000000, 77.25000000546239676, -1.836970198721029589E-15 ) ) ;
#14685 = CARTESIAN_POINT ( 'NONE',  ( 24.20753774853731244, 13.00260416666666430, -13.97622843553632599 ) ) ;
#14686 = EDGE_CURVE ( 'NONE', #4188, #16901, #27612, .T. ) ;
#14687 =( BOUNDED_CURVE ( )  B_SPLINE_CURVE ( 2, ( #9495, #19977, #25467, #30423, #22720, #6922, #1944, #7262, #25290, #28207, #1762, #4693, #20152 ),
 .UNSPECIFIED., .F., .T. ) 
 B_SPLINE_CURVE_WITH_KNOTS ( ( 3, 2, 2, 2, 2, 2, 3 ),
 ( 0.1346153846153846090, 0.1358974358974358865, 0.1384615384615384692, 0.1410256410256410242, 0.1435897435897435792, 0.1461538461538461620, 0.1474358974358974395 ),
 .UNSPECIFIED. ) 
 CURVE ( )  GEOMETRIC_REPRESENTATION_ITEM ( )  RATIONAL_B_SPLINE_CURVE ( ( 0.9755282581475768211, 0.9755282581475768211, 1.000000000000000000, 0.9510565162951535312, 1.000000000000000000, 0.9510565162951535312, 1.000000000000000000, 0.9510565162951535312, 1.000000000000000000, 0.9510565162951535312, 1.000000000000000000, 0.9755282581475768211, 0.9755282581475768211 ) ) 
 REPRESENTATION_ITEM ( '' )  );
#14688 = CARTESIAN_POINT ( 'NONE',  ( 20.75514604977248467, 40.42500000273117422, -28.56700777964554305 ) ) ;
#14689 = CARTESIAN_POINT ( 'NONE',  ( 4.300734207923757602, 72.27500000273117564, -13.23629886949340673 ) ) ;
#14690 = CARTESIAN_POINT ( 'NONE',  ( 27.16883889988623935, 40.57500000273118701, -19.73931689729374384 ) ) ;
#14691 = CARTESIAN_POINT ( 'NONE',  ( 33.58253175000000823, 26.27500000273119340, 10.91162601494192685 ) ) ;
#14692 = CARTESIAN_POINT ( 'NONE',  ( -19.82091636218621389, 16.94999999453761319, 14.40073868116558842 ) ) ;
#14693 = EDGE_CURVE ( 'NONE', #1732, #7660, #11202, .T. ) ;
#14694 = CARTESIAN_POINT ( 'NONE',  ( -6.668400408272875007E-16, 2.249999994537632553, -24.50000000000000355 ) ) ;
#14695 = CARTESIAN_POINT ( 'NONE',  ( 32.50000000000000000, 79.00000000000001421, -3.980102097228898626E-15 ) ) ;
#14696 = CARTESIAN_POINT ( 'NONE',  ( -2.092463501923844636E-15, 67.50000000000000000, -34.17252228774368916 ) ) ;
#14697 = CARTESIAN_POINT ( 'NONE',  ( -7.236395654485757944, 9.224999997268806595, -22.27133577429736988 ) ) ;
#14698 = CARTESIAN_POINT ( 'NONE',  ( 14.97647472619900455, 25.02826416574268720, -26.02091320914876960 ) ) ;
#14699 = CARTESIAN_POINT ( 'NONE',  ( -12.13525491562420910, 78.19999999999998863, 8.816778784387098611 ) ) ;
#14700 = CARTESIAN_POINT ( 'NONE',  ( -26.06988505166722803, 34.05170166574267654, 7.025853678916877953 ) ) ;
#14701 = CARTESIAN_POINT ( 'NONE',  ( 10.37757302488624056, 78.77500000273117564, -31.93888565452638417 ) ) ;
#14702 = CARTESIAN_POINT ( 'NONE',  ( 27.16883889988624290, 13.92500000273116889, 19.73931689729373673 ) ) ;
#14703 = CARTESIAN_POINT ( 'NONE',  ( -23.41746825000000243, 12.02499999726881974, -7.608796670333730638 ) ) ;
#14704 = CARTESIAN_POINT ( 'NONE',  ( -19.09188309203660694, 59.26562500000000000, 19.09188309203694800 ) ) ;
#14705 = ORIENTED_EDGE ( 'NONE', *, *, #549, .T. ) ;
#14706 = CARTESIAN_POINT ( 'NONE',  ( 20.75514604977249178, 51.82500000273120122, 28.56700777964553950 ) ) ;
#14707 = CARTESIAN_POINT ( 'NONE',  ( 33.58253175000000823, 20.27500000273117564, 10.91162601494192863 ) ) ;
#14708 = EDGE_LOOP ( 'NONE', ( #14141, #17323, #31797, #12686 ) ) ;
#14709 = CARTESIAN_POINT ( 'NONE',  ( -7.505752307972844761, 34.91666666666666430, 28.01184896238304134 ) ) ;
#14710 = CARTESIAN_POINT ( 'NONE',  ( -26.02091320914849959, 33.34673583425730214, 14.97647472619947528 ) ) ;
#14711 = CARTESIAN_POINT ( 'NONE',  ( -3.880418787951142701, 3.448745718453150477, 24.49999999999999645 ) ) ;
#14712 = CARTESIAN_POINT ( 'NONE',  ( 19.82091636218621389, 17.94999999453761319, -14.40073868116559197 ) ) ;
#14713 = CARTESIAN_POINT ( 'NONE',  ( -14.47279130897151589, 13.32499999726880624, -19.92008829642072598 ) ) ;
#14714 = CARTESIAN_POINT ( 'NONE',  ( -10.37757302488623701, 19.77500000273118985, 31.93888565452638417 ) ) ;
#14715 = CARTESIAN_POINT ( 'NONE',  ( 26.29305231718578995, 21.70000000546237828, -19.10302069950538240 ) ) ;
#14716 = CARTESIAN_POINT ( 'NONE',  ( -20.08610463437156923, 72.30000000000002558, 27.64615127144130113 ) ) ;
#14717 = CARTESIAN_POINT ( 'NONE',  ( -1.778240108872766143E-15, 6.000000005462371888, -32.49999999999999289 ) ) ;
#14718 = DIRECTION ( 'NONE',  ( -1.224646799147353454E-16, 1.000000000000000000, -0.000000000000000000 ) ) ;
#14719 = CARTESIAN_POINT ( 'NONE',  ( -30.02300923189239867, 54.25819416759065206, -0.04044903254991731589 ) ) ;
#14720 = CARTESIAN_POINT ( 'NONE',  ( -2.162160676586881955E-15, 34.87500000273117706, -35.31076352940723240 ) ) ;
#14721 = CARTESIAN_POINT ( 'NONE',  ( -10.37757302488624411, 52.72500000273121401, -31.93888565452638417 ) ) ;
#14722 = CARTESIAN_POINT ( 'NONE',  ( 7.505752307972854531, 26.32291666666666075, -28.01184896238303423 ) ) ;
#14723 = CARTESIAN_POINT ( 'NONE',  ( 0.000000000000000000, 0.000000000000000000, 0.000000000000000000 ) ) ;
#14724 = CARTESIAN_POINT ( 'NONE',  ( 18.94512977948576093, 11.32499999726882578, -13.76444248337722875 ) ) ;
#14725 = CARTESIAN_POINT ( 'NONE',  ( -20.08610463437156923, 16.29999999999997584, 27.64615127144130113 ) ) ;
#14726 = CARTESIAN_POINT ( 'NONE',  ( 32.50000000000000711, 9.400000005462381125, 10.55989012756945122 ) ) ;
#14727 = CARTESIAN_POINT ( 'NONE',  ( 24.18731323226221974, 42.50222249907603356, -14.01125832528328985 ) ) ;
#14728 = CARTESIAN_POINT ( 'NONE',  ( -10.37757302488623701, 59.52500000273119696, 31.93888565452638417 ) ) ;
#14729 = CARTESIAN_POINT ( 'NONE',  ( 33.58253175000000113, 46.47500000273119269, -10.91162601494193574 ) ) ;
#14730 = DIRECTION ( 'NONE',  ( 0.000000000000000000, -1.000000000000000000, 0.000000000000000000 ) ) ;
#14731 = CARTESIAN_POINT ( 'NONE',  ( -15.00000000000000000, 70.25000000546238255, 0.000000000000000000 ) ) ;
#14732 = CARTESIAN_POINT ( 'NONE',  ( 11.54700538379251817, 96.00000000000002842, 19.99999999999999645 ) ) ;
#14733 = CARTESIAN_POINT ( 'NONE',  ( 19.06425588902592239, 49.53163166759063785, 19.11951029504763611 ) ) ;
#14734 = CARTESIAN_POINT ( 'NONE',  ( 2.205017735002230837E-13, 56.00000000546238255, -32.50000000000000000 ) ) ;
#14735 = CARTESIAN_POINT ( 'NONE',  ( -32.15037667113026743, 52.00000000000000000, 5.379467130815013043 ) ) ;
#14736 = CARTESIAN_POINT ( 'NONE',  ( 10.37757302488624056, 20.52500000273117919, -31.93888565452638417 ) ) ;
#14737 = DIRECTION ( 'NONE',  ( -0.000000000000000000, -1.000000000000000000, -0.000000000000000000 ) ) ;
#14738 = CARTESIAN_POINT ( 'NONE',  ( 20.08610463437157279, 53.29999999999999716, -27.64615127144129758 ) ) ;
#14739 = CARTESIAN_POINT ( 'NONE',  ( -1.778240108872766143E-15, 42.00000000546236834, -32.49999999999999289 ) ) ;
#14740 = CARTESIAN_POINT ( 'NONE',  ( 30.02300923189239867, 66.85118083240935505, -0.04044903255044467877 ) ) ;
#14741 = CARTESIAN_POINT ( 'NONE',  ( -26.29305231718578995, 44.70000000546238539, 19.10302069950538595 ) ) ;
#14742 = CARTESIAN_POINT ( 'NONE',  ( 12.13525491562421088, 71.05000000546237970, 8.816778784387095058 ) ) ;
#14743 = CARTESIAN_POINT ( 'NONE',  ( -20.75514604977248112, 31.42500000273120619, 28.56700777964554661 ) ) ;
#14744 = CARTESIAN_POINT ( 'NONE',  ( 6.486482029760649416E-15, 63.87500000273119127, 35.31076352940723240 ) ) ;
#14745 = CARTESIAN_POINT ( 'NONE',  ( -26.07999730980477437, 38.92708333333333570, 6.988114217768305103 ) ) ;
#14746 = ORIENTED_EDGE ( 'NONE', *, *, #24795, .T. ) ;
#14747 = CARTESIAN_POINT ( 'NONE',  ( 20.75514604977248467, 66.42500000273120975, -28.56700777964554305 ) ) ;
#14748 = CARTESIAN_POINT ( 'NONE',  ( -26.00068869287368756, 35.91927083333332860, -15.01150461594595775 ) ) ;
#14749 = CARTESIAN_POINT ( 'NONE',  ( -5.147494310547423346, 16.94874572391552903, 32.50000000000000000 ) ) ;
#14750 = ORIENTED_EDGE ( 'NONE', *, *, #3983, .F. ) ;
#14751 = CARTESIAN_POINT ( 'NONE',  ( -15.04653450569291984, 60.56027750092398065, 25.98046417659859486 ) ) ;
#14752 = CARTESIAN_POINT ( 'NONE',  ( -24.18731323226248264, 64.85715250092397355, -14.01125832528284931 ) ) ;
#14753 = CARTESIAN_POINT ( 'NONE',  ( -33.58253175000000113, 13.12500000273118772, 0.000000000000000000 ) ) ;
#14754 = CARTESIAN_POINT ( 'NONE',  ( -15.01150461594642138, 63.70572916666667140, -26.00068869287340334 ) ) ;
#14755 = FACE_OUTER_BOUND ( 'NONE', #30607, .T. ) ;
#14756 = CARTESIAN_POINT ( 'NONE',  ( -2.162160676586881955E-15, 38.87500000273120548, -35.31076352940723240 ) ) ;
#14757 = CARTESIAN_POINT ( 'NONE',  ( -32.50000000000000000, 42.60000000546238397, 10.55989012756946366 ) ) ;
#14758 = CARTESIAN_POINT ( 'NONE',  ( -13.91746824999999887, 75.37500000273116996, 0.000000000000000000 ) ) ;
#14759 = CARTESIAN_POINT ( 'NONE',  ( -20.75514604977248112, 27.42500000273118488, 28.56700777964554661 ) ) ;
#14760 = DIRECTION ( 'NONE',  ( 0.000000000000000000, 1.000000000000000000, 0.000000000000000000 ) ) ;
#14761 = CARTESIAN_POINT ( 'NONE',  ( 20.75514604977248467, 54.67500000273119554, -28.56700777964554305 ) ) ;
#14762 = SURFACE_SIDE_STYLE ('',( #9426 ) ) ;
#14763 = CARTESIAN_POINT ( 'NONE',  ( -32.50000000000000000, 36.10000000000000142, 10.55989012756946366 ) ) ;
#14764 = CARTESIAN_POINT ( 'NONE',  ( 26.29305231718579350, 32.79999999999999716, 19.10302069950537529 ) ) ;
#14765 = CARTESIAN_POINT ( 'NONE',  ( -14.47279130897151589, 15.32499999726880269, -19.92008829642072598 ) ) ;
#14766 = CARTESIAN_POINT ( 'NONE',  ( -33.58253175000000113, 73.22500000273117848, 10.91162601494193929 ) ) ;
#14767 = CARTESIAN_POINT ( 'NONE',  ( -6.725304478055195823, 66.99999999999998579, 31.94333337441920762 ) ) ;
#14768 = CARTESIAN_POINT ( 'NONE',  ( -32.50000000000000000, 38.09999999999998010, 10.55989012756946366 ) ) ;
#14769 = CARTESIAN_POINT ( 'NONE',  ( -33.58253175000000113, 67.27500000273117564, -10.91162601494193041 ) ) ;
#14770 = CARTESIAN_POINT ( 'NONE',  ( 15.00000000000000000, 75.25000000546239676, -1.836970198721029589E-15 ) ) ;
#14771 = DIRECTION ( 'NONE',  ( -0.000000000000000000, -1.000000000000000000, -0.000000000000000000 ) ) ;
#14772 = CARTESIAN_POINT ( 'NONE',  ( 27.16883889988623935, 18.32500000273118346, -19.73931689729374384 ) ) ;
#14773 = CARTESIAN_POINT ( 'NONE',  ( -24.50000000000000000, 10.74999999453762811, -3.000384657911015469E-15 ) ) ;
#14774 = CARTESIAN_POINT ( 'NONE',  ( -27.95245687107223986, 19.88319416759064495, -0.04044903254993292840 ) ) ;
#14775 = CARTESIAN_POINT ( 'NONE',  ( 32.50000000000000000, 47.09999999999999432, -10.55989012756945833 ) ) ;
#14776 = CARTESIAN_POINT ( 'NONE',  ( -20.75514604977248823, 42.82500000273119412, -28.56700777964554305 ) ) ;
#14777 = CARTESIAN_POINT ( 'NONE',  ( 20.75514604977248467, 2.675000002731181770, -28.56700777964554305 ) ) ;
#14778 = CARTESIAN_POINT ( 'NONE',  ( -33.58253175000000113, 55.47500000273120691, 10.91162601494193929 ) ) ;
#14779 = CARTESIAN_POINT ( 'NONE',  ( -28.00173670424549499, 44.08892333425729504, -7.543491769121417612 ) ) ;
#14780 = CARTESIAN_POINT ( 'NONE',  ( 26.02091320914876960, 39.63763916574268364, 14.97647472619900455 ) ) ;
#14781 = CARTESIAN_POINT ( 'NONE',  ( -20.08610463437156923, 58.80000000546239391, 27.64615127144130113 ) ) ;
#14782 = CARTESIAN_POINT ( 'NONE',  ( 11.25946833292375793, 80.17500000273119554, 8.180482586598731842 ) ) ;
#14783 = CARTESIAN_POINT ( 'NONE',  ( -6.988114217768288228, 12.28645833333333037, -26.07999730980477437 ) ) ;
#14784 =( BOUNDED_CURVE ( )  B_SPLINE_CURVE ( 2, ( #3315, #13781, #32125, #16524, #22007, #27486, #16692, #19266, #30215, #30048, #3976, #19435, #6043 ),
 .UNSPECIFIED., .F., .T. ) 
 B_SPLINE_CURVE_WITH_KNOTS ( ( 3, 2, 2, 2, 2, 2, 3 ),
 ( 0.2628205128205128305, 0.2641025641025641080, 0.2666666666666666630, 0.2692307692307692180, 0.2717948717948717730, 0.2743589743589743835, 0.2756410256410256610 ),
 .UNSPECIFIED. ) 
 CURVE ( )  GEOMETRIC_REPRESENTATION_ITEM ( )  RATIONAL_B_SPLINE_CURVE ( ( 0.9755282581475768211, 0.9755282581475768211, 1.000000000000000000, 0.9510565162951535312, 1.000000000000000000, 0.9510565162951535312, 1.000000000000000000, 0.9510565162951535312, 1.000000000000000000, 0.9510565162951535312, 1.000000000000000000, 0.9755282581475768211, 0.9755282581475768211 ) ) 
 REPRESENTATION_ITEM ( '' )  );
#14785 = CARTESIAN_POINT ( 'NONE',  ( -20.08610463437157989, 53.69999999999998863, -27.64615127144129758 ) ) ;
#14786 = CARTESIAN_POINT ( 'NONE',  ( -26.29305231718579350, 76.30000000546239391, -19.10302069950537884 ) ) ;
#14787 = CARTESIAN_POINT ( 'NONE',  ( 7.505752307973351023, 14.00520833333333215, 28.01184896238290278 ) ) ;
#14788 = CARTESIAN_POINT ( 'NONE',  ( 33.58253175000000823, 38.27500000273118985, 10.91162601494192863 ) ) ;
#14789 = CARTESIAN_POINT ( 'NONE',  ( -18.94512977948576093, 4.324999997268818674, 13.76444248337722698 ) ) ;
#14790 = ORIENTED_EDGE ( 'NONE', *, *, #9027, .T. ) ;
#14791 = CARTESIAN_POINT ( 'NONE',  ( 33.58253175000000823, 72.27500000273118985, 10.91162601494192863 ) ) ;
#14792 = CARTESIAN_POINT ( 'NONE',  ( -10.04305231718578462, 30.90000000546237757, 30.90933677959249337 ) ) ;
#14793 = ORIENTED_EDGE ( 'NONE', *, *, #28085, .F. ) ;
#14794 = CARTESIAN_POINT ( 'NONE',  ( 20.50609665441005092, 37.78124999999999289, 20.50609665440969209 ) ) ;
#14795 = CARTESIAN_POINT ( 'NONE',  ( 10.04305231718578817, 65.90000000546237402, -30.90933677959249337 ) ) ;
#14796 = ORIENTED_EDGE ( 'NONE', *, *, #20914, .F. ) ;
#14797 = CARTESIAN_POINT ( 'NONE',  ( -19.82091636218621034, 12.54999999453762527, -14.40073868116559552 ) ) ;
#14798 = CARTESIAN_POINT ( 'NONE',  ( 20.75514604977248467, 46.42500000273119554, -28.56700777964554305 ) ) ;
#14799 = CARTESIAN_POINT ( 'NONE',  ( 1.507698388325705758E-15, 15.12499999726880873, -24.62258325217400312 ) ) ;
#14800 = CARTESIAN_POINT ( 'NONE',  ( -15.01150461594595775, 62.55989583333332860, 26.00068869287368756 ) ) ;
#14801 = CARTESIAN_POINT ( 'NONE',  ( -32.50000000000000000, 2.500000005462382546, 0.000000000000000000 ) ) ;
#14802 = CARTESIAN_POINT ( 'NONE',  ( 5.779280353836490358E-15, 8.500000000000000000, 32.49999999999999289 ) ) ;
#14803 = CARTESIAN_POINT ( 'NONE',  ( 26.00068869287341045, 13.00260416666666430, -15.01150461594642493 ) ) ;
#14804 = CARTESIAN_POINT ( 'NONE',  ( -32.50000000000000000, 55.99999999999999289, 0.000000000000000000 ) ) ;
#14805 = FACE_OUTER_BOUND ( 'NONE', #28924, .T. ) ;
#14806 = CARTESIAN_POINT ( 'NONE',  ( 27.16883889988624290, 18.17500000273120264, 19.73931689729373673 ) ) ;
#14807 = DIRECTION ( 'NONE',  ( 0.000000000000000000, 0.000000000000000000, 1.000000000000000000 ) ) ;
#14808 = CARTESIAN_POINT ( 'NONE',  ( -19.11951029504797006, 24.31211833240934794, -19.06425588902558133 ) ) ;
#14809 = PRODUCT_DEFINITION_FORMATION_WITH_SPECIFIED_SOURCE ( 'ANY', '', #4952, .NOT_KNOWN. ) ;
#14810 = CARTESIAN_POINT ( 'NONE',  ( 11.25946833292375793, 76.07500000273120122, -8.180482586598735395 ) ) ;
#14811 = CARTESIAN_POINT ( 'NONE',  ( 3.445340210940985210E-14, 7.499999999999994671, 24.50000000000000000 ) ) ;
#14812 = CARTESIAN_POINT ( 'NONE',  ( -27.16883889988624290, 79.17500000273118133, -19.73931689729374028 ) ) ;
#14813 = VERTEX_POINT ( 'NONE', #11691 ) ;
#14814 = CARTESIAN_POINT ( 'NONE',  ( -14.47279130897151589, 13.82499999726882045, -19.92008829642072598 ) ) ;
#14815 = CARTESIAN_POINT ( 'NONE',  ( 10.04305231718579705, 71.10000000546237686, 30.90933677959248982 ) ) ;
#14816 = CARTESIAN_POINT ( 'NONE',  ( 6.988114217768294445, 51.81770833333332860, 26.07999730980477437 ) ) ;
#14817 = ADVANCED_FACE ( 'NONE', ( #19598, #6381 ), #32619, .F. ) ;
#14818 = CARTESIAN_POINT ( 'NONE',  ( -27.16883889988624290, 58.92500000273119554, -19.73931689729374028 ) ) ;
#14819 = CARTESIAN_POINT ( 'NONE',  ( 10.37757302488624056, 24.77500000273118275, -31.93888565452638417 ) ) ;
#14820 = CARTESIAN_POINT ( 'NONE',  ( -33.58253175000000113, 9.275000002731177418, -10.91162601494193218 ) ) ;
#14821 = CARTESIAN_POINT ( 'NONE',  ( 20.75514604977249178, 4.075000002731195892, 28.56700777964553950 ) ) ;
#14822 = CARTESIAN_POINT ( 'NONE',  ( -28.00173670424549499, 16.58892333425730570, -7.543491769121417612 ) ) ;
#14823 = ADVANCED_FACE ( 'NONE', ( #29538 ), #24317, .T. ) ;
#14824 = CARTESIAN_POINT ( 'NONE',  ( -26.00068869287340334, 59.40885416666666430, 15.01150461594643382 ) ) ;
#14825 = CARTESIAN_POINT ( 'NONE',  ( -32.50000000000000000, 78.50000000546238255, 0.000000000000000000 ) ) ;
#14826 = CARTESIAN_POINT ( 'NONE',  ( 8.601468415847520532, 72.07500000273120122, 11.83890561707634603 ) ) ;
#14827 = CARTESIAN_POINT ( 'NONE',  ( -26.29305231718579350, 41.79999999999999005, -19.10302069950537884 ) ) ;
#14828 = CARTESIAN_POINT ( 'NONE',  ( -33.58253175000000113, 43.02500000273118275, -10.91162601494193041 ) ) ;
#14829 = CARTESIAN_POINT ( 'NONE',  ( -23.41746825000000243, 1.524999997268801755, -7.608796670333730638 ) ) ;
#14830 = EDGE_CURVE ( 'NONE', #27878, #19445, #12216, .T. ) ;
#14831 = FACE_OUTER_BOUND ( 'NONE', #2481, .T. ) ;
#14832 = ORIENTED_EDGE ( 'NONE', *, *, #8117, .F. ) ;
#14833 = CARTESIAN_POINT ( 'NONE',  ( -10.37757302488623701, 57.77500000273121117, 31.93888565452638417 ) ) ;
#14834 = CARTESIAN_POINT ( 'NONE',  ( -1.778240108872766143E-15, 41.49999999999999289, -32.49999999999999289 ) ) ;
#14835 = CARTESIAN_POINT ( 'NONE',  ( -14.47279130897152122, 11.92499999726882010, 19.92008829642072243 ) ) ;
#14836 = CARTESIAN_POINT ( 'NONE',  ( 24.18731323226247554, 32.20090250092397355, 14.01125832528285997 ) ) ;
#14837 = ORIENTED_EDGE ( 'NONE', *, *, #30899, .T. ) ;
#14838 = CARTESIAN_POINT ( 'NONE',  ( 20.75514604977248467, 30.42500000273117777, -28.56700777964554305 ) ) ;
#14839 = DIRECTION ( 'NONE',  ( -1.224646799147353454E-16, 1.000000000000000000, -0.000000000000000000 ) ) ;
#14840 = VERTEX_POINT ( 'NONE', #32250 ) ;
#14841 = CARTESIAN_POINT ( 'NONE',  ( 32.50000000000000000, 69.60000000546237686, -10.55989012756945833 ) ) ;
#14842 = CARTESIAN_POINT ( 'NONE',  ( -20.75514604977248823, 66.82500000273118701, -28.56700777964554305 ) ) ;
#14843 = CARTESIAN_POINT ( 'NONE',  ( -20.50609665440969209, 38.64062500000000000, 20.50609665441005092 ) ) ;
#14844 = CARTESIAN_POINT ( 'NONE',  ( 1.577395562988744260E-15, 12.50000000000001243, -25.76082449383753925 ) ) ;
#14845 = LINE ( 'NONE', #3866, #21019 ) ;
#14846 = CARTESIAN_POINT ( 'NONE',  ( -33.58253175000000113, 9.025000002731184523, -10.91162601494193218 ) ) ;
#14847 = FILL_AREA_STYLE ('',( #33890 ) ) ;
#14848 = CARTESIAN_POINT ( 'NONE',  ( -14.97647472619899389, 54.24701416574269075, 26.02091320914878025 ) ) ;
#14849 = CARTESIAN_POINT ( 'NONE',  ( 15.00000000000000000, 73.09999999999996589, -4.873795443493596835 ) ) ;
#14850 = CARTESIAN_POINT ( 'NONE',  ( 7.505752307972854531, 60.69791666666667140, -28.01184896238303423 ) ) ;
#14851 = CARTESIAN_POINT ( 'NONE',  ( -1.778240108872766143E-15, 55.49999999999999289, -32.49999999999999289 ) ) ;
#14852 = CARTESIAN_POINT ( 'NONE',  ( -20.08610463437156923, 52.30000000000000426, 27.64615127144130113 ) ) ;
#14853 = CARTESIAN_POINT ( 'NONE',  ( 19.82091636218621034, 3.549999994537617276, 14.40073868116559730 ) ) ;
#14854 = CARTESIAN_POINT ( 'NONE',  ( -9.657523855033125146E-16, 77.75000000546238255, -15.77193336357400710 ) ) ;
#14855 = CARTESIAN_POINT ( 'NONE',  ( 13.97622843553633665, 24.17447916666666785, 24.20753774853730889 ) ) ;
#14856 = CARTESIAN_POINT ( 'NONE',  ( -10.37757302488623701, 35.52500000273117564, 31.93888565452638417 ) ) ;
#14857 = CARTESIAN_POINT ( 'NONE',  ( -8.891200544363830713E-16, 75.50000000000001421, -15.00000000000000000 ) ) ;
#14858 = CARTESIAN_POINT ( 'NONE',  ( 10.37757302488624056, 44.77500000273119696, -31.93888565452638417 ) ) ;
#14859 = CARTESIAN_POINT ( 'NONE',  ( 10.37757302488624767, 23.97500000273117138, 31.93888565452638417 ) ) ;
#14860 = DIRECTION ( 'NONE',  ( 0.000000000000000000, -1.000000000000000000, 0.000000000000000000 ) ) ;
#14861 = CARTESIAN_POINT ( 'NONE',  ( -7.570916362186215665, 15.14999999453761603, 23.30088464923126423 ) ) ;
#14862 = CARTESIAN_POINT ( 'NONE',  ( 15.00000000000000000, 81.00000000000001421, -1.836970198721029589E-15 ) ) ;
#14863 = CARTESIAN_POINT ( 'NONE',  ( -32.50000000000000000, 63.89999999999998437, -10.55989012756945478 ) ) ;
#14864 = CARTESIAN_POINT ( 'NONE',  ( 7.236395654485755280, 10.22499999726880837, 22.27133577429736988 ) ) ;
#14865 = CARTESIAN_POINT ( 'NONE',  ( 7.543491769121922985, 26.31732666574268364, 28.00173670424535644 ) ) ;
#14866 = CARTESIAN_POINT ( 'NONE',  ( -4.635254915624211769, 77.60000000000000853, -14.26584774442730286 ) ) ;
#14867 = CARTESIAN_POINT ( 'NONE',  ( 19.06425588902558133, 38.92149333240934794, -19.11951029504797006 ) ) ;
#14868 = AXIS2_PLACEMENT_3D ( 'NONE', #23037, #20652, #15320 ) ;
#14869 = CARTESIAN_POINT ( 'NONE',  ( -10.37757302488624411, 76.97500000273120691, -31.93888565452638417 ) ) ;
#14870 = CARTESIAN_POINT ( 'NONE',  ( 6.486482029760648627E-15, 15.62500000273118062, 35.31076352940722529 ) ) ;
#14871 = CARTESIAN_POINT ( 'NONE',  ( 23.41746825000000243, 11.22499999726881548, -7.608796670333727974 ) ) ;
#14872 = CARTESIAN_POINT ( 'NONE',  ( 19.09188309203694800, 65.28125000000000000, 19.09188309203660694 ) ) ;
#14873 = ORIENTED_EDGE ( 'NONE', *, *, #11926, .T. ) ;
#14874 = CARTESIAN_POINT ( 'NONE',  ( 27.16883889988623935, 52.32500000273120122, -19.73931689729374384 ) ) ;
#14875 = CARTESIAN_POINT ( 'NONE',  ( 10.37757302488624056, 22.77500000273117919, -31.93888565452638417 ) ) ;
#14876 = ADVANCED_FACE ( 'NONE', ( #13578 ), #24371, .T. ) ;
#14877 = ORIENTED_EDGE ( 'NONE', *, *, #3297, .F. ) ;
#14878 = CARTESIAN_POINT ( 'NONE',  ( -15.01150461594642138, 29.33072916666665719, -26.00068869287340334 ) ) ;
#14879 = CARTESIAN_POINT ( 'NONE',  ( -25.98046417659859486, 30.48215250092397710, -15.04653450569291628 ) ) ;
#14880 = CIRCLE ( 'NONE', #29656, 10.17814985357208890 ) ;
#14881 = TOROIDAL_SURFACE ( 'NONE', #27467, 11.45223628611452860, 4.000000000000014211 ) ;
#14882 = FACE_OUTER_BOUND ( 'NONE', #13607, .T. ) ;
#14883 = CARTESIAN_POINT ( 'NONE',  ( -14.47279130897152122, 4.424999997268826313, 19.92008829642072243 ) ) ;
#14884 = CARTESIAN_POINT ( 'NONE',  ( 23.41746825000000243, 12.72499999726882436, -7.608796670333727974 ) ) ;
#14885 = CARTESIAN_POINT ( 'NONE',  ( 27.16883889988623935, 22.57500000273118701, -19.73931689729374384 ) ) ;
#14886 = CARTESIAN_POINT ( 'NONE',  ( 32.50000000000000000, 27.50000000546237544, -3.980102097228898626E-15 ) ) ;
#14887 =( BOUNDED_CURVE ( )  B_SPLINE_CURVE ( 2, ( #7130, #11942, #4048, #14523, #30462, #22253, #14862, #22928, #17610, #9030, #11772, #19510, #24814 ),
 .UNSPECIFIED., .F., .T. ) 
 B_SPLINE_CURVE_WITH_KNOTS ( ( 3, 2, 2, 2, 2, 2, 3 ),
 ( 0.05000000000000000278, 0.05999999999999999778, 0.08000000000000000167, 0.1000000000000000056, 0.1199999999999999956, 0.1400000000000000133, 0.1500000000000000222 ),
 .UNSPECIFIED. ) 
 CURVE ( )  GEOMETRIC_REPRESENTATION_ITEM ( )  RATIONAL_B_SPLINE_CURVE ( ( 0.9755282581475768211, 0.9755282581475768211, 1.000000000000000000, 0.9510565162951535312, 1.000000000000000000, 0.9510565162951535312, 1.000000000000000000, 0.9510565162951535312, 1.000000000000000000, 0.9510565162951535312, 1.000000000000000000, 0.9755282581475767101, 0.9755282581475768211 ) ) 
 REPRESENTATION_ITEM ( '' )  );
#14888 = CARTESIAN_POINT ( 'NONE',  ( -10.04305231718578462, 66.40000000000001990, 30.90933677959249337 ) ) ;
#14889 = DIRECTION ( 'NONE',  ( -0.8660254037844410391, -0.4999999999999958367, -0.000000000000000000 ) ) ;
#14890 = CARTESIAN_POINT ( 'NONE',  ( 5.779280353836490358E-15, 66.49999999999998579, 32.49999999999999289 ) ) ;
#14891 = CARTESIAN_POINT ( 'NONE',  ( 20.50609665440969565, 16.29687499999999645, -20.50609665441004736 ) ) ;
#14892 = CARTESIAN_POINT ( 'NONE',  ( -20.75514604977248112, 37.67500000273118133, 28.56700777964554661 ) ) ;
#14893 = DIRECTION ( 'NONE',  ( 0.000000000000000000, 0.000000000000000000, -1.000000000000000000 ) ) ;
#14894 = CARTESIAN_POINT ( 'NONE',  ( 15.01150461594643382, 31.04947916666666430, 26.00068869287340334 ) ) ;
#14895 = CARTESIAN_POINT ( 'NONE',  ( -2.092463501923844636E-15, 11.49999999999998579, -34.17252228774368916 ) ) ;
#14896 = CARTESIAN_POINT ( 'NONE',  ( 19.82091636218621034, 17.80000000000001137, 14.40073868116559730 ) ) ;
#14897 = CARTESIAN_POINT ( 'NONE',  ( -24.18731323226221974, 51.09597249907602645, 14.01125832528330406 ) ) ;
#14898 = CARTESIAN_POINT ( 'NONE',  ( -33.58253175000000113, 57.12500000273118417, 0.000000000000000000 ) ) ;
#14899 = CARTESIAN_POINT ( 'NONE',  ( 10.37757302488624056, 60.77500000273118275, -31.93888565452638417 ) ) ;
#14900 = CARTESIAN_POINT ( 'NONE',  ( -27.16883889988624290, 43.17500000273119554, -19.73931689729374028 ) ) ;
#14901 = CARTESIAN_POINT ( 'NONE',  ( 20.08610463437158344, 44.69999999999998153, 27.64615127144129403 ) ) ;
#14902 = CARTESIAN_POINT ( 'NONE',  ( 15.14183272437242422, 10.29999999999999361, -20.84094480462497856 ) ) ;
#14903 = DIRECTION ( 'NONE',  ( -0.8660254037844387076, 0.000000000000000000, -0.4999999999999998335 ) ) ;
#14904 = CARTESIAN_POINT ( 'NONE',  ( -0.04044903254992426173, 49.96131916759065206, 27.95245687107223276 ) ) ;
#14905 = CARTESIAN_POINT ( 'NONE',  ( 10.04305231718579705, 63.10000000546238397, 30.90933677959248982 ) ) ;
#14906 = CARTESIAN_POINT ( 'NONE',  ( 19.82091636218621034, 3.799999999999998046, 14.40073868116559730 ) ) ;
#14907 = CARTESIAN_POINT ( 'NONE',  ( 10.37757302488624056, 22.52500000273117919, -31.93888565452638417 ) ) ;
#14908 = CARTESIAN_POINT ( 'NONE',  ( 2.489536152421872915E-14, 76.00000000546238255, -32.49999999999999289 ) ) ;
#14909 = DIRECTION ( 'NONE',  ( 1.000000000000000000, 0.000000000000000000, 0.000000000000000000 ) ) ;
#14910 = DIRECTION ( 'NONE',  ( 0.000000000000000000, 0.000000000000000000, -1.000000000000000000 ) ) ;
#14911 = CARTESIAN_POINT ( 'NONE',  ( 0.04044903255045854962, 64.27305583240934084, 30.02300923189239867 ) ) ;
#14912 = CARTESIAN_POINT ( 'NONE',  ( -32.50000000000000000, 40.40000000546239534, -10.55989012756945478 ) ) ;
#14913 = DIRECTION ( 'NONE',  ( -0.000000000000000000, -1.000000000000000000, -0.000000000000000000 ) ) ;
#14914 = CARTESIAN_POINT ( 'NONE',  ( -10.37757302488624411, 32.72500000273117848, -31.93888565452638417 ) ) ;
#14915 = CARTESIAN_POINT ( 'NONE',  ( -6.988114217768288228, 39.78645833333332860, -26.07999730980477437 ) ) ;
#14916 = VERTEX_POINT ( 'NONE', #21634 ) ;
#14917 = CARTESIAN_POINT ( 'NONE',  ( 20.75514604977248467, 68.42500000273120975, -28.56700777964554305 ) ) ;
#14918 = CARTESIAN_POINT ( 'NONE',  ( 26.00068869287367335, 37.63802083333331439, 15.01150461594596308 ) ) ;
#14919 = EDGE_CURVE ( 'NONE', #14306, #33710, #24205, .T. ) ;
#14920 = CARTESIAN_POINT ( 'NONE',  ( -20.08610463437156923, 16.80000000546237970, 27.64615127144130113 ) ) ;
#14921 = EDGE_LOOP ( 'NONE', ( #8132, #20416, #27616, #1645 ) ) ;
#14922 = CARTESIAN_POINT ( 'NONE',  ( -7.468012846824771955, 58.41184000092398065, -28.02196122052045624 ) ) ;
#14923 = CARTESIAN_POINT ( 'NONE',  ( -19.11951029504763611, 64.14100666759063074, 19.06425588902592239 ) ) ;
#14924 = CARTESIAN_POINT ( 'NONE',  ( -20.75514604977248112, 13.42500000273119198, 28.56700777964554661 ) ) ;
#14925 = EDGE_CURVE ( 'NONE', #17393, #30686, #15807, .T. ) ;
#14926 = CARTESIAN_POINT ( 'NONE',  ( -26.00068869287368756, 66.85677083333334281, -15.01150461594595775 ) ) ;
#14927 = CARTESIAN_POINT ( 'NONE',  ( -32.50000000000000000, 45.90000000000000568, -10.55989012756945300 ) ) ;
#14928 = CARTESIAN_POINT ( 'NONE',  ( 6.486482029760649416E-15, 43.87500000273118417, 35.31076352940723240 ) ) ;
#14929 = CARTESIAN_POINT ( 'NONE',  ( 32.50000000000000000, 41.50000000546238965, -3.980102097228898626E-15 ) ) ;
#14930 = CARTESIAN_POINT ( 'NONE',  ( -9.270509831248425314, 73.70000000000000284, -12.75976212528059861 ) ) ;
#14931 = CARTESIAN_POINT ( 'NONE',  ( -10.37757302488623701, 27.52500000273119696, 31.93888565452638417 ) ) ;
#14932 = CARTESIAN_POINT ( 'NONE',  ( -1.778240108872766143E-15, 23.49999999999999645, -32.49999999999999289 ) ) ;
#14933 = CARTESIAN_POINT ( 'NONE',  ( 33.58253175000000113, 56.37500000273118417, -4.112674001490185761E-15 ) ) ;
#14934 = SURFACE_STYLE_USAGE ( .BOTH. , #7376 ) ;
#14935 = CARTESIAN_POINT ( 'NONE',  ( -10.04305231718579172, 31.60000000000000142, -30.90933677959248982 ) ) ;
#14936 = CARTESIAN_POINT ( 'NONE',  ( 32.50000000000000000, 33.10000000000000853, -10.55989012756945833 ) ) ;
#14937 = CARTESIAN_POINT ( 'NONE',  ( -18.94512977948576093, 15.82499999726880091, 13.76444248337722698 ) ) ;
#14938 = CARTESIAN_POINT ( 'NONE',  ( -10.37757302488624411, 78.72500000273119269, -31.93888565452638417 ) ) ;
#14939 = FACE_OUTER_BOUND ( 'NONE', #1096, .T. ) ;
#14940 = CARTESIAN_POINT ( 'NONE',  ( -19.82091636218621034, 14.80000000000000782, -14.40073868116559552 ) ) ;
#14941 = CARTESIAN_POINT ( 'NONE',  ( -27.16883889988624290, 69.17500000273119554, -19.73931689729374028 ) ) ;
#14942 = CARTESIAN_POINT ( 'NONE',  ( 15.00000000000000000, 79.35000000546241949, -4.873795443493596835 ) ) ;
#14943 = VERTEX_POINT ( 'NONE', #26934 ) ;
#14944 = CARTESIAN_POINT ( 'NONE',  ( -33.58253175000000113, 21.02500000273117919, -10.91162601494193218 ) ) ;
#14945 = CARTESIAN_POINT ( 'NONE',  ( 24.50000000000000355, 9.849999994537622428, -7.960532557706203605 ) ) ;
#14946 = CARTESIAN_POINT ( 'NONE',  ( 19.06425588902592239, 22.03163166759064495, 19.11951029504763611 ) ) ;
#14947 = CARTESIAN_POINT ( 'NONE',  ( -2.165007332552593587E-13, 46.50000000000000711, 32.50000000000000000 ) ) ;
#14948 = CIRCLE ( 'NONE', #10032, 26.50000000000000355 ) ;
#14949 = CARTESIAN_POINT ( 'NONE',  ( 33.58253175000000113, 38.22500000273119269, -10.91162601494193751 ) ) ;
#14950 = CARTESIAN_POINT ( 'NONE',  ( -10.37757302488623701, 3.775000002731190740, 31.93888565452638417 ) ) ;
#14951 = CARTESIAN_POINT ( 'NONE',  ( 27.16883889988623935, 58.57500000273117990, -19.73931689729374384 ) ) ;
#14952 = CARTESIAN_POINT ( 'NONE',  ( -14.97647472619946285, 47.95611083425732346, -26.02091320914851025 ) ) ;
#14953 = AXIS2_PLACEMENT_3D ( 'NONE', #14291, #19446, #9643 ) ;
#14954 = CARTESIAN_POINT ( 'NONE',  ( -8.960552108402744065E-16, 80.37500000273119838, -14.63369212191046209 ) ) ;
#14955 = CARTESIAN_POINT ( 'NONE',  ( -25.98046417659831420, 37.34597249907603356, 15.04653450569339945 ) ) ;
#14956 = CARTESIAN_POINT ( 'NONE',  ( 32.50000000000000711, 59.40000000546237402, 10.55989012756945122 ) ) ;
#14957 = CARTESIAN_POINT ( 'NONE',  ( -4.300734207923759378, 74.47500000273116427, -13.23629886949340495 ) ) ;
#14958 = CARTESIAN_POINT ( 'NONE',  ( -13.94119854578892514, 61.12201416574268364, 24.22776226481266448 ) ) ;
#14959 = CARTESIAN_POINT ( 'NONE',  ( 30.91025403784432868, -20.70096189432334199, 0.000000000000000000 ) ) ;
#14960 = CARTESIAN_POINT ( 'NONE',  ( -20.08610463437156923, 74.80000000546239391, 27.64615127144130113 ) ) ;
#14961 = CARTESIAN_POINT ( 'NONE',  ( 12.13525491562421088, 78.80000000000003979, 8.816778784387095058 ) ) ;
#14962 = CARTESIAN_POINT ( 'NONE',  ( -33.58253175000000113, 35.37500000273117706, 0.000000000000000000 ) ) ;
#14963 = CARTESIAN_POINT ( 'NONE',  ( 18.94512977948575738, 6.924999997268810326, 13.76444248337723408 ) ) ;
#14964 = ORIENTED_EDGE ( 'NONE', *, *, #10945, .T. ) ;
#14965 = CARTESIAN_POINT ( 'NONE',  ( -10.37757302488623701, 73.77500000273118985, 31.93888565452638417 ) ) ;
#14966 = CARTESIAN_POINT ( 'NONE',  ( 10.04305231718579705, 23.10000000546237686, 30.90933677959248982 ) ) ;
#14967 = CARTESIAN_POINT ( 'NONE',  ( -7.505752307973343918, 46.66145833333332860, -28.01184896238290989 ) ) ;
#14968 = CARTESIAN_POINT ( 'NONE',  ( -26.29305231718578995, 62.70000000546238539, 19.10302069950538595 ) ) ;
#14969 = ORIENTED_EDGE ( 'NONE', *, *, #32764, .F. ) ;
#14970 = CARTESIAN_POINT ( 'NONE',  ( -10.04305231718579172, 55.59999999999998010, -30.90933677959248982 ) ) ;
#14971 = CARTESIAN_POINT ( 'NONE',  ( 27.16883889988624290, 45.92500000273119554, 19.73931689729373673 ) ) ;
#14972 = CARTESIAN_POINT ( 'NONE',  ( -23.41746825000000598, 15.72499999726882081, 7.608796670333726198 ) ) ;
#14973 = CARTESIAN_POINT ( 'NONE',  ( 32.50000000000000000, 7.500000005462359454, -3.980102097228898626E-15 ) ) ;
#14974 = CARTESIAN_POINT ( 'NONE',  ( -10.04305231718579172, 7.599999999999996092, -30.90933677959248982 ) ) ;
#14975 = CARTESIAN_POINT ( 'NONE',  ( -20.50609665440969209, 14.57812499999999645, 20.50609665441005092 ) ) ;
#14976 = CARTESIAN_POINT ( 'NONE',  ( -10.04305231718578462, 50.39999999999999858, 30.90933677959249337 ) ) ;
#14977 = CARTESIAN_POINT ( 'NONE',  ( -33.58253175000000113, 19.27500000273117919, -10.91162601494193218 ) ) ;
#14978 = DIRECTION ( 'NONE',  ( -0.000000000000000000, -1.000000000000000000, -0.000000000000000000 ) ) ;
#14979 = CARTESIAN_POINT ( 'NONE',  ( 19.06425588902558133, 25.17149333240934439, -19.11951029504797006 ) ) ;
#14980 = CARTESIAN_POINT ( 'NONE',  ( 4.300734207923757602, 80.77500000273118985, -13.23629886949340673 ) ) ;
#14981 = LINE ( 'NONE', #4507, #10212 ) ;
#14982 = CARTESIAN_POINT ( 'NONE',  ( -26.29305231718579350, 43.80000000000000426, -19.10302069950537884 ) ) ;
#14983 = CARTESIAN_POINT ( 'NONE',  ( -26.29305231718579350, 3.799999999999998046, -19.10302069950537884 ) ) ;
#14984 = ORIENTED_EDGE ( 'NONE', *, *, #29583, .F. ) ;
#14985 = CARTESIAN_POINT ( 'NONE',  ( 14.47279130897151767, 11.42499999726880944, -19.92008829642072598 ) ) ;
#14986 = CARTESIAN_POINT ( 'NONE',  ( 23.41746824999999887, 0.7249999972688272454, -7.608796670333727974 ) ) ;
#14987 = CARTESIAN_POINT ( 'NONE',  ( 19.09188309203694800, 54.96875000000000000, 19.09188309203660694 ) ) ;
#14988 = ADVANCED_FACE ( 'NONE', ( #3432 ), #842, .T. ) ;
#14989 = CARTESIAN_POINT ( 'NONE',  ( -33.58253175000000113, 63.22500000273119269, 10.91162601494193929 ) ) ;
#14990 = CARTESIAN_POINT ( 'NONE',  ( -10.37757302488623701, 23.77500000273117919, 31.93888565452638417 ) ) ;
#14991 = CARTESIAN_POINT ( 'NONE',  ( 20.75514604977249178, 12.07500000273119234, 28.56700777964553950 ) ) ;
#14992 = CARTESIAN_POINT ( 'NONE',  ( -19.09188309203660694, 28.32812499999999645, 19.09188309203694800 ) ) ;
#14993 = CARTESIAN_POINT ( 'NONE',  ( -2.162160676586882350E-15, 4.875000002731200155, -35.31076352940722529 ) ) ;
#14994 = CARTESIAN_POINT ( 'NONE',  ( -7.543491769121417612, 19.16704833425730570, 28.00173670424549499 ) ) ;
#14995 = CARTESIAN_POINT ( 'NONE',  ( -15.04653450569338524, 14.14284749907602290, -25.98046417659831775 ) ) ;
#14996 = CARTESIAN_POINT ( 'NONE',  ( 27.16883889988623935, 2.325000002731183901, -19.73931689729374384 ) ) ;
#14997 = CARTESIAN_POINT ( 'NONE',  ( 32.50000000000000711, 2.899999999999995470, 10.55989012756945122 ) ) ;
#14998 = CARTESIAN_POINT ( 'NONE',  ( -26.29305231718578995, 42.20000000000000284, 19.10302069950538595 ) ) ;
#14999 = CARTESIAN_POINT ( 'NONE',  ( -27.16883889988624290, 44.92500000273119554, -19.73931689729374028 ) ) ;
#15000 = AXIS2_PLACEMENT_3D ( 'NONE', #33447, #21302, #15812 ) ;
#15001 = CARTESIAN_POINT ( 'NONE',  ( 23.41746825000000243, 2.524999997268798868, 7.608796670333735079 ) ) ;
#15002 = CARTESIAN_POINT ( 'NONE',  ( -6.988114217767819270, 65.85416666666665719, 26.07999730980490583 ) ) ;
#15003 = ORIENTED_EDGE ( 'NONE', *, *, #480, .F. ) ;
#15004 = CARTESIAN_POINT ( 'NONE',  ( -33.58253175000000113, 57.47500000273119269, 10.91162601494193929 ) ) ;
#15005 = CARTESIAN_POINT ( 'NONE',  ( 5.779280353836490358E-15, 19.00000000546237544, 32.49999999999999289 ) ) ;
#15006 = CARTESIAN_POINT ( 'NONE',  ( -18.94512977948576093, 13.82499999726882756, 13.76444248337722698 ) ) ;
#15007 = CARTESIAN_POINT ( 'NONE',  ( -13.94119854578936923, 37.64361083425730925, -24.22776226481241224 ) ) ;
#15008 = ORIENTED_EDGE ( 'NONE', *, *, #14495, .T. ) ;
#15009 = CARTESIAN_POINT ( 'NONE',  ( 10.37757302488624767, 29.72500000273119269, 31.93888565452638417 ) ) ;
#15010 = LINE ( 'NONE', #9166, #11566 ) ;
#15011 = ORIENTED_EDGE ( 'NONE', *, *, #27745, .F. ) ;
#15012 = DIRECTION ( 'NONE',  ( -1.000000000000000000, 0.000000000000000000, 0.000000000000000000 ) ) ;
#15013 = CARTESIAN_POINT ( 'NONE',  ( 6.486482029760649416E-15, 69.62500000273118417, 35.31076352940723240 ) ) ;
#15014 = CARTESIAN_POINT ( 'NONE',  ( 7.505752307972854531, 40.07291666666666430, -28.01184896238303423 ) ) ;
#15015 = ADVANCED_FACE ( 'NONE', ( #3046 ), #23305, .T. ) ;
#15016 = CARTESIAN_POINT ( 'NONE',  ( 19.82091636218621034, 13.80000000000000604, 14.40073868116559730 ) ) ;
#15017 = CARTESIAN_POINT ( 'NONE',  ( -7.236395654485757944, 3.724999997268802154, -22.27133577429736988 ) ) ;
#15018 = CARTESIAN_POINT ( 'NONE',  ( 33.58253175000000823, 8.025000002731188076, 10.91162601494192863 ) ) ;
#15019 = CARTESIAN_POINT ( 'NONE',  ( -24.50000000000000000, 6.749999994537625447, -3.000384657911015469E-15 ) ) ;
#15020 = CARTESIAN_POINT ( 'NONE',  ( 14.97647472619900455, 49.09076416574269786, -26.02091320914876960 ) ) ;
#15021 = CARTESIAN_POINT ( 'NONE',  ( -12.13525491562420910, 74.19999999999998863, 8.816778784387098611 ) ) ;
#15022 = CONICAL_SURFACE ( 'NONE', #13387, 10.17814985357208890, 0.2617993877991527385 ) ;
#15023 = CARTESIAN_POINT ( 'NONE',  ( -28.01184896238304134, 66.71354166666665719, -7.505752307972844761 ) ) ;
#15024 = CARTESIAN_POINT ( 'NONE',  ( -5.147494310547450880, 70.44874571845318201, 32.49999999999999289 ) ) ;
#15025 = AXIS2_PLACEMENT_3D ( 'NONE', #907, #14304, #19126 ) ;
#15026 = EDGE_CURVE ( 'NONE', #28636, #30070, #453, .T. ) ;
#15027 = ADVANCED_FACE ( 'NONE', ( #8347 ), #15589, .T. ) ;
#15028 = CARTESIAN_POINT ( 'NONE',  ( 5.779280353836490358E-15, 54.49999999999999289, 32.49999999999999289 ) ) ;
#15029 = CARTESIAN_POINT ( 'NONE',  ( -4.732186688966233175E-15, 13.24999999453763166, 25.76082449383753925 ) ) ;
#15030 = CARTESIAN_POINT ( 'NONE',  ( 2.897257156509938333E-15, 76.75000000546238255, 15.77193336357400710 ) ) ;
#15031 = CARTESIAN_POINT ( 'NONE',  ( 2.584737979205441561E-13, 24.46093749999999645, 27.95245687107222921 ) ) ;
#15032 = CARTESIAN_POINT ( 'NONE',  ( 27.16883889988623935, 30.32500000273119412, -19.73931689729374384 ) ) ;
#15033 = CARTESIAN_POINT ( 'NONE',  ( 11.25946833292375793, 71.67500000273119554, 8.180482586598731842 ) ) ;
#15034 = CARTESIAN_POINT ( 'NONE',  ( 20.75514604977248467, 44.67500000273118843, -28.56700777964554305 ) ) ;
#15035 = CARTESIAN_POINT ( 'NONE',  ( 6.486482029760648627E-15, 19.87500000273118772, 35.31076352940722529 ) ) ;
#15036 = CARTESIAN_POINT ( 'NONE',  ( -5.147494310547423346, 68.44874571845316780, 32.50000000000000000 ) ) ;
#15037 = EDGE_CURVE ( 'NONE', #14916, #5385, #19889, .T. ) ;
#15038 = CARTESIAN_POINT ( 'NONE',  ( 19.82091636218621389, 2.200000000000007283, -14.40073868116559197 ) ) ;
#15039 = CARTESIAN_POINT ( 'NONE',  ( 5.147494310547217289, 32.55125428154683931, 32.50000000000007105 ) ) ;
#15040 = CARTESIAN_POINT ( 'NONE',  ( 32.50000000000000000, 63.10000000000001563, -10.55989012756945833 ) ) ;
#15041 = CARTESIAN_POINT ( 'NONE',  ( -23.41746824999999887, 13.52499999726880198, -7.608796670333730638 ) ) ;
#15042 = CARTESIAN_POINT ( 'NONE',  ( -33.58253175000000113, 67.22500000273117848, 10.91162601494193929 ) ) ;
#15043 = CARTESIAN_POINT ( 'NONE',  ( 7.236395654485760609, 1.524999997268822183, -22.27133577429736633 ) ) ;
#15044 = CARTESIAN_POINT ( 'NONE',  ( -7.025853678916861966, 34.91107666574267654, -26.06988505166722803 ) ) ;
#15045 = CARTESIAN_POINT ( 'NONE',  ( 0.000000000000000000, 16.99999999999998579, 0.000000000000000000 ) ) ;
#15046 = CARTESIAN_POINT ( 'NONE',  ( 20.75514604977249178, 5.825000002731198556, 28.56700777964553950 ) ) ;
#15047 = CARTESIAN_POINT ( 'NONE',  ( -4.523095164977116484E-15, 10.62499999726880695, 24.62258325217400312 ) ) ;
#15048 = CARTESIAN_POINT ( 'NONE',  ( 19.09188309203694800, 58.40625000000000711, 19.09188309203660694 ) ) ;
#15049 = EDGE_LOOP ( 'NONE', ( #30960, #2455, #6011, #8662 ) ) ;
#15050 = CARTESIAN_POINT ( 'NONE',  ( 6.486482029760649416E-15, 51.62500000273120548, 35.31076352940723240 ) ) ;
#15051 = CARTESIAN_POINT ( 'NONE',  ( 33.58253175000000113, 22.37500000273119483, -4.112674001490185761E-15 ) ) ;
#15052 = EDGE_LOOP ( 'NONE', ( #28890, #14533, #21100, #24724 ) ) ;
#15053 = CARTESIAN_POINT ( 'NONE',  ( 20.50609665440969565, 33.48437500000000000, -20.50609665441004736 ) ) ;
#15054 = CARTESIAN_POINT ( 'NONE',  ( 30.02300923189239867, 28.47694416759064495, 0.04044903254992252006 ) ) ;
#15055 = CARTESIAN_POINT ( 'NONE',  ( -26.29305231718579350, 79.79999999999998295, -19.10302069950537884 ) ) ;
#15056 = CARTESIAN_POINT ( 'NONE',  ( -26.29305231718579350, 72.30000000546237970, -19.10302069950537884 ) ) ;
#15057 = CARTESIAN_POINT ( 'NONE',  ( 14.47279130897151589, 6.824999997268808904, 19.92008829642072953 ) ) ;
#15058 = CARTESIAN_POINT ( 'NONE',  ( 7.236395654485760609, 13.02499999726880375, -22.27133577429736633 ) ) ;
#15059 = CARTESIAN_POINT ( 'NONE',  ( -2.162160676586881955E-15, 16.87500000273120193, -35.31076352940723240 ) ) ;
#15060 = CARTESIAN_POINT ( 'NONE',  ( -32.50000000000000000, 22.50000000546237189, 0.000000000000000000 ) ) ;
#15061 = CARTESIAN_POINT ( 'NONE',  ( 10.04305231718578817, 63.40000000000001279, -30.90933677959249337 ) ) ;
#15062 = CARTESIAN_POINT ( 'NONE',  ( -1.877258788446258597, 74.00000000000004263, 14.08662250695439155 ) ) ;
#15063 = CARTESIAN_POINT ( 'NONE',  ( -28.00173670424549499, 64.71392333425730214, -7.543491769121417612 ) ) ;
#15064 = CARTESIAN_POINT ( 'NONE',  ( -27.16883889988624290, 27.17500000273118133, -19.73931689729374028 ) ) ;
#15065 = CARTESIAN_POINT ( 'NONE',  ( 13.91746824999999887, 80.37500000273118417, -1.704398294459741270E-15 ) ) ;
#15066 = CARTESIAN_POINT ( 'NONE',  ( 26.00068869287341045, 26.75260416666666075, -15.01150461594642493 ) ) ;
#15067 = CARTESIAN_POINT ( 'NONE',  ( -23.41746825000000598, 18.22499999726879949, 7.608796670333726198 ) ) ;
#15068 = CARTESIAN_POINT ( 'NONE',  ( 26.29305231718579350, 6.800000000000000711, 19.10302069950537529 ) ) ;
#15069 = CIRCLE ( 'NONE', #23848, 15.00000000000000000 ) ;
#15070 = CARTESIAN_POINT ( 'NONE',  ( -2.165007332552593587E-13, 52.50000000000000711, 32.50000000000000000 ) ) ;
#15071 = CARTESIAN_POINT ( 'NONE',  ( 26.06988505166722803, 56.39545166574268364, -7.025853678916862854 ) ) ;
#15072 = CARTESIAN_POINT ( 'NONE',  ( 33.58253175000000113, 54.12500000273118417, -4.112674001490185761E-15 ) ) ;
#15073 = CARTESIAN_POINT ( 'NONE',  ( -10.37757302488623701, 63.77500000273118985, 31.93888565452638417 ) ) ;
#15074 = CARTESIAN_POINT ( 'NONE',  ( 10.37757302488624767, 41.97500000273118559, 31.93888565452638417 ) ) ;
#15075 = CARTESIAN_POINT ( 'NONE',  ( -7.236395654485763274, 14.02499999726880553, 22.27133577429736633 ) ) ;
#15076 = PLANE ( 'NONE',  #21065 ) ;
#15077 = CARTESIAN_POINT ( 'NONE',  ( -20.08610463437157989, 49.70000000000000284, -27.64615127144129758 ) ) ;
#15078 = CARTESIAN_POINT ( 'NONE',  ( -7.570916362186210335, 4.349999994537640191, -23.30088464923126779 ) ) ;
#15079 = CARTESIAN_POINT ( 'NONE',  ( -20.08610463437157989, 27.69999999999999929, -27.64615127144129758 ) ) ;
#15080 = CARTESIAN_POINT ( 'NONE',  ( 20.75514604977249178, 23.82500000273118701, 28.56700777964553950 ) ) ;
#15081 = CARTESIAN_POINT ( 'NONE',  ( -26.29305231718579350, 62.30000000546237260, -19.10302069950537884 ) ) ;
#15082 = CARTESIAN_POINT ( 'NONE',  ( 26.29305231718578995, 55.70000000546236407, -19.10302069950538240 ) ) ;
#15083 = CARTESIAN_POINT ( 'NONE',  ( -13.91746824999999887, 71.12500000273119838, 0.000000000000000000 ) ) ;
#15084 = CARTESIAN_POINT ( 'NONE',  ( -25.98046417659831420, 61.40847249907603356, 15.04653450569339945 ) ) ;
#15085 = CARTESIAN_POINT ( 'NONE',  ( -10.04305231718578462, 38.90000000546238113, 30.90933677959249337 ) ) ;
#15086 = DIRECTION ( 'NONE',  ( -1.000000000000000000, -1.145572106777136737E-16, 0.000000000000000000 ) ) ;
#15087 = CARTESIAN_POINT ( 'NONE',  ( -10.37757302488623701, 35.52500000273117564, 31.93888565452638417 ) ) ;
#15088 = CARTESIAN_POINT ( 'NONE',  ( 27.95245687107222921, 37.35156249999997868, -2.463307335887066074E-13 ) ) ;
#15089 = ORIENTED_EDGE ( 'NONE', *, *, #13841, .F. ) ;
#15090 = ORIENTED_EDGE ( 'NONE', *, *, #14265, .T. ) ;
#15091 = CARTESIAN_POINT ( 'NONE',  ( 27.16883889988624290, 67.92500000273120975, 19.73931689729373673 ) ) ;
#15092 = CARTESIAN_POINT ( 'NONE',  ( -20.50609665440969209, 42.07812499999999289, 20.50609665441005092 ) ) ;
#15093 = PRESENTATION_LAYER_ASSIGNMENT (  '', '', ( #10711 ) ) ;
#15094 =( BOUNDED_CURVE ( )  B_SPLINE_CURVE ( 2, ( #3188, #13658, #1427, #4012, #2075, #6588, #32825, #11567, #12551, #32661, #23022, #22047, #3845 ),
 .UNSPECIFIED., .F., .T. ) 
 B_SPLINE_CURVE_WITH_KNOTS ( ( 3, 2, 2, 2, 2, 2, 3 ),
 ( 0.3055555555555555802, 0.3111111111111111160, 0.3222222222222222432, 0.3333333333333333148, 0.3444444444444444420, 0.3555555555555555691, 0.3611111111111111049 ),
 .UNSPECIFIED. ) 
 CURVE ( )  GEOMETRIC_REPRESENTATION_ITEM ( )  RATIONAL_B_SPLINE_CURVE ( ( 0.9755282581475767101, 0.9755282581475768211, 1.000000000000000000, 0.9510565162951535312, 1.000000000000000000, 0.9510565162951535312, 1.000000000000000000, 0.9510565162951535312, 1.000000000000000000, 0.9510565162951535312, 1.000000000000000000, 0.9755282581475768211, 0.9755282581475768211 ) ) 
 REPRESENTATION_ITEM ( '' )  );
#15095 = DIRECTION ( 'NONE',  ( 0.000000000000000000, -1.000000000000000000, 0.000000000000000000 ) ) ;
#15096 = ORIENTED_EDGE ( 'NONE', *, *, #25723, .F. ) ;
#15097 = CARTESIAN_POINT ( 'NONE',  ( -7.468012846824771955, 61.84934000092397355, -28.02196122052045624 ) ) ;
#15098 = CARTESIAN_POINT ( 'NONE',  ( 6.950374756619721595, 60.13059000092398065, 26.09010956794232428 ) ) ;
#15099 = ORIENTED_EDGE ( 'NONE', *, *, #1803, .T. ) ;
#15100 = CARTESIAN_POINT ( 'NONE',  ( 27.16883889988623935, 10.32500000273119056, -19.73931689729374384 ) ) ;
#15101 = CARTESIAN_POINT ( 'NONE',  ( -14.97647472619899389, 19.87201416574269075, 26.02091320914878025 ) ) ;
#15102 = CARTESIAN_POINT ( 'NONE',  ( -10.04305231718579172, 45.60000000000000142, -30.90933677959248982 ) ) ;
#15103 = CARTESIAN_POINT ( 'NONE',  ( -27.16883889988623935, 43.57500000273117990, 19.73931689729374739 ) ) ;
#15104 = CARTESIAN_POINT ( 'NONE',  ( 20.08610463437157279, 43.80000000546237970, -27.64615127144129758 ) ) ;
#15105 = CARTESIAN_POINT ( 'NONE',  ( 15.00000000000000000, 77.10000000000000853, -4.873795443493596835 ) ) ;
#15106 = CARTESIAN_POINT ( 'NONE',  ( -10.37757302488623701, 21.52500000273119340, 31.93888565452638417 ) ) ;
#15107 = CARTESIAN_POINT ( 'NONE',  ( -20.08610463437156923, 24.29999999999999005, 27.64615127144130113 ) ) ;
#15108 = CARTESIAN_POINT ( 'NONE',  ( 33.58253175000000113, 46.37500000273120548, -4.112674001490185761E-15 ) ) ;
#15109 =( NAMED_UNIT ( * ) SI_UNIT ( $, .STERADIAN. ) SOLID_ANGLE_UNIT ( ) );
#15110 = CARTESIAN_POINT ( 'NONE',  ( -32.50000000000000000, 31.90000000000001279, -10.55989012756945478 ) ) ;
#15111 = CARTESIAN_POINT ( 'NONE',  ( -32.50000000000000000, 27.99999999999999645, 0.000000000000000000 ) ) ;
#15112 = CARTESIAN_POINT ( 'NONE',  ( -19.82091636218621034, 0.7999999999999951594, -14.40073868116559552 ) ) ;
#15113 = CARTESIAN_POINT ( 'NONE',  ( 20.75514604977249178, 75.82500000273118701, 28.56700777964553950 ) ) ;
#15114 = DIRECTION ( 'NONE',  ( 0.000000000000000000, -1.000000000000000000, 0.000000000000000000 ) ) ;
#15115 = CARTESIAN_POINT ( 'NONE',  ( -24.50000000000000711, 15.09999999999998899, 7.960532557706201828 ) ) ;
#15116 = CARTESIAN_POINT ( 'NONE',  ( 33.58253175000000113, 60.37500000273119127, -4.112674001490185761E-15 ) ) ;
#15117 = CARTESIAN_POINT ( 'NONE',  ( 9.270509831248425314, 74.95000000546237118, 12.75976212528059683 ) ) ;
#15118 = VERTEX_POINT ( 'NONE', #2536 ) ;
#15119 = CARTESIAN_POINT ( 'NONE',  ( -33.58253175000000113, 17.12500000273120548, 0.000000000000000000 ) ) ;
#15120 = CARTESIAN_POINT ( 'NONE',  ( 24.50000000000000000, 9.749999994537628112, 0.000000000000000000 ) ) ;
#15121 = CARTESIAN_POINT ( 'NONE',  ( -26.06988505166735237, 23.46392333425730570, -7.025853678916388567 ) ) ;
#15122 = ADVANCED_FACE ( 'NONE', ( #281 ), #7838, .T. ) ;
#15123 = CARTESIAN_POINT ( 'NONE',  ( -1.778240108872766143E-15, 25.50000000000000711, -32.49999999999999289 ) ) ;
#15124 = CARTESIAN_POINT ( 'NONE',  ( -10.37757302488624411, 40.72500000273119980, -31.93888565452638417 ) ) ;
#15125 = CARTESIAN_POINT ( 'NONE',  ( -27.16883889988624290, 3.175000002731187543, -19.73931689729374028 ) ) ;
#15126 = CARTESIAN_POINT ( 'NONE',  ( -27.16883889988624290, 55.17500000273119554, -19.73931689729374028 ) ) ;
#15127 = CARTESIAN_POINT ( 'NONE',  ( -7.543491769121417612, 50.10454833425731636, 28.00173670424549499 ) ) ;
#15128 = EDGE_CURVE ( 'NONE', #22201, #7013, #31187, .T. ) ;
#15129 = CARTESIAN_POINT ( 'NONE',  ( 15.14183272437242067, 15.69999999999999929, 20.84094480462498211 ) ) ;
#15130 = CARTESIAN_POINT ( 'NONE',  ( -30.02300923189239867, 41.06993083240934794, 0.04044903255044988294 ) ) ;
#15131 = CARTESIAN_POINT ( 'NONE',  ( 6.277390505771533514E-15, 59.00000000546238255, 34.17252228774368916 ) ) ;
#15132 = CARTESIAN_POINT ( 'NONE',  ( -13.91746824999999887, 70.87500000273122680, 0.000000000000000000 ) ) ;
#15133 = CARTESIAN_POINT ( 'NONE',  ( 20.08610463437157279, 57.80000000546236549, -27.64615127144129758 ) ) ;
#15134 = CARTESIAN_POINT ( 'NONE',  ( -26.09010956794245217, 61.83815999907601935, -6.950374756619243755 ) ) ;
#15135 = DIRECTION ( 'NONE',  ( -0.000000000000000000, -1.000000000000000000, -0.000000000000000000 ) ) ;
#15136 = CARTESIAN_POINT ( 'NONE',  ( 10.04305231718579705, 75.10000000546237686, 30.90933677959248982 ) ) ;
#15137 = CARTESIAN_POINT ( 'NONE',  ( -1.089172066684569321E-14, 78.49999999999998579, 15.00000000000000000 ) ) ;
#15138 = CARTESIAN_POINT ( 'NONE',  ( 20.75514604977248467, 36.67500000273118843, -28.56700777964554305 ) ) ;
#15139 = CARTESIAN_POINT ( 'NONE',  ( -14.47279130897151767, 5.824999997268811569, -19.92008829642072598 ) ) ;
#15140 = ORIENTED_EDGE ( 'NONE', *, *, #12795, .F. ) ;
#15141 = CARTESIAN_POINT ( 'NONE',  ( -20.75514604977248112, 77.67500000273119554, 28.56700777964554661 ) ) ;
#15142 = CARTESIAN_POINT ( 'NONE',  ( -32.50000000000000000, 26.50000000546236123, 0.000000000000000000 ) ) ;
#15143 = CARTESIAN_POINT ( 'NONE',  ( -26.00068869287340334, 38.78385416666665719, 15.01150461594643382 ) ) ;
#15144 = CARTESIAN_POINT ( 'NONE',  ( 32.50000000000000711, 63.40000000546236691, 10.55989012756945122 ) ) ;
#15145 = ORIENTED_EDGE ( 'NONE', *, *, #16099, .T. ) ;
#15146 = CARTESIAN_POINT ( 'NONE',  ( 3.445340210940985210E-14, 7.499999999999994671, 24.50000000000000000 ) ) ;
#15147 = CARTESIAN_POINT ( 'NONE',  ( 33.58253175000000823, 46.02500000273118275, 10.91162601494192863 ) ) ;
#15148 = CARTESIAN_POINT ( 'NONE',  ( -7.236395654485763274, 18.02499999726880731, 22.27133577429736633 ) ) ;
#15149 = CARTESIAN_POINT ( 'NONE',  ( 6.277390505771533514E-15, 7.000000005462369224, 34.17252228774368916 ) ) ;
#15150 = DIRECTION ( 'NONE',  ( 0.000000000000000000, -1.000000000000000000, 0.000000000000000000 ) ) ;
#15151 = FACE_OUTER_BOUND ( 'NONE', #9765, .T. ) ;
#15152 = CARTESIAN_POINT ( 'NONE',  ( 20.08610463437157279, 49.29999999999998295, -27.64615127144129758 ) ) ;
#15153 = CARTESIAN_POINT ( 'NONE',  ( 5.779280353836490358E-15, 28.50000000000000355, 32.49999999999999289 ) ) ;
#15154 = CARTESIAN_POINT ( 'NONE',  ( -27.16883889988624290, 15.17500000273119909, -19.73931689729374028 ) ) ;
#15155 = CARTESIAN_POINT ( 'NONE',  ( 3.778760231354629433E-15, 0.5000000000000067724, -24.50000000000000355 ) ) ;
#15156 = CARTESIAN_POINT ( 'NONE',  ( -24.18731323226221974, 27.03347249907602290, 14.01125832528330406 ) ) ;
#15157 = CARTESIAN_POINT ( 'NONE',  ( -8.601468415847515203, 75.67500000273118133, 11.83890561707634959 ) ) ;
#15158 = FACE_OUTER_BOUND ( 'NONE', #13764, .T. ) ;
#15159 = CARTESIAN_POINT ( 'NONE',  ( -5.147494310547430452, 43.55125428154684641, -32.49999999999999289 ) ) ;
#15160 = CARTESIAN_POINT ( 'NONE',  ( -26.29305231718579350, 5.799999999999999822, -19.10302069950537884 ) ) ;
#15161 = ORIENTED_EDGE ( 'NONE', *, *, #30747, .T. ) ;
#15162 = CARTESIAN_POINT ( 'NONE',  ( -18.94512977948575738, 11.92499999726881477, -13.76444248337723231 ) ) ;
#15163 = CARTESIAN_POINT ( 'NONE',  ( -18.94512977948576093, 3.824999997268818674, 13.76444248337722698 ) ) ;
#15164 = CARTESIAN_POINT ( 'NONE',  ( 24.20753774853731244, 50.81510416666667140, -13.97622843553632599 ) ) ;
#15165 = CARTESIAN_POINT ( 'NONE',  ( 27.16883889988623935, 58.32500000273120833, -19.73931689729374384 ) ) ;
#15166 = CARTESIAN_POINT ( 'NONE',  ( -33.58253175000000113, 23.27500000273116854, -10.91162601494193218 ) ) ;
#15167 = CARTESIAN_POINT ( 'NONE',  ( 20.75514604977248467, 12.67500000273118488, -28.56700777964554305 ) ) ;
#15168 = CARTESIAN_POINT ( 'NONE',  ( 26.07999730980490227, 27.18229166666666430, 6.988114217767821046 ) ) ;
#15169 = CARTESIAN_POINT ( 'NONE',  ( 14.97647472619947351, 18.73736083425731636, 26.02091320914850314 ) ) ;
#15170 = CARTESIAN_POINT ( 'NONE',  ( 26.00068869287340334, 64.56510416666667140, -15.01150461594642316 ) ) ;
#15171 = EDGE_CURVE ( 'NONE', #1581, #1179, #21410, .T. ) ;
#15172 = CARTESIAN_POINT ( 'NONE',  ( -10.37757302488624411, 2.725000002731181592, -31.93888565452638417 ) ) ;
#15173 = CARTESIAN_POINT ( 'NONE',  ( 5.147494310547434893, 2.551254281546845082, 32.49999999999999289 ) ) ;
#15174 = CARTESIAN_POINT ( 'NONE',  ( 26.29305231718578995, 39.19999999999999574, -19.10302069950538240 ) ) ;
#15175 = CARTESIAN_POINT ( 'NONE',  ( 33.58253175000000113, 48.22500000273119269, -10.91162601494193574 ) ) ;
#15176 = CARTESIAN_POINT ( 'NONE',  ( 14.47279130897151589, 12.32499999726880802, 19.92008829642072953 ) ) ;
#15177 = CARTESIAN_POINT ( 'NONE',  ( 0.000000000000000000, 111.9999999999999858, 0.000000000000000000 ) ) ;
#15178 = ORIENTED_EDGE ( 'NONE', *, *, #15316, .F. ) ;
#15179 = CARTESIAN_POINT ( 'NONE',  ( -27.16883889988624290, 53.17500000273118843, -19.73931689729374028 ) ) ;
#15180 = CARTESIAN_POINT ( 'NONE',  ( 32.50000000000000000, 59.60000000546236976, -10.55989012756945833 ) ) ;
#15181 = CARTESIAN_POINT ( 'NONE',  ( 24.18731323226247554, 39.07590250092398065, 14.01125832528285997 ) ) ;
#15182 = ADVANCED_FACE ( 'NONE', ( #28949 ), #20744, .T. ) ;
#15183 = CARTESIAN_POINT ( 'NONE',  ( -27.16883889988623935, 73.57500000273120122, 19.73931689729374739 ) ) ;
#15184 = VERTEX_POINT ( 'NONE', #31354 ) ;
#15185 = CARTESIAN_POINT ( 'NONE',  ( -10.37757302488623701, 21.52500000273117919, 31.93888565452638417 ) ) ;
#15186 = CARTESIAN_POINT ( 'NONE',  ( 7.505752307972854531, 16.01041666666666075, -28.01184896238303423 ) ) ;
#15187 = ORIENTED_EDGE ( 'NONE', *, *, #32622, .F. ) ;
#15188 = DIRECTION ( 'NONE',  ( 0.000000000000000000, -1.000000000000000000, 0.000000000000000000 ) ) ;
#15189 = CARTESIAN_POINT ( 'NONE',  ( -2.162160676586881955E-15, 66.62500000273118417, -35.31076352940723240 ) ) ;
#15190 = CARTESIAN_POINT ( 'NONE',  ( -7.505752307973343918, 39.78645833333332860, -28.01184896238290989 ) ) ;
#15191 = AXIS2_PLACEMENT_3D ( 'NONE', #21970, #16825, #6679 ) ;
#15192 = CARTESIAN_POINT ( 'NONE',  ( -15.14183272437242600, 11.29999999999999361, 20.84094480462497856 ) ) ;
#15193 = CARTESIAN_POINT ( 'NONE',  ( 14.47279130897151944, 1.424999997268804997, -19.92008829642072598 ) ) ;
#15194 = CARTESIAN_POINT ( 'NONE',  ( -33.58253175000000113, 13.12500000273120193, 0.000000000000000000 ) ) ;
#15195 = CARTESIAN_POINT ( 'NONE',  ( 28.02196122052058413, 49.80690999907602645, 7.468012846824272799 ) ) ;
#15196 = CARTESIAN_POINT ( 'NONE',  ( 4.635254915624212657, 74.59999999999999432, 14.26584774442730286 ) ) ;
#15197 = CARTESIAN_POINT ( 'NONE',  ( 2.375766604868043697, 80.55125428154687484, 15.00000000000000178 ) ) ;
#15198 = CARTESIAN_POINT ( 'NONE',  ( -32.50000000000000000, 70.09999999999999432, 10.55989012756946366 ) ) ;
#15199 = CARTESIAN_POINT ( 'NONE',  ( 26.29305231718579350, 61.30000000546237260, 19.10302069950537529 ) ) ;
#15200 = CARTESIAN_POINT ( 'NONE',  ( 1.577395562988744260E-15, 12.24999999453763522, -25.76082449383753925 ) ) ;
#15201 = CARTESIAN_POINT ( 'NONE',  ( -8.960552108402742093E-16, 80.37500000273115575, -14.63369212191046387 ) ) ;
#15202 = CARTESIAN_POINT ( 'NONE',  ( 6.988114217767829928, 19.44791666666666075, -26.07999730980489872 ) ) ;
#15203 = CARTESIAN_POINT ( 'NONE',  ( -27.16883889988623935, 31.32500000273119412, 19.73931689729374739 ) ) ;
#15204 = CARTESIAN_POINT ( 'NONE',  ( 4.635254915624209993, 75.40000000000001990, -14.26584774442730463 ) ) ;
#15205 = CARTESIAN_POINT ( 'NONE',  ( 6.486482029760649416E-15, 41.87500000273119127, 35.31076352940723240 ) ) ;
#15206 = CARTESIAN_POINT ( 'NONE',  ( -2.162160676586882350E-15, 22.87500000273118062, -35.31076352940722529 ) ) ;
#15207 = CARTESIAN_POINT ( 'NONE',  ( -10.04305231718578462, 68.40000000000001990, 30.90933677959249337 ) ) ;
#15208 = CARTESIAN_POINT ( 'NONE',  ( -10.37757302488624411, 78.72500000273119269, -31.93888565452638417 ) ) ;
#15209 = CARTESIAN_POINT ( 'NONE',  ( 3.880418787951159132, 8.448745718453144704, -24.49999999999999289 ) ) ;
#15210 = CARTESIAN_POINT ( 'NONE',  ( 32.50000000000000711, 60.89999999999999147, 10.55989012756945122 ) ) ;
#15211 = CARTESIAN_POINT ( 'NONE',  ( 14.47279130897151944, 16.92499999726880944, -19.92008829642072598 ) ) ;
#15212 = CARTESIAN_POINT ( 'NONE',  ( 20.75514604977248467, 64.42500000273116711, -28.56700777964554305 ) ) ;
#15213 = CARTESIAN_POINT ( 'NONE',  ( 7.236395654485760609, 9.524999997268828622, -22.27133577429736633 ) ) ;
#15214 = CARTESIAN_POINT ( 'NONE',  ( 0.04044903255044120238, 43.64805583240936215, 27.95245687107223276 ) ) ;
#15215 = CARTESIAN_POINT ( 'NONE',  ( 20.75514604977248467, 74.67500000273118133, -28.56700777964554305 ) ) ;
#15216 = CARTESIAN_POINT ( 'NONE',  ( 27.16883889988624290, 7.925000002731191984, 19.73931689729373673 ) ) ;
#15217 = CARTESIAN_POINT ( 'NONE',  ( -18.94512977948575738, 13.92499999726881654, -13.76444248337723231 ) ) ;
#15218 = CARTESIAN_POINT ( 'NONE',  ( -19.09188309203694445, 63.56249999999999289, -19.09188309203661049 ) ) ;
#15219 = EDGE_LOOP ( 'NONE', ( #20933, #8378, #22017, #23879 ) ) ;
#15220 = CARTESIAN_POINT ( 'NONE',  ( 20.75514604977248467, 48.42500000273119554, -28.56700777964554305 ) ) ;
#15221 = ORIENTED_EDGE ( 'NONE', *, *, #30248, .T. ) ;
#15222 = CARTESIAN_POINT ( 'NONE',  ( -26.00068869287368756, 35.91927083333332860, -15.01150461594595775 ) ) ;
#15223 = DIRECTION ( 'NONE',  ( -1.000000000000000000, -1.063101997391471025E-16, 0.000000000000000000 ) ) ;
#15224 = CARTESIAN_POINT ( 'NONE',  ( -20.08610463437157989, 10.20000000546238539, -27.64615127144129758 ) ) ;
#15225 = DIRECTION ( 'NONE',  ( -0.000000000000000000, -1.000000000000000000, -0.000000000000000000 ) ) ;
#15226 = CARTESIAN_POINT ( 'NONE',  ( -23.41746824999999887, 4.124999997268813168, -2.867812753649727150E-15 ) ) ;
#15227 = CARTESIAN_POINT ( 'NONE',  ( -23.41746825000000598, 11.72499999726882614, 7.608796670333726198 ) ) ;
#15228 = CARTESIAN_POINT ( 'NONE',  ( -20.75514604977248112, 15.67500000273117600, 28.56700777964554661 ) ) ;
#15229 = CARTESIAN_POINT ( 'NONE',  ( 20.08610463437157279, 17.80000000546237615, -27.64615127144129758 ) ) ;
#15230 = CARTESIAN_POINT ( 'NONE',  ( 32.50000000000000711, 64.89999999999997726, 10.55989012756945122 ) ) ;
#15231 = CARTESIAN_POINT ( 'NONE',  ( 15.00000000000000000, 77.35000000546237686, -4.873795443493596835 ) ) ;
#15232 = CARTESIAN_POINT ( 'NONE',  ( -33.04126587500000056, 79.68750000136559208, 0.000000000000000000 ) ) ;
#15233 = CARTESIAN_POINT ( 'NONE',  ( -20.47846945139902175, 61.56288166759063074, -20.53372385742072481 ) ) ;
#15234 = CARTESIAN_POINT ( 'NONE',  ( 20.75514604977248467, 28.67500000273117777, -28.56700777964554305 ) ) ;
#15235 = CARTESIAN_POINT ( 'NONE',  ( 8.601468415847520532, 80.07500000273118701, 11.83890561707634781 ) ) ;
#15236 = CARTESIAN_POINT ( 'NONE',  ( -26.00068869287340334, 38.78385416666665719, 15.01150461594643559 ) ) ;
#15237 = CARTESIAN_POINT ( 'NONE',  ( 0.000000000000000000, 0.000000000000000000, 0.000000000000000000 ) ) ;
#15238 = CARTESIAN_POINT ( 'NONE',  ( -7.236395654485757944, 15.72499999726881192, -22.27133577429736988 ) ) ;
#15239 = CARTESIAN_POINT ( 'NONE',  ( -20.08610463437156923, 10.29999999999999361, 27.64615127144130113 ) ) ;
#15240 = VECTOR ( 'NONE', #5792, 1000.000000000000000 ) ;
#15241 = CARTESIAN_POINT ( 'NONE',  ( 1.577395562988744260E-15, 16.50000000000000000, -25.76082449383753925 ) ) ;
#15242 = CARTESIAN_POINT ( 'NONE',  ( -6.950374756619247307, 54.10378499907602645, 26.09010956794245217 ) ) ;
#15243 = CARTESIAN_POINT ( 'NONE',  ( -33.58253175000000113, 47.22500000273117138, 10.91162601494193929 ) ) ;
#15244 = CARTESIAN_POINT ( 'NONE',  ( -10.37757302488623701, 61.77500000273118985, 31.93888565452638417 ) ) ;
#15245 = CARTESIAN_POINT ( 'NONE',  ( -20.75514604977248112, 43.67500000273119554, 28.56700777964554661 ) ) ;
#15246 = DIRECTION ( 'NONE',  ( 0.000000000000000000, 0.000000000000000000, -1.000000000000000000 ) ) ;
#15247 = CARTESIAN_POINT ( 'NONE',  ( -19.09188309203694445, 15.43749999999999645, -19.09188309203661049 ) ) ;
#15248 = CARTESIAN_POINT ( 'NONE',  ( -15.14183272437242067, 8.699999999999986855, -20.84094480462497856 ) ) ;
#15249 = ADVANCED_FACE ( 'NONE', ( #33936 ), #10598, .F. ) ;
#15250 = CARTESIAN_POINT ( 'NONE',  ( 5.147494310547327423, 51.05125428700922896, 32.50000000000003553 ) ) ;
#15251 = CARTESIAN_POINT ( 'NONE',  ( 32.50000000000000000, 79.10000000000000853, -10.55989012756945833 ) ) ;
#15252 = CARTESIAN_POINT ( 'NONE',  ( 27.16883889988624290, 17.92500000273118843, 19.73931689729373673 ) ) ;
#15253 = CARTESIAN_POINT ( 'NONE',  ( 20.08610463437158344, 6.699999999999991296, 27.64615127144129403 ) ) ;
#15254 = CARTESIAN_POINT ( 'NONE',  ( -15.14183272437242778, 13.04999999453763770, 20.84094480462497856 ) ) ;
#15255 = CARTESIAN_POINT ( 'NONE',  ( 5.147494310547426899, 41.94874572391552192, -32.50000000000000000 ) ) ;
#15256 = CARTESIAN_POINT ( 'NONE',  ( -19.06425588902558133, 23.45274333240935150, 19.11951029504797006 ) ) ;
#15257 = CARTESIAN_POINT ( 'NONE',  ( 20.08610463437158344, 43.20000000546235697, 27.64615127144129403 ) ) ;
#15258 = CARTESIAN_POINT ( 'NONE',  ( -1.778240108872766143E-15, 11.49999999999999112, -32.49999999999999289 ) ) ;
#15259 = CARTESIAN_POINT ( 'NONE',  ( -20.75514604977248823, 24.82500000273117635, -28.56700777964554305 ) ) ;
#15260 = ADVANCED_BREP_SHAPE_REPRESENTATION ( '', ( #33133, #1376 ), #231 ) ;
#15261 = CARTESIAN_POINT ( 'NONE',  ( 2.584737979205441561E-13, 38.21093750000000000, 27.95245687107222921 ) ) ;
#15262 = VERTEX_POINT ( 'NONE', #23982 ) ;
#15263 = CARTESIAN_POINT ( 'NONE',  ( -27.16883889988624290, 68.92500000273120975, -19.73931689729374028 ) ) ;
#15264 = CARTESIAN_POINT ( 'NONE',  ( 7.505752307972854531, 43.51041666666666430, -28.01184896238303423 ) ) ;
#15265 = DIRECTION ( 'NONE',  ( -1.000000000000000000, 0.000000000000000000, 0.000000000000000000 ) ) ;
#15266 = ORIENTED_EDGE ( 'NONE', *, *, #17014, .F. ) ;
#15267 = CARTESIAN_POINT ( 'NONE',  ( 0.04044903254992426173, 55.11756916759064495, -30.02300923189239867 ) ) ;
#15268 = CARTESIAN_POINT ( 'NONE',  ( 24.22776226481241224, 62.56548583425730925, -13.94119854578936923 ) ) ;
#15269 = ORIENTED_EDGE ( 'NONE', *, *, #6933, .F. ) ;
#15270 = CARTESIAN_POINT ( 'NONE',  ( 6.486482029760649416E-15, 9.625000002731178839, 35.31076352940723240 ) ) ;
#15271 = CARTESIAN_POINT ( 'NONE',  ( 0.04044903255045854962, 16.14805583240936215, 30.02300923189239867 ) ) ;
#15272 = LINE ( 'NONE', #28137, #26165 ) ;
#15273 = CARTESIAN_POINT ( 'NONE',  ( 33.58253175000000823, 34.27500000273116854, 10.91162601494192863 ) ) ;
#15274 = CARTESIAN_POINT ( 'NONE',  ( -32.50000000000000000, 44.40000000546238823, -10.55989012756945478 ) ) ;
#15275 = CARTESIAN_POINT ( 'NONE',  ( 4.635254915624212657, 74.59999999999999432, 14.26584774442730286 ) ) ;
#15276 = CARTESIAN_POINT ( 'NONE',  ( -10.37757302488623701, 23.52500000273119340, 31.93888565452638417 ) ) ;
#15277 = CARTESIAN_POINT ( 'NONE',  ( 1.555960095263670572E-15, 14.24999999453762278, -24.50000000000000000 ) ) ;
#15278 = CARTESIAN_POINT ( 'NONE',  ( -10.37757302488623701, 51.77500000273118985, 31.93888565452638417 ) ) ;
#15279 = SHAPE_REPRESENTATION_RELATIONSHIP ( 'NONE' , 'NONE' ,  #15301, #22997 ) ;
#15280 = CARTESIAN_POINT ( 'NONE',  ( -10.04305231718578462, 26.39999999999999147, 30.90933677959249337 ) ) ;
#15281 = CARTESIAN_POINT ( 'NONE',  ( -26.29305231718578995, 30.20000000000000284, 19.10302069950538595 ) ) ;
#15282 = CARTESIAN_POINT ( 'NONE',  ( -24.50000000000001066, 1.099999999999994094, 7.960532557706201828 ) ) ;
#15283 = CARTESIAN_POINT ( 'NONE',  ( 33.58253175000000823, 68.02500000273117564, 10.91162601494192863 ) ) ;
#15284 = CARTESIAN_POINT ( 'NONE',  ( -2.708425130540669024, 66.99999999999998579, 32.46185396738155049 ) ) ;
#15285 = CARTESIAN_POINT ( 'NONE',  ( -8.601468415847518756, 75.07500000273118701, -11.83890561707634603 ) ) ;
#15286 = CARTESIAN_POINT ( 'NONE',  ( 33.58253175000000113, 60.47500000273118559, -10.91162601494193574 ) ) ;
#15287 = CARTESIAN_POINT ( 'NONE',  ( -8.960552108402742093E-16, 80.37500000273118417, -14.63369212191046387 ) ) ;
#15288 = CARTESIAN_POINT ( 'NONE',  ( 20.08610463437157279, 39.80000000546238681, -27.64615127144129758 ) ) ;
#15289 = CARTESIAN_POINT ( 'NONE',  ( 20.75514604977249178, 17.82500000273120122, 28.56700777964553950 ) ) ;
#15290 = CARTESIAN_POINT ( 'NONE',  ( -4.732186688966233175E-15, 9.249999994537640546, 25.76082449383753925 ) ) ;
#15291 = CARTESIAN_POINT ( 'NONE',  ( 26.06988505166735592, 18.30767333425730214, 7.025853678916393896 ) ) ;
#15292 = DIRECTION ( 'NONE',  ( -0.000000000000000000, -1.000000000000000000, -0.000000000000000000 ) ) ;
#15293 = CARTESIAN_POINT ( 'NONE',  ( -27.16883889988623935, 41.32500000273119412, 19.73931689729374739 ) ) ;
#15294 = CARTESIAN_POINT ( 'NONE',  ( -32.50000000000000000, 64.60000000546239107, 10.55989012756946366 ) ) ;
#15295 = CARTESIAN_POINT ( 'NONE',  ( 20.75514604977249178, 58.07500000273117990, 28.56700777964553950 ) ) ;
#15296 = CARTESIAN_POINT ( 'NONE',  ( -26.02091320914849959, 50.53423583425731636, 14.97647472619947528 ) ) ;
#15297 = DIRECTION ( 'NONE',  ( 1.000000000000000000, 0.000000000000000000, 0.000000000000000000 ) ) ;
#15298 = CARTESIAN_POINT ( 'NONE',  ( -26.02091320914878025, 41.35638916574269075, -14.97647472619899389 ) ) ;
#15299 = CARTESIAN_POINT ( 'NONE',  ( 20.08610463437158344, 63.20000000546237118, 27.64615127144129403 ) ) ;
#15300 = CARTESIAN_POINT ( 'NONE',  ( -8.601468415847518756, 79.07500000273118701, -11.83890561707634781 ) ) ;
#15301 = SHAPE_REPRESENTATION ( 'level compensator', ( #1376 ), #21134 ) ;
#15302 = CARTESIAN_POINT ( 'NONE',  ( -1.778240108872766143E-15, 33.50000000000000000, -32.49999999999999289 ) ) ;
#15303 = CARTESIAN_POINT ( 'NONE',  ( -26.06988505166722803, 61.55170166574269786, 7.025853678916877953 ) ) ;
#15304 = CARTESIAN_POINT ( 'NONE',  ( -18.94512977948575738, 1.924999997268805885, -13.76444248337723231 ) ) ;
#15305 = CARTESIAN_POINT ( 'NONE',  ( 26.29305231718579350, 75.30000000546237970, 19.10302069950537529 ) ) ;
#15306 = CARTESIAN_POINT ( 'NONE',  ( -20.50609665440969209, 14.57812499999999645, 20.50609665441005092 ) ) ;
#15307 = CARTESIAN_POINT ( 'NONE',  ( -20.75514604977248823, 33.07500000273117990, -28.56700777964554305 ) ) ;
#15308 = CARTESIAN_POINT ( 'NONE',  ( -23.41746824999999887, 6.124999997268814944, -2.867812753649727150E-15 ) ) ;
#15309 = ORIENTED_EDGE ( 'NONE', *, *, #1942, .T. ) ;
#15310 = CARTESIAN_POINT ( 'NONE',  ( 27.16883889988623935, 76.57500000273120122, -19.73931689729374384 ) ) ;
#15311 = CARTESIAN_POINT ( 'NONE',  ( -32.50000000000000000, 24.50000000546238965, 0.000000000000000000 ) ) ;
#15312 = CARTESIAN_POINT ( 'NONE',  ( 7.505752307972854531, 43.51041666666666430, -28.01184896238303423 ) ) ;
#15313 = CARTESIAN_POINT ( 'NONE',  ( -7.505752307973343918, 60.41145833333332149, -28.01184896238290989 ) ) ;
#15314 = CARTESIAN_POINT ( 'NONE',  ( -20.75514604977248823, 53.07500000273118701, -28.56700777964554305 ) ) ;
#15315 = CARTESIAN_POINT ( 'NONE',  ( -10.04305231718579172, 64.10000000546240528, -30.90933677959248982 ) ) ;
#15317 = VERTEX_POINT ( 'NONE', #26041 ) ;
#15316 = EDGE_CURVE ( 'NONE', #18620, #15868, #374, .T. ) ;
#15318 = CARTESIAN_POINT ( 'NONE',  ( -4.223320258572819786E-15, 15.24999999453762278, 24.50000000000000000 ) ) ;
#15319 = CARTESIAN_POINT ( 'NONE',  ( 20.75514604977249178, 43.82500000273119412, 28.56700777964553950 ) ) ;
#15320 = DIRECTION ( 'NONE',  ( 0.000000000000000000, 0.000000000000000000, -1.000000000000000000 ) ) ;
#15321 = CARTESIAN_POINT ( 'NONE',  ( 20.75514604977249178, 66.07500000273118701, 28.56700777964553950 ) ) ;
#15322 = EDGE_CURVE ( 'NONE', #27023, #25888, #20106, .T. ) ;
#15323 = CARTESIAN_POINT ( 'NONE',  ( -32.50000000000000000, 4.400000005462393560, -10.55989012756945478 ) ) ;
#15324 = CARTESIAN_POINT ( 'NONE',  ( -27.16883889988623935, 59.32500000273120833, 19.73931689729374739 ) ) ;
#15325 = FACE_OUTER_BOUND ( 'NONE', #21891, .T. ) ;
#15326 = CARTESIAN_POINT ( 'NONE',  ( 32.50000000000000711, 44.90000000000001279, 10.55989012756945122 ) ) ;
#15327 = CARTESIAN_POINT ( 'NONE',  ( -1.778240108872766143E-15, 13.50000000000000355, -32.49999999999999289 ) ) ;
#15328 = CARTESIAN_POINT ( 'NONE',  ( -10.37757302488624411, 14.97500000273119269, -31.93888565452638417 ) ) ;
#15329 = CARTESIAN_POINT ( 'NONE',  ( 5.779280353836490358E-15, 74.50000000000001421, 32.49999999999999289 ) ) ;
#15330 = CARTESIAN_POINT ( 'NONE',  ( 24.18731323226221974, 28.75222249907602290, -14.01125832528328985 ) ) ;
#15331 = CARTESIAN_POINT ( 'NONE',  ( -8.601468415847515203, 79.67500000273118133, 11.83890561707634959 ) ) ;
#15332 = DIRECTION ( 'NONE',  ( -1.224646799147353454E-16, 1.000000000000000000, -0.000000000000000000 ) ) ;
#15333 = CARTESIAN_POINT ( 'NONE',  ( -5.147494310547423346, 22.44874571845314648, 32.50000000000000000 ) ) ;
#15334 = CARTESIAN_POINT ( 'NONE',  ( -27.16883889988623935, 75.57500000273118701, 19.73931689729374739 ) ) ;
#15335 = ORIENTED_EDGE ( 'NONE', *, *, #3903, .F. ) ;
#15336 = CARTESIAN_POINT ( 'NONE',  ( -23.41746825000000243, 14.02499999726881263, -7.608796670333730638 ) ) ;
#15337 = CARTESIAN_POINT ( 'NONE',  ( 7.236395654485760609, 5.024999997268825069, -22.27133577429736633 ) ) ;
#15338 = CARTESIAN_POINT ( 'NONE',  ( 26.07999730980490227, 51.24479166666666430, 6.988114217767821046 ) ) ;
#15339 = CARTESIAN_POINT ( 'NONE',  ( 10.37757302488624767, 59.72500000273119269, 31.93888565452638417 ) ) ;
#15340 = CARTESIAN_POINT ( 'NONE',  ( 33.58253175000000823, 16.27500000273118630, 10.91162601494192863 ) ) ;
#15341 = CARTESIAN_POINT ( 'NONE',  ( -10.37757302488623701, 7.775000002731194293, 31.93888565452638417 ) ) ;
#15342 = CARTESIAN_POINT ( 'NONE',  ( 13.97622843553589966, 29.90364583333332860, -24.20753774853756113 ) ) ;
#15343 = UNCERTAINTY_MEASURE_WITH_UNIT (LENGTH_MEASURE( 1.000000000000000082E-05 ), #13718, 'distance_accuracy_value', 'NONE');
#15344 = CARTESIAN_POINT ( 'NONE',  ( -28.02196122052045268, 23.17746500092398065, 7.468012846824790607 ) ) ;
#15345 = CARTESIAN_POINT ( 'NONE',  ( -20.50609665441004736, 63.56249999999999289, -20.50609665440969565 ) ) ;
#15346 = CARTESIAN_POINT ( 'NONE',  ( 20.75514604977249178, 3.825000002731188786, 28.56700777964553950 ) ) ;
#15347 = CARTESIAN_POINT ( 'NONE',  ( -8.601468415847515203, 71.67500000273118133, 11.83890561707634959 ) ) ;
#15348 = CARTESIAN_POINT ( 'NONE',  ( 10.04305231718579705, 42.60000000000001563, 30.90933677959248982 ) ) ;
#15349 = CARTESIAN_POINT ( 'NONE',  ( 33.58253175000000823, 46.02500000273118275, 10.91162601494192685 ) ) ;
#15350 = CARTESIAN_POINT ( 'NONE',  ( -7.236395654485757944, 7.224999997268804819, -22.27133577429736988 ) ) ;
#15351 = PRODUCT_DEFINITION_SHAPE ( 'NONE', 'NONE',  #33997 ) ;
#15352 = CARTESIAN_POINT ( 'NONE',  ( -19.09188309203694445, 67.00000000000000000, -19.09188309203661049 ) ) ;
#15353 = ORIENTED_EDGE ( 'NONE', *, *, #15453, .T. ) ;
#15354 = CARTESIAN_POINT ( 'NONE',  ( -20.75514604977248112, 55.67500000273118843, 28.56700777964554661 ) ) ;
#15355 = CARTESIAN_POINT ( 'NONE',  ( 26.29305231718578995, 59.70000000546237118, -19.10302069950538240 ) ) ;
#15356 = CARTESIAN_POINT ( 'NONE',  ( 19.06425588902592239, 46.09413166759064495, 19.11951029504763611 ) ) ;
#15357 = CARTESIAN_POINT ( 'NONE',  ( -2.162160676586881955E-15, 78.87500000273118417, -35.31076352940723240 ) ) ;
#15358 = ORIENTED_EDGE ( 'NONE', *, *, #11041, .T. ) ;
#15359 = CARTESIAN_POINT ( 'NONE',  ( 6.486482029760649416E-15, 21.62500000273119483, 35.31076352940723240 ) ) ;
#15360 = CARTESIAN_POINT ( 'NONE',  ( -15.01150461594642138, 19.01822916666666785, -26.00068869287340334 ) ) ;
#15361 = EDGE_CURVE ( 'NONE', #25643, #12120, #26213, .T. ) ;
#15362 = ORIENTED_EDGE ( 'NONE', *, *, #27766, .T. ) ;
#15363 = CARTESIAN_POINT ( 'NONE',  ( -26.29305231718578995, 58.20000000000001705, 19.10302069950538595 ) ) ;
#15364 = CARTESIAN_POINT ( 'NONE',  ( -2.162160676586881955E-15, 62.62500000273116996, -35.31076352940723240 ) ) ;
#15365 = CARTESIAN_POINT ( 'NONE',  ( -15.01150461594642138, 36.20572916666666430, -26.00068869287340334 ) ) ;
#15366 = FACE_OUTER_BOUND ( 'NONE', #3031, .T. ) ;
#15367 = CARTESIAN_POINT ( 'NONE',  ( 0.000000000000000000, -10.99999999999999645, 0.000000000000000000 ) ) ;
#15368 = CARTESIAN_POINT ( 'NONE',  ( 33.58253175000000113, 8.225000002731182036, -10.91162601494193751 ) ) ;
#15369 = CARTESIAN_POINT ( 'NONE',  ( 20.47846945139867003, 52.67149333240935505, -20.53372385742107653 ) ) ;
#15370 = CARTESIAN_POINT ( 'NONE',  ( 9.270509831248425314, 76.70000000000000284, 12.75976212528059683 ) ) ;
#15371 = CARTESIAN_POINT ( 'NONE',  ( 8.891200544363830713E-16, 81.50000000000001421, -15.00000000000000000 ) ) ;
#15372 = CARTESIAN_POINT ( 'NONE',  ( -15.14183272437242067, 14.44999999453762207, -20.84094480462497856 ) ) ;
#15373 = CARTESIAN_POINT ( 'NONE',  ( 32.50000000000000000, 17.00000000000000000, -3.980102097228898626E-15 ) ) ;
#15374 = CARTESIAN_POINT ( 'NONE',  ( 7.570916362186213000, 10.14999999453763913, -23.30088464923126423 ) ) ;
#15375 = CARTESIAN_POINT ( 'NONE',  ( -15.00000000000000000, 74.15000000546237402, -4.873795443493594171 ) ) ;
#15376 = CARTESIAN_POINT ( 'NONE',  ( 19.09188309203661049, 26.60937499999999645, -19.09188309203694445 ) ) ;
#15377 = CARTESIAN_POINT ( 'NONE',  ( -20.75514604977248112, 33.42500000273120264, 28.56700777964554661 ) ) ;
#15378 = PRODUCT_DEFINITION_SHAPE ( 'NONE', 'NONE',  #18358 ) ;
#15379 = CARTESIAN_POINT ( 'NONE',  ( 4.635254915624212657, 74.59999999999999432, 14.26584774442730286 ) ) ;
#15380 = CARTESIAN_POINT ( 'NONE',  ( -33.58253175000000113, 41.47500000273117138, 10.91162601494193929 ) ) ;
#15381 = CARTESIAN_POINT ( 'NONE',  ( -2.162160676586882350E-15, 24.87500000273117706, -35.31076352940722529 ) ) ;
#15382 = CARTESIAN_POINT ( 'NONE',  ( -4.635254915624211769, 79.60000000000000853, -14.26584774442730286 ) ) ;
#15383 = CARTESIAN_POINT ( 'NONE',  ( 10.37757302488624056, 74.52500000273118985, -31.93888565452638417 ) ) ;
#15384 = CARTESIAN_POINT ( 'NONE',  ( 32.50000000000000000, 59.60000000546236976, -10.55989012756945833 ) ) ;
#15385 = CARTESIAN_POINT ( 'NONE',  ( -20.08610463437157989, 61.69999999999999574, -27.64615127144129758 ) ) ;
#15386 = CARTESIAN_POINT ( 'NONE',  ( -14.47279130897151767, 17.32499999726882578, -19.92008829642072598 ) ) ;
#15387 = CARTESIAN_POINT ( 'NONE',  ( 33.58253175000000113, 62.22500000273119269, -10.91162601494193574 ) ) ;
#15388 = CARTESIAN_POINT ( 'NONE',  ( 1.507698388325705758E-15, 5.624999997268818497, -24.62258325217400312 ) ) ;
#15389 = CARTESIAN_POINT ( 'NONE',  ( 6.486482029760649416E-15, 73.87500000273119838, 35.31076352940723240 ) ) ;
#15390 = CARTESIAN_POINT ( 'NONE',  ( -20.75514604977248112, 7.425000002731177773, 28.56700777964554661 ) ) ;
#15391 = CARTESIAN_POINT ( 'NONE',  ( 18.94512977948575738, 18.92499999726882010, 13.76444248337723408 ) ) ;
#15392 = CARTESIAN_POINT ( 'NONE',  ( 27.95245687107223986, 11.28944416759064140, 0.04044903254993640479 ) ) ;
#15393 = VERTEX_POINT ( 'NONE', #23815 ) ;
#15394 = CARTESIAN_POINT ( 'NONE',  ( 10.37757302488624056, 44.52500000273119696, -31.93888565452638417 ) ) ;
#15395 =( BOUNDED_CURVE ( )  B_SPLINE_CURVE ( 2, ( #24671, #5820, #981, #8384, #9054, #29814, #21611, #488, #32228, #1145, #16793, #24181, #8717 ),
 .UNSPECIFIED., .F., .T. ) 
 B_SPLINE_CURVE_WITH_KNOTS ( ( 3, 2, 2, 2, 2, 2, 3 ),
 ( 0.5833333333333332593, 0.5888888888888889062, 0.5999999999999999778, 0.6111111111111111605, 0.6222222222222222321, 0.6333333333333333037, 0.6388888888888889506 ),
 .UNSPECIFIED. ) 
 CURVE ( )  GEOMETRIC_REPRESENTATION_ITEM ( )  RATIONAL_B_SPLINE_CURVE ( ( 0.9755282581475768211, 0.9755282581475765991, 1.000000000000000000, 0.9510565162951535312, 1.000000000000000000, 0.9510565162951535312, 1.000000000000000000, 0.9510565162951535312, 1.000000000000000000, 0.9510565162951535312, 1.000000000000000000, 0.9755282581475765991, 0.9755282581475768211 ) ) 
 REPRESENTATION_ITEM ( '' )  );
#15396 = ORIENTED_EDGE ( 'NONE', *, *, #20791, .T. ) ;
#15397 = CARTESIAN_POINT ( 'NONE',  ( -20.50609665441004736, 39.49999999999999289, -20.50609665440969565 ) ) ;
#15398 = CYLINDRICAL_SURFACE ( 'NONE', #23757, 12.00000000000000178 ) ;
#15399 = CARTESIAN_POINT ( 'NONE',  ( 10.04305231718578817, 1.900000005462379349, -30.90933677959249337 ) ) ;
#15400 = CARTESIAN_POINT ( 'NONE',  ( -32.50000000000000000, 72.09999999999999432, 10.55989012756946366 ) ) ;
#15401 = CARTESIAN_POINT ( 'NONE',  ( 18.94512977948576093, 3.324999997268818230, -13.76444248337722875 ) ) ;
#15402 = CARTESIAN_POINT ( 'NONE',  ( 18.94512977948575738, 12.42499999726881477, 13.76444248337723408 ) ) ;
#15403 = CARTESIAN_POINT ( 'NONE',  ( -33.58253175000000113, 15.47500000273118381, 10.91162601494193929 ) ) ;
#15404 = CARTESIAN_POINT ( 'NONE',  ( -10.04305231718578462, 18.90000000546238113, 30.90933677959249337 ) ) ;
#15405 = CARTESIAN_POINT ( 'NONE',  ( 20.08610463437157279, 63.30000000000001137, -27.64615127144129758 ) ) ;
#15406 = CARTESIAN_POINT ( 'NONE',  ( -1.756012107511856980E-14, 4.499999999999997335, -24.50000000000000000 ) ) ;
#15407 = CYLINDRICAL_SURFACE ( 'NONE', #1684, 24.50000000000000000 ) ;
#15408 = VECTOR ( 'NONE', #3212, 1000.000000000000000 ) ;
#15409 = CARTESIAN_POINT ( 'NONE',  ( 28.01184896238304134, 13.43229166666666607, 7.505752307972846538 ) ) ;
#15410 = CARTESIAN_POINT ( 'NONE',  ( -10.04305231718579172, 32.10000000546236976, -30.90933677959248982 ) ) ;
#15411 = CARTESIAN_POINT ( 'NONE',  ( 15.01150461594596486, 36.77864583333332860, -26.00068869287367690 ) ) ;
#15412 = SHAPE_DEFINITION_REPRESENTATION ( #8539, #8075 ) ;
#15413 = DIRECTION ( 'NONE',  ( 0.000000000000000000, 0.000000000000000000, 1.000000000000000000 ) ) ;
#15414 = CARTESIAN_POINT ( 'NONE',  ( 23.41746825000000243, 17.22499999726880304, -7.608796670333727974 ) ) ;
#15415 = CARTESIAN_POINT ( 'NONE',  ( 10.04305231718578817, 11.39999999999999325, -30.90933677959249337 ) ) ;
#15416 = CARTESIAN_POINT ( 'NONE',  ( -12.13525491562421088, 73.80000000000001137, -8.816778784387096835 ) ) ;
#15417 = CARTESIAN_POINT ( 'NONE',  ( 27.95245687107223276, 56.53868083240936215, -0.04044903255042905932 ) ) ;
#15418 = CARTESIAN_POINT ( 'NONE',  ( 33.58253175000000113, 52.12500000273118417, -4.112674001490185761E-15 ) ) ;
#15419 = CARTESIAN_POINT ( 'NONE',  ( 27.16883889988624290, 60.17500000273119554, 19.73931689729373673 ) ) ;
#15420 = CARTESIAN_POINT ( 'NONE',  ( -33.58253175000000113, 39.47500000273117848, 10.91162601494193929 ) ) ;
#15421 = CARTESIAN_POINT ( 'NONE',  ( 6.001560367445586717E-15, 1.500000000000005995, 24.50000000000000000 ) ) ;
#15422 = CARTESIAN_POINT ( 'NONE',  ( 19.09188309203661049, 16.29687499999999645, -19.09188309203694445 ) ) ;
#15423 = CARTESIAN_POINT ( 'NONE',  ( -20.08610463437156923, 62.29999999999998295, 27.64615127144130113 ) ) ;
#15424 = CARTESIAN_POINT ( 'NONE',  ( -26.29305231718579350, 22.30000000546239391, -19.10302069950537884 ) ) ;
#15425 = DIRECTION ( 'NONE',  ( -1.224646799147353454E-16, 1.000000000000000000, -0.000000000000000000 ) ) ;
#15426 = CARTESIAN_POINT ( 'NONE',  ( -2.162160676586881955E-15, 12.62500000273118772, -35.31076352940723240 ) ) ;
#15427 = FACE_BOUND ( 'NONE', #30055, .T. ) ;
#15428 = CYLINDRICAL_SURFACE ( 'NONE', #27046, 24.50000000000000000 ) ;
#15429 = CARTESIAN_POINT ( 'NONE',  ( 23.41746824999999887, 1.124999997268810725, 0.000000000000000000 ) ) ;
#15430 = CARTESIAN_POINT ( 'NONE',  ( 7.025853678916867295, 16.00482666574268720, 26.06988505166722803 ) ) ;
#15431 = CARTESIAN_POINT ( 'NONE',  ( -2.092463501923844636E-15, 34.00000000546236123, -34.17252228774368916 ) ) ;
#15432 = CARTESIAN_POINT ( 'NONE',  ( 7.890940483122900408E-14, 18.24999999453761745, -24.50000000000000000 ) ) ;
#15433 = CARTESIAN_POINT ( 'NONE',  ( 6.486482029760648627E-15, 23.62500000273119127, 35.31076352940722529 ) ) ;
#15434 = VECTOR ( 'NONE', #29433, 1000.000000000000000 ) ;
#15435 = CARTESIAN_POINT ( 'NONE',  ( 13.97622843553589966, 43.65364583333332860, -24.20753774853756113 ) ) ;
#15436 = ORIENTED_EDGE ( 'NONE', *, *, #27277, .F. ) ;
#15437 = CARTESIAN_POINT ( 'NONE',  ( -10.37757302488624411, 62.72500000273119269, -31.93888565452638417 ) ) ;
#15438 = CARTESIAN_POINT ( 'NONE',  ( -26.00068869287340334, 49.09635416666665719, 15.01150461594643382 ) ) ;
#15439 = ORIENTED_EDGE ( 'NONE', *, *, #27464, .T. ) ;
#15440 = CARTESIAN_POINT ( 'NONE',  ( 28.00173670424549499, 62.99517333425730214, 7.543491769121417612 ) ) ;
#15441 = CARTESIAN_POINT ( 'NONE',  ( 24.18731323226247554, 59.70090250092397355, 14.01125832528285997 ) ) ;
#15442 = ORIENTED_EDGE ( 'NONE', *, *, #31693, .F. ) ;
#15443 = CARTESIAN_POINT ( 'NONE',  ( 10.37757302488624767, 13.72500000273117671, 31.93888565452638417 ) ) ;
#15444 = CARTESIAN_POINT ( 'NONE',  ( -30.02300923189239512, 66.57031250000000000, 2.654126918244515359E-13 ) ) ;
#15445 = DIRECTION ( 'NONE',  ( 0.000000000000000000, -0.000000000000000000, -1.000000000000000000 ) ) ;
#15446 = CARTESIAN_POINT ( 'NONE',  ( 20.75514604977248467, 36.67500000273118843, -28.56700777964554305 ) ) ;
#15447 = CARTESIAN_POINT ( 'NONE',  ( -32.50000000000000000, 38.40000000546235981, -10.55989012756945478 ) ) ;
#15448 = CARTESIAN_POINT ( 'NONE',  ( 4.635254915624212657, 76.59999999999999432, 14.26584774442730286 ) ) ;
#15449 = CARTESIAN_POINT ( 'NONE',  ( -32.50000000000000000, 48.09999999999998721, 10.55989012756946366 ) ) ;
#15450 = CARTESIAN_POINT ( 'NONE',  ( -33.58253175000000113, 25.22500000273119625, 10.91162601494193929 ) ) ;
#15451 = CARTESIAN_POINT ( 'NONE',  ( 8.891200544363830713E-16, 79.75000000546236834, -15.00000000000000000 ) ) ;
#15452 = CARTESIAN_POINT ( 'NONE',  ( -33.58253175000000113, 51.27500000273118275, -10.91162601494193218 ) ) ;
#15453 = EDGE_CURVE ( 'NONE', #9893, #19228, #18334, .T. ) ;
#15454 = CARTESIAN_POINT ( 'NONE',  ( 6.277390505771533514E-15, 30.49999999999999645, 34.17252228774368916 ) ) ;
#15455 = CARTESIAN_POINT ( 'NONE',  ( -32.50000000000000000, 28.10000000000001208, 10.55989012756946366 ) ) ;
#15456 = CARTESIAN_POINT ( 'NONE',  ( 24.50000000000000355, 7.900000000000012790, 7.960532557706212486 ) ) ;
#15457 = CARTESIAN_POINT ( 'NONE',  ( 20.75514604977249178, 67.82500000273120122, 28.56700777964553950 ) ) ;
#15458 = CARTESIAN_POINT ( 'NONE',  ( -26.29305231718578995, 78.19999999999998863, 19.10302069950538595 ) ) ;
#15459 = AXIS2_PLACEMENT_3D ( 'NONE', #19823, #33013, #27212 ) ;
#15460 = CARTESIAN_POINT ( 'NONE',  ( -10.04305231718578462, 38.39999999999999147, 30.90933677959249337 ) ) ;
#15461 = CARTESIAN_POINT ( 'NONE',  ( 27.16883889988624290, 62.17500000273118133, 19.73931689729373673 ) ) ;
#15462 = ADVANCED_FACE ( 'NONE', ( #13167 ), #23645, .F. ) ;
#15463 = EDGE_CURVE ( 'NONE', #21102, #2430, #1952, .T. ) ;
#15464 = CARTESIAN_POINT ( 'NONE',  ( 32.50000000000000000, 39.60000000546235555, -10.55989012756945833 ) ) ;
#15465 = CARTESIAN_POINT ( 'NONE',  ( 33.58253175000000823, 14.02500000273117209, 10.91162601494192863 ) ) ;
#15466 = CARTESIAN_POINT ( 'NONE',  ( -19.11951029504763611, 26.32850666759063785, 19.06425588902592239 ) ) ;
#15467 = CARTESIAN_POINT ( 'NONE',  ( 29.12397828776036235, 66.99999999999997158, -15.02363756889424273 ) ) ;
#15468 = CARTESIAN_POINT ( 'NONE',  ( 10.37757302488624056, 36.52500000273118985, -31.93888565452638417 ) ) ;
#15469 = PLANE ( 'NONE',  #20990 ) ;
#15470 = FACE_OUTER_BOUND ( 'NONE', #16883, .T. ) ;
#15471 = ADVANCED_FACE ( 'NONE', ( #29448 ), #3216, .F. ) ;
#15472 = CARTESIAN_POINT ( 'NONE',  ( -8.960552108402744065E-16, 74.37500000273121259, -14.63369212191046209 ) ) ;
#15473 = CARTESIAN_POINT ( 'NONE',  ( 14.97647472619900455, 49.09076416574269786, -26.02091320914876960 ) ) ;
#15474 = CARTESIAN_POINT ( 'NONE',  ( -10.04305231718579172, 58.10000000546237686, -30.90933677959248982 ) ) ;
#15475 = CARTESIAN_POINT ( 'NONE',  ( -13.91746824999999532, 75.27500000273118985, -4.522059556121115875 ) ) ;
#15476 = PRESENTATION_STYLE_ASSIGNMENT (( #19639 ) ) ;
#15477 = CARTESIAN_POINT ( 'NONE',  ( -19.11951029504797006, 65.56211833240934084, -19.06425588902558133 ) ) ;
#15478 = CARTESIAN_POINT ( 'NONE',  ( 10.04305231718578817, 63.90000000546236691, -30.90933677959249337 ) ) ;
#15479 = CARTESIAN_POINT ( 'NONE',  ( 32.50000000000000711, 73.40000000546234560, 10.55989012756945122 ) ) ;
#15480 = CARTESIAN_POINT ( 'NONE',  ( -7.505752307973343918, 22.59895833333332860, -28.01184896238290989 ) ) ;
#15481 = CARTESIAN_POINT ( 'NONE',  ( 10.37757302488624056, 34.77500000273118985, -31.93888565452638417 ) ) ;
#15482 = CARTESIAN_POINT ( 'NONE',  ( -4.523095164977117273E-15, 6.624999997268815832, 24.62258325217400312 ) ) ;
#15483 = ORIENTED_EDGE ( 'NONE', *, *, #32495, .F. ) ;
#15484 = CARTESIAN_POINT ( 'NONE',  ( -33.58253175000000113, 73.37500000273116996, 0.000000000000000000 ) ) ;
#15485 = CARTESIAN_POINT ( 'NONE',  ( 26.29305231718579350, 25.30000000546238326, 19.10302069950537529 ) ) ;
#15486 = CARTESIAN_POINT ( 'NONE',  ( -26.00068869287368756, 42.79427083333331439, -15.01150461594595775 ) ) ;
#15487 = CARTESIAN_POINT ( 'NONE',  ( 20.50609665440969565, 60.98437499999999289, -20.50609665441004736 ) ) ;
#15488 = CARTESIAN_POINT ( 'NONE',  ( -33.58253175000000113, 55.27500000273120406, -10.91162601494193218 ) ) ;
#15489 = CARTESIAN_POINT ( 'NONE',  ( 20.08610463437158344, 55.20000000546238539, 27.64615127144129403 ) ) ;
#15490 = DIRECTION ( 'NONE',  ( 1.000000000000000000, 0.000000000000000000, 1.224646799147352714E-16 ) ) ;
#15491 = CARTESIAN_POINT ( 'NONE',  ( -33.58253175000000113, 41.12500000273119838, 0.000000000000000000 ) ) ;
#15492 = CARTESIAN_POINT ( 'NONE',  ( -9.270509831248419985, 72.30000000000001137, 12.75976212528060039 ) ) ;
#15493 = CARTESIAN_POINT ( 'NONE',  ( -33.58253175000000113, 67.47500000273117848, 10.91162601494193929 ) ) ;
#15494 = CARTESIAN_POINT ( 'NONE',  ( 10.04305231718579705, 5.100000005462374197, 30.90933677959248982 ) ) ;
#15495 = CARTESIAN_POINT ( 'NONE',  ( -27.16883889988623935, 61.32500000273120833, 19.73931689729374739 ) ) ;
#15496 = CARTESIAN_POINT ( 'NONE',  ( 18.94512977948575738, 18.92499999726882010, 13.76444248337723408 ) ) ;
#15497 = CARTESIAN_POINT ( 'NONE',  ( -20.08610463437156923, 46.29999999999999716, 27.64615127144130113 ) ) ;
#15498 = CARTESIAN_POINT ( 'NONE',  ( 1.507698388325705758E-15, 1.124999997268814722, -24.62258325217400312 ) ) ;
#15499 = CARTESIAN_POINT ( 'NONE',  ( 27.16883889988624290, 10.17500000273119376, 19.73931689729373673 ) ) ;
#15500 = VECTOR ( 'NONE', #17315, 1000.000000000000000 ) ;
#15501 = LINE ( 'NONE', #33329, #5256 ) ;
#15502 = CARTESIAN_POINT ( 'NONE',  ( -7.025853678916861966, 34.91107666574267654, -26.06988505166722803 ) ) ;
#15503 = CARTESIAN_POINT ( 'NONE',  ( -4.300734207923755825, 71.27500000273117564, 13.23629886949340673 ) ) ;
#15504 = CARTESIAN_POINT ( 'NONE',  ( -27.16883889988624290, 79.17500000273119554, -19.73931689729374028 ) ) ;
#15505 = FACE_OUTER_BOUND ( 'NONE', #12854, .T. ) ;
#15506 =( BOUNDED_CURVE ( )  B_SPLINE_CURVE ( 2, ( #4364, #25127, #16908, #22387, #24955, #32836, #17245 ),
 .UNSPECIFIED., .F., .T. ) 
 B_SPLINE_CURVE_WITH_KNOTS ( ( 3, 2, 2, 3 ),
 ( 0.7500000000000000000, 0.7600000000000001199, 0.7800000000000004707, 0.8000000000000007105 ),
 .UNSPECIFIED. ) 
 CURVE ( )  GEOMETRIC_REPRESENTATION_ITEM ( )  RATIONAL_B_SPLINE_CURVE ( ( 0.9755282581475768211, 0.9755282581475768211, 1.000000000000000000, 0.9510565162951535312, 1.000000000000000000, 0.9510565162951518658, 1.000000000000001554 ) ) 
 REPRESENTATION_ITEM ( '' )  );
#15507 = AXIS2_PLACEMENT_3D ( 'NONE', #4366, #12436, #22906 ) ;
#15508 = CARTESIAN_POINT ( 'NONE',  ( -20.75514604977248823, 77.07500000273117280, -28.56700777964554305 ) ) ;
#15509 = ORIENTED_EDGE ( 'NONE', *, *, #7163, .F. ) ;
#15510 = CARTESIAN_POINT ( 'NONE',  ( 23.41746825000000243, 15.22499999726880482, -7.608796670333727974 ) ) ;
#15511 = CARTESIAN_POINT ( 'NONE',  ( -4.523095164977117273E-15, 2.124999997268811835, 24.62258325217400312 ) ) ;
#15512 = CARTESIAN_POINT ( 'NONE',  ( 24.20753774853756113, 58.26302083333332149, 13.97622843553589789 ) ) ;
#15513 =( BOUNDED_CURVE ( )  B_SPLINE_CURVE ( 2, ( #17549, #6561, #11704, #12041, #22187, #4494, #29892, #32963, #27839, #30056, #14970, #4323, #17036 ),
 .UNSPECIFIED., .F., .T. ) 
 B_SPLINE_CURVE_WITH_KNOTS ( ( 3, 2, 2, 2, 2, 2, 3 ),
 ( 0.3012820512820512664, 0.3025641025641025439, 0.3051282051282051544, 0.3076923076923077094, 0.3102564102564102644, 0.3128205128205128194, 0.3141025641025640969 ),
 .UNSPECIFIED. ) 
 CURVE ( )  GEOMETRIC_REPRESENTATION_ITEM ( )  RATIONAL_B_SPLINE_CURVE ( ( 0.9755282581475768211, 0.9755282581475768211, 1.000000000000000000, 0.9510565162951535312, 1.000000000000000000, 0.9510565162951535312, 1.000000000000000000, 0.9510565162951535312, 1.000000000000000000, 0.9510565162951535312, 1.000000000000000000, 0.9755282581475768211, 0.9755282581475768211 ) ) 
 REPRESENTATION_ITEM ( '' )  );
#15514 = CARTESIAN_POINT ( 'NONE',  ( 27.16883889988624290, 55.92500000273119554, 19.73931689729373673 ) ) ;
#15515 = CARTESIAN_POINT ( 'NONE',  ( -27.16883889988624290, 19.17500000273118843, -19.73931689729374028 ) ) ;
#15516 = CARTESIAN_POINT ( 'NONE',  ( -20.75514604977248823, 7.075000002731188786, -28.56700777964554305 ) ) ;
#15517 = CARTESIAN_POINT ( 'NONE',  ( 19.09188309203694800, 44.65624999999999289, 19.09188309203660694 ) ) ;
#15518 = CARTESIAN_POINT ( 'NONE',  ( -26.02091320914849959, 19.59673583425730925, 14.97647472619947528 ) ) ;
#15519 = CARTESIAN_POINT ( 'NONE',  ( 14.97647472619900455, 21.59076416574269430, -26.02091320914876960 ) ) ;
#15520 = CARTESIAN_POINT ( 'NONE',  ( -20.75514604977248112, 3.425000002731186655, 28.56700777964554661 ) ) ;
#15521 = ADVANCED_FACE ( 'NONE', ( #14012 ), #11429, .T. ) ;
#15522 = FACE_OUTER_BOUND ( 'NONE', #13629, .T. ) ;
#15523 = CARTESIAN_POINT ( 'NONE',  ( 33.58253175000000113, 44.12500000273117706, -4.112674001490185761E-15 ) ) ;
#15524 = CARTESIAN_POINT ( 'NONE',  ( -23.41746824999999887, 9.624999997268817609, -2.867812753649727150E-15 ) ) ;
#15525 = CARTESIAN_POINT ( 'NONE',  ( 9.270509831248425314, 78.69999999999998863, 12.75976212528059683 ) ) ;
#15526 = VERTEX_POINT ( 'NONE', #32518 ) ;
#15527 = CARTESIAN_POINT ( 'NONE',  ( -33.58253175000000113, 55.37500000273119838, 0.000000000000000000 ) ) ;
#15528 = CARTESIAN_POINT ( 'NONE',  ( 10.04305231718579705, 59.10000000546237686, 30.90933677959248982 ) ) ;
#15529 = CARTESIAN_POINT ( 'NONE',  ( -14.01125832528285109, 46.81027750092398776, 24.18731323226248264 ) ) ;
#15530 = CARTESIAN_POINT ( 'NONE',  ( 6.486482029760649416E-15, 73.87500000273119838, 35.31076352940723240 ) ) ;
#15531 = EDGE_LOOP ( 'NONE', ( #9126, #25896 ) ) ;
#15532 = CARTESIAN_POINT ( 'NONE',  ( 6.486482029760649416E-15, 25.62500000273118772, 35.31076352940723240 ) ) ;
#15533 = CIRCLE ( 'NONE', #33028, 9.000000000000001776 ) ;
#15534 = CARTESIAN_POINT ( 'NONE',  ( -7.505752307972844761, 17.72916666666666430, 28.01184896238304134 ) ) ;
#15535 = ORIENTED_EDGE ( 'NONE', *, *, #24657, .T. ) ;
#15536 = CARTESIAN_POINT ( 'NONE',  ( -10.04305231718579172, 57.60000000000000142, -30.90933677959248982 ) ) ;
#15537 = CARTESIAN_POINT ( 'NONE',  ( -33.58253175000000113, 63.02500000273118985, -10.91162601494193218 ) ) ;
#15538 = CARTESIAN_POINT ( 'NONE',  ( -15.01150461594595775, 38.49739583333332860, 26.00068869287368756 ) ) ;
#15539 = CARTESIAN_POINT ( 'NONE',  ( 7.570916362186207671, 17.60000000000000497, 23.30088464923126779 ) ) ;
#15540 = CARTESIAN_POINT ( 'NONE',  ( 1.507698388325705758E-15, 5.624999997268818497, -24.62258325217400312 ) ) ;
#15541 = CARTESIAN_POINT ( 'NONE',  ( 27.16883889988623935, 4.325000002731171911, -19.73931689729374384 ) ) ;
#15542 = CARTESIAN_POINT ( 'NONE',  ( -19.82091636218621034, 6.549999994537619941, -14.40073868116559552 ) ) ;
#15543 = CARTESIAN_POINT ( 'NONE',  ( 25.98046417659831775, 66.56472249907604066, -15.04653450569338879 ) ) ;
#15544 = CARTESIAN_POINT ( 'NONE',  ( -2.162160676586881955E-15, 78.87500000273118417, -35.31076352940723240 ) ) ;
#15545 = CARTESIAN_POINT ( 'NONE',  ( -28.01184896238290278, 62.98958333333332149, 7.505752307973363457 ) ) ;
#15546 = CARTESIAN_POINT ( 'NONE',  ( -32.50000000000000000, 70.00000000000000000, 0.000000000000000000 ) ) ;
#15547 = CARTESIAN_POINT ( 'NONE',  ( 6.277390505771533514E-15, 18.49999999999999645, 34.17252228774368916 ) ) ;
#15548 = CARTESIAN_POINT ( 'NONE',  ( 2.584737979205442066E-13, 62.27343749999999289, 27.95245687107223276 ) ) ;
#15549 = CARTESIAN_POINT ( 'NONE',  ( 19.82091636218621389, 13.94999999453763806, -14.40073868116559197 ) ) ;
#15550 = CARTESIAN_POINT ( 'NONE',  ( -4.300734207923759378, 80.47500000273119269, -13.23629886949340495 ) ) ;
#15551 = CARTESIAN_POINT ( 'NONE',  ( -26.07999730980477437, 21.73958333333332860, 6.988114217768305103 ) ) ;
#15552 = CARTESIAN_POINT ( 'NONE',  ( -33.58253175000000113, 33.02500000273118275, -10.91162601494193218 ) ) ;
#15553 = CYLINDRICAL_SURFACE ( 'NONE', #29201, 32.50000000000000000 ) ;
#15554 = CARTESIAN_POINT ( 'NONE',  ( 20.75514604977248467, 36.67500000273118843, -28.56700777964554305 ) ) ;
#15555 = CARTESIAN_POINT ( 'NONE',  ( 27.16883889988623935, 20.57500000273118701, -19.73931689729374384 ) ) ;
#15556 = CARTESIAN_POINT ( 'NONE',  ( -9.270509831248419985, 80.29999999999999716, 12.75976212528060039 ) ) ;
#15557 = CARTESIAN_POINT ( 'NONE',  ( -26.06988505166735237, 44.08892333425729504, -7.025853678916388567 ) ) ;
#15558 = AXIS2_PLACEMENT_3D ( 'NONE', #24692, #8400, #3764 ) ;
#15559 = CARTESIAN_POINT ( 'NONE',  ( -33.58253175000000113, 77.22500000273117848, 10.91162601494193929 ) ) ;
#15560 = FACE_OUTER_BOUND ( 'NONE', #27327, .T. ) ;
#15561 = EDGE_CURVE ( 'NONE', #32793, #29266, #31126, .T. ) ;
#15562 = CARTESIAN_POINT ( 'NONE',  ( -26.29305231718578995, 60.20000000000001705, 19.10302069950538595 ) ) ;
#15563 = CARTESIAN_POINT ( 'NONE',  ( -14.47279130897152299, 17.92499999726880588, 19.92008829642072243 ) ) ;
#15564 = CARTESIAN_POINT ( 'NONE',  ( -10.37757302488624411, 62.72500000273117848, -31.93888565452638417 ) ) ;
#15565 = EDGE_CURVE ( 'NONE', #9328, #30741, #12274, .T. ) ;
#15566 = CARTESIAN_POINT ( 'NONE',  ( -7.236395654485757944, 11.72499999726880837, -22.27133577429736988 ) ) ;
#15567 = CARTESIAN_POINT ( 'NONE',  ( 33.58253175000000113, 76.47500000273117848, -10.91162601494193751 ) ) ;
#15568 = CARTESIAN_POINT ( 'NONE',  ( 33.58253175000000113, 6.125000002731195714, -4.112674001490185761E-15 ) ) ;
#15569 = CARTESIAN_POINT ( 'NONE',  ( 23.41746825000000243, 17.02499999726880731, 7.608796670333735079 ) ) ;
#15570 = CARTESIAN_POINT ( 'NONE',  ( -14.01125832528285109, 15.87277750092397710, 24.18731323226248264 ) ) ;
#15571 = EDGE_LOOP ( 'NONE', ( #19191, #30348, #32545, #25609, #18819, #16074, #5808, #31446, #14166, #19030, #29304, #16416, #13667, #13259, #25562, #29227, #16207, #18951, #28219, #19477, #29054, #28932 ) ) ;
#15572 = CARTESIAN_POINT ( 'NONE',  ( 33.58253175000000113, 46.22500000273119269, -10.91162601494193751 ) ) ;
#15573 = ORIENTED_EDGE ( 'NONE', *, *, #29737, .T. ) ;
#15574 = CARTESIAN_POINT ( 'NONE',  ( -20.50609665440969209, 42.07812499999999289, 20.50609665441005092 ) ) ;
#15575 = CARTESIAN_POINT ( 'NONE',  ( 1.806199397676865774E-16, -24.47487373415291145, 0.000000000000000000 ) ) ;
#15576 = CARTESIAN_POINT ( 'NONE',  ( -10.04305231718579172, 4.100000005462373309, -30.90933677959248982 ) ) ;
#15577 = CARTESIAN_POINT ( 'NONE',  ( -1.778240108872766143E-15, 28.00000000546237544, -32.49999999999999289 ) ) ;
#15578 = CLOSED_SHELL ( 'NONE', ( #32109, #6837, #23925, #5470, #24466, #5671, #27938, #30632, #17060, #30265, #33106, #31078, #3485, #7471, #1463, #15521, #11588, #28510, #2681, #328, #19539, #11135, #20714, #3564, #22864, #19843, #11415, #13418 ) ) ;
#15579 = CARTESIAN_POINT ( 'NONE',  ( 14.47279130897151767, 5.424999997268823648, -19.92008829642072598 ) ) ;
#15580 = AXIS2_PLACEMENT_3D ( 'NONE', #28, #2627, #3132 ) ;
#15581 = CARTESIAN_POINT ( 'NONE',  ( -18.94512977948575738, 17.42499999726882010, -13.76444248337723231 ) ) ;
#15582 = CARTESIAN_POINT ( 'NONE',  ( 10.37757302488624056, 18.77500000273118985, -31.93888565452638417 ) ) ;
#15583 = CARTESIAN_POINT ( 'NONE',  ( -32.50000000000000000, 64.10000000000000853, 10.55989012756946366 ) ) ;
#15584 = DIRECTION ( 'NONE',  ( -1.000000000000000000, 0.000000000000000000, 0.000000000000000000 ) ) ;
#15585 = CARTESIAN_POINT ( 'NONE',  ( 0.000000000000000000, 0.000000000000000000, 0.000000000000000000 ) ) ;
#15586 = CARTESIAN_POINT ( 'NONE',  ( 7.505752307972854531, 16.01041666666666075, -28.01184896238303423 ) ) ;
#15587 = CARTESIAN_POINT ( 'NONE',  ( 13.91746824999999887, 76.37500000273116996, -1.704398294459741270E-15 ) ) ;
#15588 = CARTESIAN_POINT ( 'NONE',  ( -28.01184896238304134, 42.65104166666666430, -7.505752307972844761 ) ) ;
#15589 = CYLINDRICAL_SURFACE ( 'NONE', #5097, 15.00000000000000000 ) ;
#15590 = CARTESIAN_POINT ( 'NONE',  ( 18.94512977948575738, 18.92499999726882010, 13.76444248337723408 ) ) ;
#15591 = CARTESIAN_POINT ( 'NONE',  ( 10.04305231718578817, 5.400000000000016342, -30.90933677959249337 ) ) ;
#15592 = CARTESIAN_POINT ( 'NONE',  ( -3.712076227271900841E-14, 8.499999999999994671, -24.50000000000000000 ) ) ;
#15593 = CARTESIAN_POINT ( 'NONE',  ( 19.11951029504797006, 53.53086833240935505, 19.06425588902558133 ) ) ;
#15594 = CARTESIAN_POINT ( 'NONE',  ( -10.37757302488623701, 51.52500000273118985, 31.93888565452638417 ) ) ;
#15595 = CARTESIAN_POINT ( 'NONE',  ( 33.58253175000000113, 58.47500000273118559, -10.91162601494193751 ) ) ;
#15596 = CARTESIAN_POINT ( 'NONE',  ( -27.16883889988623935, 43.57500000273117990, 19.73931689729374739 ) ) ;
#15597 = DIRECTION ( 'NONE',  ( -0.000000000000000000, 1.000000000000000000, -0.000000000000000000 ) ) ;
#15598 = CARTESIAN_POINT ( 'NONE',  ( -19.09188309203694445, 11.99999999999999645, -19.09188309203661049 ) ) ;
#15599 = CARTESIAN_POINT ( 'NONE',  ( 4.023268246324634798E-14, 8.499999999999992895, -24.50000000000000355 ) ) ;
#15600 = CARTESIAN_POINT ( 'NONE',  ( 26.29305231718579350, 51.30000000546236549, 19.10302069950537529 ) ) ;
#15601 = CARTESIAN_POINT ( 'NONE',  ( 6.277390505771533514E-15, 78.49999999999998579, 34.17252228774368916 ) ) ;
#15602 = CARTESIAN_POINT ( 'NONE',  ( -33.58253175000000113, 13.02500000273118985, -10.91162601494193218 ) ) ;
#15603 = FACE_OUTER_BOUND ( 'NONE', #16532, .T. ) ;
#15604 = CARTESIAN_POINT ( 'NONE',  ( -24.50000000000000000, 12.74999999453763166, -3.000384657911015469E-15 ) ) ;
#15605 = CARTESIAN_POINT ( 'NONE',  ( 24.50000000000000000, 11.90000000000000213, 7.960532557706212486 ) ) ;
#15606 = CARTESIAN_POINT ( 'NONE',  ( -24.18731323226221974, 16.72097249907602290, 14.01125832528330406 ) ) ;
#15607 = EDGE_CURVE ( 'NONE', #16123, #26574, #13393, .T. ) ;
#15608 = CARTESIAN_POINT ( 'NONE',  ( 20.08610463437157279, 35.80000000546235128, -27.64615127144129758 ) ) ;
#15609 = EDGE_CURVE ( 'NONE', #23625, #22018, #12433, .T. ) ;
#15610 =( BOUNDED_CURVE ( )  B_SPLINE_CURVE ( 2, ( #25151, #6957, #17100, #20186, #12105, #6789, #25501, #22576, #1462, #4385, #11940, #9532, #27558 ),
 .UNSPECIFIED., .F., .F. ) 
 B_SPLINE_CURVE_WITH_KNOTS ( ( 3, 2, 2, 2, 2, 2, 3 ),
 ( 0.4935897435897436125, 0.4948717948717948900, 0.4974358974358974450, 0.5000000000000000000, 0.5025641025641025550, 0.5051282051282051100, 0.5064102564102563875 ),
 .UNSPECIFIED. ) 
 CURVE ( )  GEOMETRIC_REPRESENTATION_ITEM ( )  RATIONAL_B_SPLINE_CURVE ( ( 0.9755282581475768211, 0.9755282581475768211, 1.000000000000000000, 0.9510565162951535312, 1.000000000000000000, 0.9510565162951535312, 1.000000000000000000, 0.9510565162951535312, 1.000000000000000000, 0.9510565162951535312, 1.000000000000000000, 0.9755282581475768211, 0.9755282581475768211 ) ) 
 REPRESENTATION_ITEM ( '' )  );
#15611 = CARTESIAN_POINT ( 'NONE',  ( -19.82091636218621034, 10.54999999453762349, -14.40073868116559552 ) ) ;
#15612 = CARTESIAN_POINT ( 'NONE',  ( -10.37757302488624411, 28.72500000273120335, -31.93888565452638417 ) ) ;
#15613 = CARTESIAN_POINT ( 'NONE',  ( -6.988114217767819270, 45.22916666666665719, 26.07999730980490583 ) ) ;
#15614 = VERTEX_POINT ( 'NONE', #30279 ) ;
#15615 = CARTESIAN_POINT ( 'NONE',  ( -33.58253175000000113, 65.12500000273118417, 0.000000000000000000 ) ) ;
#15616 = CARTESIAN_POINT ( 'NONE',  ( -26.00068869287368756, 46.23177083333331439, -15.01150461594595775 ) ) ;
#15617 = ORIENTED_EDGE ( 'NONE', *, *, #9950, .F. ) ;
#15618 = CARTESIAN_POINT ( 'NONE',  ( 26.00068869287367335, 17.01302083333332504, 15.01150461594596308 ) ) ;
#15619 = CARTESIAN_POINT ( 'NONE',  ( -20.53372385742071771, 12.57850666759064140, 20.47846945139902530 ) ) ;
#15620 = CARTESIAN_POINT ( 'NONE',  ( 27.16883889988623935, 6.325000002731187898, -19.73931689729374384 ) ) ;
#15621 = FACE_OUTER_BOUND ( 'NONE', #7960, .T. ) ;
#15622 = CARTESIAN_POINT ( 'NONE',  ( -27.16883889988623935, 33.57500000273120122, 19.73931689729374739 ) ) ;
#15623 = AXIS2_PLACEMENT_3D ( 'NONE', #15237, #30322, #33237 ) ;
#15624 = CARTESIAN_POINT ( 'NONE',  ( 6.277390505771533514E-15, 37.00000000546237544, 34.17252228774368916 ) ) ;
#15625 = EDGE_CURVE ( 'NONE', #3936, #30562, #13793, .T. ) ;
#15626 = CARTESIAN_POINT ( 'NONE',  ( 9.270509831248425314, 78.70000000000003126, 12.75976212528059683 ) ) ;
#15627 = CARTESIAN_POINT ( 'NONE',  ( -28.01184896238304134, 63.27604166666667140, -7.505752307972844761 ) ) ;
#15628 = CARTESIAN_POINT ( 'NONE',  ( 27.16883889988623935, 20.32500000273118701, -19.73931689729374384 ) ) ;
#15629 = CARTESIAN_POINT ( 'NONE',  ( 0.000000000000000000, 0.000000000000000000, 26.50000000000000355 ) ) ;
#15630 = CARTESIAN_POINT ( 'NONE',  ( -27.16883889988623935, 47.57500000273117990, 19.73931689729374739 ) ) ;
#15631 = CARTESIAN_POINT ( 'NONE',  ( 20.08610463437157279, 29.30000000000000782, -27.64615127144129758 ) ) ;
#15632 = CARTESIAN_POINT ( 'NONE',  ( -20.08610463437157989, 27.69999999999999929, -27.64615127144129758 ) ) ;
#15633 = CARTESIAN_POINT ( 'NONE',  ( -24.50000000000001066, 3.099999999999989875, 7.960532557706201828 ) ) ;
#15634 = CARTESIAN_POINT ( 'NONE',  ( -10.37757302488623701, 69.52500000273120406, 31.93888565452638417 ) ) ;
#15635 = CARTESIAN_POINT ( 'NONE',  ( -32.61426705943295445, 67.00000000000001421, -7.648559219945903820 ) ) ;
#15636 = CARTESIAN_POINT ( 'NONE',  ( 12.41655794490159082, 74.00000000000001421, -6.419367199009562874 ) ) ;
#15637 = CARTESIAN_POINT ( 'NONE',  ( -27.16883889988623935, 57.57500000273119412, 19.73931689729374739 ) ) ;
#15638 = FACE_OUTER_BOUND ( 'NONE', #18058, .T. ) ;
#15639 = CARTESIAN_POINT ( 'NONE',  ( -2.162160676586881955E-15, 14.62500000273118239, -35.31076352940723240 ) ) ;
#15640 = CARTESIAN_POINT ( 'NONE',  ( 24.18731323226247554, 32.20090250092397355, 14.01125832528285997 ) ) ;
#15641 = CARTESIAN_POINT ( 'NONE',  ( 12.18942006770534547, 66.99999999999997158, -30.86762708970427127 ) ) ;
#15642 = CARTESIAN_POINT ( 'NONE',  ( -20.75514604977248112, 1.675000002731184212, 28.56700777964554661 ) ) ;
#15643 = CARTESIAN_POINT ( 'NONE',  ( -2.162160676586881955E-15, 36.62500000273119127, -35.31076352940723240 ) ) ;
#15644 = CARTESIAN_POINT ( 'NONE',  ( 10.04305231718579705, 45.10000000546238397, 30.90933677959248982 ) ) ;
#15645 = LINE ( 'NONE', #25923, #16647 ) ;
#15646 = CARTESIAN_POINT ( 'NONE',  ( 13.91746824999999532, 75.97500000273116427, -4.522059556121118540 ) ) ;
#15647 = CARTESIAN_POINT ( 'NONE',  ( -20.47846945139866648, 50.95274333240935505, 20.53372385742108008 ) ) ;
#15648 = CARTESIAN_POINT ( 'NONE',  ( 10.04305231718579705, 53.10000000546237686, 30.90933677959248982 ) ) ;
#15649 = AXIS2_PLACEMENT_3D ( 'NONE', #15045, #4055, #19844 ) ;
#15650 = CARTESIAN_POINT ( 'NONE',  ( -4.300734207923759378, 74.97500000273122112, -13.23629886949340495 ) ) ;
#15651 = FILL_AREA_STYLE ('',( #31415 ) ) ;
#15652 = CARTESIAN_POINT ( 'NONE',  ( 19.09188309203661049, 19.73437500000000000, -19.09188309203694445 ) ) ;
#15653 = FACE_OUTER_BOUND ( 'NONE', #29972, .T. ) ;
#15654 = CARTESIAN_POINT ( 'NONE',  ( -10.04305231718579172, 72.10000000546237686, -30.90933677959248982 ) ) ;
#15655 = CARTESIAN_POINT ( 'NONE',  ( -28.01184896238290278, 18.30208333333332860, 7.505752307973363457 ) ) ;
#15656 = CARTESIAN_POINT ( 'NONE',  ( 10.37757302488624056, 36.77500000273118985, -31.93888565452638417 ) ) ;
#15657 = CARTESIAN_POINT ( 'NONE',  ( 14.47279130897151767, 16.82499999726881157, 19.92008829642072953 ) ) ;
#15658 = ORIENTED_EDGE ( 'NONE', *, *, #32821, .F. ) ;
#15659 = CARTESIAN_POINT ( 'NONE',  ( -28.02196122052045268, 40.36496500092396644, 7.468012846824790607 ) ) ;
#15660 = CARTESIAN_POINT ( 'NONE',  ( 20.08610463437157279, 23.80000000546235839, -27.64615127144129758 ) ) ;
#15661 = EDGE_CURVE ( 'NONE', #10375, #4234, #26321, .T. ) ;
#15662 = CARTESIAN_POINT ( 'NONE',  ( -2.584737979205441561E-13, 39.92968750000000000, -30.02300923189239512 ) ) ;
#15663 = CARTESIAN_POINT ( 'NONE',  ( -15.01150461594642138, 63.70572916666667140, -26.00068869287340334 ) ) ;
#15664 = CARTESIAN_POINT ( 'NONE',  ( 20.75514604977248467, 54.67500000273119554, -28.56700777964554305 ) ) ;
#15665 = CARTESIAN_POINT ( 'NONE',  ( 32.50000000000000000, 55.60000000546238397, -10.55989012756945833 ) ) ;
#15666 = CARTESIAN_POINT ( 'NONE',  ( 1.555960095263670572E-15, 8.249999994537619230, -24.50000000000000000 ) ) ;
#15667 = CARTESIAN_POINT ( 'NONE',  ( -33.58253175000000113, 41.02500000273118985, -10.91162601494193218 ) ) ;
#15668 = FACE_BOUND ( 'NONE', #12189, .T. ) ;
#15669 = CARTESIAN_POINT ( 'NONE',  ( 33.58253175000000113, 70.47500000273117848, -10.91162601494193751 ) ) ;
#15670 = CARTESIAN_POINT ( 'NONE',  ( 32.50000000000000000, 1.600000005462365760, -10.55989012756945833 ) ) ;
#15671 = EDGE_CURVE ( 'NONE', #24911, #25651, #22805, .T. ) ;
#15672 = CARTESIAN_POINT ( 'NONE',  ( 20.75514604977248467, 62.42500000273118133, -28.56700777964554305 ) ) ;
#15673 = CARTESIAN_POINT ( 'NONE',  ( 20.50609665440969565, 19.73437500000000000, -20.50609665441004736 ) ) ;
#15674 =( GEOMETRIC_REPRESENTATION_CONTEXT ( 3 ) GLOBAL_UNCERTAINTY_ASSIGNED_CONTEXT ( ( #23234 ) ) GLOBAL_UNIT_ASSIGNED_CONTEXT ( ( #9258, #1190, #1362 ) ) REPRESENTATION_CONTEXT ( 'NONE', 'WORKASPACE' ) );
#15675 = CARTESIAN_POINT ( 'NONE',  ( 32.50000000000000000, 48.99999999999998579, -3.980102097228898626E-15 ) ) ;
#15676 = CARTESIAN_POINT ( 'NONE',  ( -14.47279130897152122, 3.924999997268813434, 19.92008829642072243 ) ) ;
#15677 = CARTESIAN_POINT ( 'NONE',  ( -10.37757302488623701, 13.77500000273118630, 31.93888565452638417 ) ) ;
#15678 = CARTESIAN_POINT ( 'NONE',  ( -26.09010956794245217, 37.77565999907600514, -6.950374756619243755 ) ) ;
#15679 = CARTESIAN_POINT ( 'NONE',  ( -4.300734207923755825, 79.77500000273118985, 13.23629886949340673 ) ) ;
#15680 = CARTESIAN_POINT ( 'NONE',  ( 12.13525491562421088, 75.05000000546237970, 8.816778784387095058 ) ) ;
#15681 = CYLINDRICAL_SURFACE ( 'NONE', #24812, 32.50000000000000000 ) ;
#15682 = CARTESIAN_POINT ( 'NONE',  ( -27.16883889988624290, 75.17500000273118133, -19.73931689729374028 ) ) ;
#15683 = ORIENTED_EDGE ( 'NONE', *, *, #26732, .T. ) ;
#15684 = CARTESIAN_POINT ( 'NONE',  ( -23.41746825000000598, 18.22499999726882436, 7.608796670333726198 ) ) ;
#15685 = CARTESIAN_POINT ( 'NONE',  ( 6.988114217768294445, 58.69270833333332860, 26.07999730980477437 ) ) ;
#15686 = CONICAL_SURFACE ( 'NONE', #3608, 26.50000000000000000, 1.047197551196594523 ) ;
#15687 = CARTESIAN_POINT ( 'NONE',  ( -33.58253175000000113, 55.12500000273119838, 0.000000000000000000 ) ) ;
#15688 = CARTESIAN_POINT ( 'NONE',  ( -10.37757302488623701, 15.77500000273117386, 31.93888565452638417 ) ) ;
#15689 = CARTESIAN_POINT ( 'NONE',  ( -33.58253175000000113, 3.375000002731193049, 0.000000000000000000 ) ) ;
#15690 = CARTESIAN_POINT ( 'NONE',  ( 24.20753774853756113, 41.07552083333332149, 13.97622843553589789 ) ) ;
#15691 = CARTESIAN_POINT ( 'NONE',  ( -7.543491769121417612, 29.47954833425730570, 28.00173670424549499 ) ) ;
#15692 = CARTESIAN_POINT ( 'NONE',  ( 25.98046417659831775, 18.43972249907602290, -15.04653450569338879 ) ) ;
#15693 = CARTESIAN_POINT ( 'NONE',  ( -20.08610463437156923, 74.80000000546239391, 27.64615127144130113 ) ) ;
#15694 = CARTESIAN_POINT ( 'NONE',  ( -10.37757302488623701, 41.52500000273118275, 31.93888565452638417 ) ) ;
#15695 = CARTESIAN_POINT ( 'NONE',  ( 1.507698388325705758E-15, 11.12499999726881761, -24.62258325217400312 ) ) ;
#15696 = LINE ( 'NONE', #26150, #27631 ) ;
#15697 = ORIENTED_EDGE ( 'NONE', *, *, #7258, .F. ) ;
#15698 = CARTESIAN_POINT ( 'NONE',  ( 10.37757302488624056, 54.77500000273121117, -31.93888565452638417 ) ) ;
#15699 = DIRECTION ( 'NONE',  ( -0.000000000000000000, -1.000000000000000000, -0.000000000000000000 ) ) ;
#15700 = CARTESIAN_POINT ( 'NONE',  ( -7.025853678916393008, 43.22954833425730925, 26.06988505166735592 ) ) ;
#15701 = CARTESIAN_POINT ( 'NONE',  ( 33.58253175000000113, 76.47500000273117848, -10.91162601494193751 ) ) ;
#15702 = VERTEX_POINT ( 'NONE', #15028 ) ;
#15703 = CARTESIAN_POINT ( 'NONE',  ( -33.58253175000000113, 25.12500000273119838, 0.000000000000000000 ) ) ;
#15704 = CARTESIAN_POINT ( 'NONE',  ( -7.505752307973343918, 12.28645833333333037, -28.01184896238290989 ) ) ;
#15705 = EDGE_LOOP ( 'NONE', ( #24953, #5729, #23618, #27741 ) ) ;
#15706 = CARTESIAN_POINT ( 'NONE',  ( -26.29305231718578995, 14.70000000546237118, 19.10302069950538595 ) ) ;
#15707 = CARTESIAN_POINT ( 'NONE',  ( -20.75514604977248823, 60.82500000273121543, -28.56700777964554305 ) ) ;
#15708 = CARTESIAN_POINT ( 'NONE',  ( -28.01184896238290278, 52.67708333333333570, 7.505752307973363457 ) ) ;
#15709 =( BOUNDED_CURVE ( )  B_SPLINE_CURVE ( 2, ( #19645, #22219, #17070, #7100, #20160, #22897, #17583, #4530, #7271, #28385, #28213, #1953, #12598 ),
 .UNSPECIFIED., .F., .T. ) 
 B_SPLINE_CURVE_WITH_KNOTS ( ( 3, 2, 2, 2, 2, 2, 3 ),
 ( 0.4679487179487179516, 0.4692307692307692291, 0.4717948717948717841, 0.4743589743589743390, 0.4769230769230769496, 0.4794871794871795045, 0.4807692307692307820 ),
 .UNSPECIFIED. ) 
 CURVE ( )  GEOMETRIC_REPRESENTATION_ITEM ( )  RATIONAL_B_SPLINE_CURVE ( ( 0.9755282581475768211, 0.9755282581475768211, 1.000000000000000000, 0.9510565162951535312, 1.000000000000000000, 0.9510565162951535312, 1.000000000000000000, 0.9510565162951535312, 1.000000000000000000, 0.9510565162951535312, 1.000000000000000000, 0.9755282581475768211, 0.9755282581475768211 ) ) 
 REPRESENTATION_ITEM ( '' )  );
#15710 = LINE ( 'NONE', #18789, #32200 ) ;
#15711 = CARTESIAN_POINT ( 'NONE',  ( 14.47279130897151944, 3.424999997268799667, -19.92008829642072598 ) ) ;
#15712 = CARTESIAN_POINT ( 'NONE',  ( 20.75514604977249178, 3.825000002731174575, 28.56700777964553950 ) ) ;
#15713 =( BOUNDED_CURVE ( )  B_SPLINE_CURVE ( 2, ( #2666, #28565, #29069, #10386, #7974, #21369, #18118, #31484, #24107, #10553, #2829, #33894, #575 ),
 .UNSPECIFIED., .F., .F. ) 
 B_SPLINE_CURVE_WITH_KNOTS ( ( 3, 2, 2, 2, 2, 2, 3 ),
 ( 0.9038461538461538547, 0.9051282051282051322, 0.9076923076923076872, 0.9102564102564102422, 0.9128205128205127972, 0.9153846153846153522, 0.9166666666666666297 ),
 .UNSPECIFIED. ) 
 CURVE ( )  GEOMETRIC_REPRESENTATION_ITEM ( )  RATIONAL_B_SPLINE_CURVE ( ( 0.9755282581475768211, 0.9755282581475768211, 1.000000000000000000, 0.9510565162951535312, 1.000000000000000000, 0.9510565162951535312, 1.000000000000000000, 0.9510565162951535312, 1.000000000000000000, 0.9510565162951535312, 1.000000000000000000, 0.9755282581475768211, 0.9755282581475768211 ) ) 
 REPRESENTATION_ITEM ( '' )  );
#15714 = DIRECTION ( 'NONE',  ( -0.000000000000000000, -1.000000000000000000, -0.000000000000000000 ) ) ;
#15715 = CARTESIAN_POINT ( 'NONE',  ( 25.98046417659831775, 59.68972249907602645, -15.04653450569338879 ) ) ;
#15716 = CARTESIAN_POINT ( 'NONE',  ( -15.14183272437242067, 14.70000000000000107, -20.84094480462497856 ) ) ;
#15717 = CARTESIAN_POINT ( 'NONE',  ( -28.01184896238290278, 66.42708333333332860, 7.505752307973363457 ) ) ;
#15718 = CARTESIAN_POINT ( 'NONE',  ( -26.29305231718579350, 69.79999999999999716, -19.10302069950537884 ) ) ;
#15719 = CARTESIAN_POINT ( 'NONE',  ( -32.50000000000000000, 13.89999999999999858, -10.55989012756945478 ) ) ;
#15720 = CARTESIAN_POINT ( 'NONE',  ( 13.97622843553589966, 60.84114583333332860, -24.20753774853756113 ) ) ;
#15721 = CARTESIAN_POINT ( 'NONE',  ( 1.577395562988744260E-15, 10.24999999453763877, -25.76082449383753925 ) ) ;
#15722 = CARTESIAN_POINT ( 'NONE',  ( -12.13525491562420910, 70.45000000546237118, 8.816778784387098611 ) ) ;
#15723 = CARTESIAN_POINT ( 'NONE',  ( -24.20753774853730889, 31.90885416666666430, 13.97622843553633842 ) ) ;
#15724 = CARTESIAN_POINT ( 'NONE',  ( 10.37757302488624767, 29.72500000273120691, 31.93888565452638417 ) ) ;
#15725 = CARTESIAN_POINT ( 'NONE',  ( 20.75514604977249178, 71.82500000273118701, 28.56700777964553950 ) ) ;
#15726 = CARTESIAN_POINT ( 'NONE',  ( -20.75514604977248823, 39.07500000273119412, -28.56700777964554305 ) ) ;
#15727 = CARTESIAN_POINT ( 'NONE',  ( -33.58253175000000113, 17.37500000273117706, 0.000000000000000000 ) ) ;
#15728 = CARTESIAN_POINT ( 'NONE',  ( -24.50000000000000000, 6.900000000000014566, -7.960532557706207157 ) ) ;
#15729 = CARTESIAN_POINT ( 'NONE',  ( 26.06988505166735592, 56.12017333425732346, 7.025853678916393896 ) ) ;
#15730 = CARTESIAN_POINT ( 'NONE',  ( -27.16883889988624290, 74.92500000273119554, -19.73931689729374028 ) ) ;
#15731 = CARTESIAN_POINT ( 'NONE',  ( -1.778240108872766143E-15, 65.50000000000000000, -32.49999999999999289 ) ) ;
#15732 = CARTESIAN_POINT ( 'NONE',  ( 6.277390505771533514E-15, 52.50000000000000000, 34.17252228774368916 ) ) ;
#15733 = CARTESIAN_POINT ( 'NONE',  ( 18.94512977948575738, 14.42499999726881654, 13.76444248337723408 ) ) ;
#15734 = CARTESIAN_POINT ( 'NONE',  ( -27.16883889988624290, 62.92500000273118843, -19.73931689729374028 ) ) ;
#15735 = CARTESIAN_POINT ( 'NONE',  ( -4.523095164977116484E-15, 8.624999997268810503, 24.62258325217400312 ) ) ;
#15736 = CARTESIAN_POINT ( 'NONE',  ( 27.16883889988624290, 74.17500000273118133, 19.73931689729373673 ) ) ;
#15737 = CARTESIAN_POINT ( 'NONE',  ( 27.16883889988624290, 5.925000002731190207, 19.73931689729373673 ) ) ;
#15738 = CARTESIAN_POINT ( 'NONE',  ( 14.47279130897151767, 0.9249999972688209837, -19.92008829642072598 ) ) ;
#15739 = CARTESIAN_POINT ( 'NONE',  ( 24.22776226481241224, 17.87798583425730570, -13.94119854578936923 ) ) ;
#15740 = EDGE_LOOP ( 'NONE', ( #21438, #16406, #8330, #11325 ) ) ;
#15741 = VECTOR ( 'NONE', #19731, 1000.000000000000000 ) ;
#15742 = CARTESIAN_POINT ( 'NONE',  ( -33.58253175000000113, 41.12500000273118417, 0.000000000000000000 ) ) ;
#15743 = VERTEX_POINT ( 'NONE', #23084 ) ;
#15744 = CARTESIAN_POINT ( 'NONE',  ( -30.02300923189239512, 42.50781249999997868, 2.654126918244515359E-13 ) ) ;
#15745 = DIRECTION ( 'NONE',  ( 0.000000000000000000, 1.000000000000000000, 0.000000000000000000 ) ) ;
#15746 = CARTESIAN_POINT ( 'NONE',  ( -20.08610463437156923, 4.800000005462381480, 27.64615127144130113 ) ) ;
#15747 = CARTESIAN_POINT ( 'NONE',  ( -26.29305231718578995, 72.19999999999998863, 19.10302069950538595 ) ) ;
#15748 = CARTESIAN_POINT ( 'NONE',  ( -15.01150461594642138, 19.01822916666666785, -26.00068869287340334 ) ) ;
#15749 = CARTESIAN_POINT ( 'NONE',  ( 24.50000000000000000, 2.000000000000001776, 0.000000000000000000 ) ) ;
#15750 = CARTESIAN_POINT ( 'NONE',  ( -33.58253175000000113, 13.47500000273118914, 10.91162601494193929 ) ) ;
#15751 = ADVANCED_FACE ( 'NONE', ( #1792, #30109 ), #25493, .T. ) ;
#15752 = CARTESIAN_POINT ( 'NONE',  ( -20.08610463437156923, 60.29999999999998295, 27.64615127144130113 ) ) ;
#15753 = CARTESIAN_POINT ( 'NONE',  ( 1.555960095263670572E-15, 8.249999994537619230, -24.50000000000000000 ) ) ;
#15754 = FACE_OUTER_BOUND ( 'NONE', #1641, .T. ) ;
#15755 = CARTESIAN_POINT ( 'NONE',  ( 7.468012846824281681, 38.63503499907601224, -28.02196122052058058 ) ) ;
#15756 = CARTESIAN_POINT ( 'NONE',  ( -11.25946833292375793, 73.17500000273119554, -8.180482586598733619 ) ) ;
#15757 = CARTESIAN_POINT ( 'NONE',  ( -7.505752307973343918, 43.22395833333332860, -28.01184896238290989 ) ) ;
#15758 = CONTEXT_DEPENDENT_SHAPE_REPRESENTATION ( #30687, #2470 ) ;
#15759 = EDGE_CURVE ( 'NONE', #1581, #26581, #10081, .T. ) ;
#15760 = DIRECTION ( 'NONE',  ( -1.000000000000000000, 0.000000000000000000, 0.000000000000000000 ) ) ;
#15761 = CARTESIAN_POINT ( 'NONE',  ( -15.14183272437242067, 12.70000000000000639, -20.84094480462497856 ) ) ;
#15762 = CARTESIAN_POINT ( 'NONE',  ( -20.75514604977248823, 79.07500000273121543, -28.56700777964554305 ) ) ;
#15763 = DIRECTION ( 'NONE',  ( -1.224646799147353454E-16, 1.000000000000000000, -0.000000000000000000 ) ) ;
#15764 = CARTESIAN_POINT ( 'NONE',  ( -26.06988505166722803, 64.98920166574268364, 7.025853678916877953 ) ) ;
#15765 = CARTESIAN_POINT ( 'NONE',  ( -20.75514604977248112, 49.42500000273118133, 28.56700777964554661 ) ) ;
#15766 = CARTESIAN_POINT ( 'NONE',  ( -2.162160676586881955E-15, 52.87500000273119838, -35.31076352940723240 ) ) ;
#15767 = CARTESIAN_POINT ( 'NONE',  ( 27.16883889988623935, 34.57500000273120122, -19.73931689729374384 ) ) ;
#15768 = VECTOR ( 'NONE', #25900, 1000.000000000000000 ) ;
#15769 = CARTESIAN_POINT ( 'NONE',  ( -19.09188309203660694, 14.57812499999999645, 19.09188309203694800 ) ) ;
#15770 = CARTESIAN_POINT ( 'NONE',  ( -32.50000000000000000, 62.09999999999998721, 10.55989012756946366 ) ) ;
#15771 = CARTESIAN_POINT ( 'NONE',  ( 0.000000000000000000, 0.000000000000000000, 0.000000000000000000 ) ) ;
#15772 = CARTESIAN_POINT ( 'NONE',  ( -5.147494310547213736, 27.55125428154684997, -32.50000000000007105 ) ) ;
#15773 = CARTESIAN_POINT ( 'NONE',  ( 10.37757302488624056, 14.52500000273120051, -31.93888565452638417 ) ) ;
#15774 = CARTESIAN_POINT ( 'NONE',  ( 5.334720326618300005E-14, 72.00000000546238255, -32.50000000000000000 ) ) ;
#15775 = DIRECTION ( 'NONE',  ( 0.000000000000000000, -0.000000000000000000, -1.000000000000000000 ) ) ;
#15776 = CARTESIAN_POINT ( 'NONE',  ( 3.880418787951153803, 9.301254276084472750, 24.49999999999999645 ) ) ;
#15777 = CARTESIAN_POINT ( 'NONE',  ( 26.09010956794244507, 22.30690999907601579, 6.950374756619249084 ) ) ;
#15778 = CARTESIAN_POINT ( 'NONE',  ( 20.08610463437158344, 33.20000000546238539, 27.64615127144129403 ) ) ;
#15779 = DIRECTION ( 'NONE',  ( -0.000000000000000000, -1.000000000000000000, -0.000000000000000000 ) ) ;
#15780 = CARTESIAN_POINT ( 'NONE',  ( 10.37757302488624767, 23.72500000273119980, 31.93888565452638417 ) ) ;
#15781 = CARTESIAN_POINT ( 'NONE',  ( 24.20753774853731244, 40.50260416666666430, -13.97622843553632599 ) ) ;
#15782 = ORIENTED_EDGE ( 'NONE', *, *, #22470, .T. ) ;
#15783 = CARTESIAN_POINT ( 'NONE',  ( 20.75514604977249178, 59.82500000273117280, 28.56700777964553950 ) ) ;
#15784 = ORIENTED_EDGE ( 'NONE', *, *, #1373, .T. ) ;
#15785 = CARTESIAN_POINT ( 'NONE',  ( -20.50609665441004736, 11.99999999999999645, -20.50609665440969565 ) ) ;
#15786 = CARTESIAN_POINT ( 'NONE',  ( -7.468012846824771955, 17.16184000092397000, -28.02196122052045624 ) ) ;
#15787 = ORIENTED_EDGE ( 'NONE', *, *, #29234, .T. ) ;
#15788 = CARTESIAN_POINT ( 'NONE',  ( 20.75514604977248467, 4.425000002731183990, -28.56700777964554305 ) ) ;
#15789 = DIRECTION ( 'NONE',  ( -0.8660254037844398178, 0.4999999999999979461, -0.000000000000000000 ) ) ;
#15790 = CARTESIAN_POINT ( 'NONE',  ( -2.162160676586881955E-15, 32.87500000273118417, -35.31076352940723240 ) ) ;
#15791 = CARTESIAN_POINT ( 'NONE',  ( 32.50000000000000000, 39.50000000546238965, -3.980102097228898626E-15 ) ) ;
#15792 = ADVANCED_FACE ( 'NONE', ( #24971 ), #26695, .F. ) ;
#15793 = CARTESIAN_POINT ( 'NONE',  ( 4.635254915624209993, 73.40000000000001990, -14.26584774442730463 ) ) ;
#15794 = PLANE ( 'NONE',  #15980 ) ;
#15795 = CARTESIAN_POINT ( 'NONE',  ( 19.82091636218621034, 5.549999994537619052, 14.40073868116559730 ) ) ;
#15796 = CARTESIAN_POINT ( 'NONE',  ( 27.16883889988624290, 48.17500000273117422, 19.73931689729373673 ) ) ;
#15797 = CARTESIAN_POINT ( 'NONE',  ( 20.08610463437157279, 21.29999999999999716, -27.64615127144129758 ) ) ;
#15798 = CARTESIAN_POINT ( 'NONE',  ( 32.50000000000000000, 25.09999999999999432, -10.55989012756945833 ) ) ;
#15799 = CARTESIAN_POINT ( 'NONE',  ( -4.732186688966233175E-15, 7.499999999999995559, 25.76082449383753925 ) ) ;
#15800 = CARTESIAN_POINT ( 'NONE',  ( 20.75514604977249178, 71.82500000273118701, 28.56700777964553950 ) ) ;
#15801 = CARTESIAN_POINT ( 'NONE',  ( 24.50000000000000000, 1.749999994537621006, 0.000000000000000000 ) ) ;
#15802 = CARTESIAN_POINT ( 'NONE',  ( 9.081462083391590667, 73.99999999999997158, -10.89876187695312915 ) ) ;
#15803 = CARTESIAN_POINT ( 'NONE',  ( 20.75514604977248467, 58.67500000273118843, -28.56700777964554305 ) ) ;
#15804 = CARTESIAN_POINT ( 'NONE',  ( 20.08610463437157279, 73.29999999999996874, -27.64615127144129758 ) ) ;
#15805 = CARTESIAN_POINT ( 'NONE',  ( 6.486482029760649416E-15, 13.62500000273118417, 35.31076352940723240 ) ) ;
#15806 = CARTESIAN_POINT ( 'NONE',  ( 13.94119854578937812, 29.04986083425730570, 24.22776226481240514 ) ) ;
#15807 =( BOUNDED_CURVE ( )  B_SPLINE_CURVE ( 2, ( #8405, #16651, #10995, #29341, #26778, #32412, #24041, #21468, #29839, #16478, #3267, #674, #29500 ),
 .UNSPECIFIED., .F., .T. ) 
 B_SPLINE_CURVE_WITH_KNOTS ( ( 3, 2, 2, 2, 2, 2, 3 ),
 ( 0.3910256410256410242, 0.3923076923076923017, 0.3948717948717948567, 0.3974358974358974117, 0.4000000000000000222, 0.4025641025641025772, 0.4038461538461538547 ),
 .UNSPECIFIED. ) 
 CURVE ( )  GEOMETRIC_REPRESENTATION_ITEM ( )  RATIONAL_B_SPLINE_CURVE ( ( 0.9755282581475768211, 0.9755282581475768211, 1.000000000000000000, 0.9510565162951535312, 1.000000000000000000, 0.9510565162951535312, 1.000000000000000000, 0.9510565162951535312, 1.000000000000000000, 0.9510565162951535312, 1.000000000000000000, 0.9755282581475768211, 0.9755282581475768211 ) ) 
 REPRESENTATION_ITEM ( '' )  );
#15808 = CARTESIAN_POINT ( 'NONE',  ( 20.30017892146906533, 66.99999999999995737, -26.02681000244154674 ) ) ;
#15809 = CARTESIAN_POINT ( 'NONE',  ( 6.486482029760648627E-15, 3.875000002731201931, 35.31076352940722529 ) ) ;
#15810 = CARTESIAN_POINT ( 'NONE',  ( 27.16883889988623935, 34.32500000273118701, -19.73931689729374384 ) ) ;
#15811 = CARTESIAN_POINT ( 'NONE',  ( -20.08610463437157989, 64.20000000546238539, -27.64615127144129758 ) ) ;
#15812 = DIRECTION ( 'NONE',  ( -0.4999999999999996669, 0.000000000000000000, 0.8660254037844388186 ) ) ;
#15813 = CARTESIAN_POINT ( 'NONE',  ( -13.91746824999999532, 76.97500000273119269, 4.522059556121122093 ) ) ;
#15814 = CARTESIAN_POINT ( 'NONE',  ( 15.04653450569339945, 46.79909749907603356, 25.98046417659831775 ) ) ;
#15815 = CARTESIAN_POINT ( 'NONE',  ( 10.04305231718578817, 55.90000000546240244, -30.90933677959249337 ) ) ;
#15816 = CIRCLE ( 'NONE', #16350, 14.00000000000000178 ) ;
#15817 = CARTESIAN_POINT ( 'NONE',  ( -8.601468415847518756, 77.07500000273117280, -11.83890561707634781 ) ) ;
#15818 =( LENGTH_UNIT ( ) NAMED_UNIT ( * ) SI_UNIT ( .MILLI., .METRE. ) );
#15819 = CARTESIAN_POINT ( 'NONE',  ( -24.20753774853756823, 18.73177083333332149, -13.97622843553588723 ) ) ;
#15820 = CARTESIAN_POINT ( 'NONE',  ( 18.94512977948576093, 3.324999997268818230, -13.76444248337722875 ) ) ;
#15821 = CARTESIAN_POINT ( 'NONE',  ( -20.08610463437156923, 68.80000000546236549, 27.64615127144130113 ) ) ;
#15822 = CARTESIAN_POINT ( 'NONE',  ( 2.740863092043355209E-13, 21.02343749999999645, 30.02300923189239512 ) ) ;
#15823 = CARTESIAN_POINT ( 'NONE',  ( 10.37757302488624056, 30.77500000273118630, -31.93888565452638417 ) ) ;
#15824 = CARTESIAN_POINT ( 'NONE',  ( -18.94512977948575738, 13.92499999726881654, -13.76444248337723231 ) ) ;
#15825 = EDGE_LOOP ( 'NONE', ( #23582, #25260, #27641, #12983 ) ) ;
#15826 = CARTESIAN_POINT ( 'NONE',  ( 0.04044903254992426173, 44.80506916759064495, -30.02300923189239867 ) ) ;
#15827 = CARTESIAN_POINT ( 'NONE',  ( 26.29305231718579350, 19.30000000546237970, 19.10302069950537529 ) ) ;
#15828 = CARTESIAN_POINT ( 'NONE',  ( -2.584737979205441561E-13, 53.67968750000000000, -30.02300923189239512 ) ) ;
#15829 = DIRECTION ( 'NONE',  ( -1.224646799147353454E-16, 1.000000000000000000, -0.000000000000000000 ) ) ;
#15830 = CARTESIAN_POINT ( 'NONE',  ( -33.58253175000000113, 53.47500000273117848, 10.91162601494193929 ) ) ;
#15831 = CARTESIAN_POINT ( 'NONE',  ( -26.29305231718578995, 58.70000000546238539, 19.10302069950538595 ) ) ;
#15832 = CYLINDRICAL_SURFACE ( 'NONE', #31915, 24.50000000000000000 ) ;
#15833 = CARTESIAN_POINT ( 'NONE',  ( 33.58253175000000823, 42.02500000273118985, 10.91162601494192863 ) ) ;
#15834 = CARTESIAN_POINT ( 'NONE',  ( 33.58253175000000113, 68.37500000273119838, -4.112674001490185761E-15 ) ) ;
#15835 = LINE ( 'NONE', #20818, #22754 ) ;
#15836 = CARTESIAN_POINT ( 'NONE',  ( -33.58253175000000113, 61.22500000273119269, 10.91162601494193929 ) ) ;
#15837 = CARTESIAN_POINT ( 'NONE',  ( -15.01150461594595775, 17.87239583333332860, 26.00068869287368756 ) ) ;
#15838 = CARTESIAN_POINT ( 'NONE',  ( 32.50000000000000711, 46.90000000000000568, 10.55989012756945122 ) ) ;
#15839 = CARTESIAN_POINT ( 'NONE',  ( -7.236395654485757944, 5.224999997268803043, -22.27133577429736988 ) ) ;
#15840 = CARTESIAN_POINT ( 'NONE',  ( 27.16883889988623935, 8.575000002731202997, -19.73931689729374384 ) ) ;
#15841 = CARTESIAN_POINT ( 'NONE',  ( 40.00000000000000000, 66.99999999999998579, -23.09401076758505766 ) ) ;
#15842 = CARTESIAN_POINT ( 'NONE',  ( -26.09010956794245217, 34.33815999907601224, -6.950374756619243755 ) ) ;
#15843 = CARTESIAN_POINT ( 'NONE',  ( 11.25946833292375793, 72.57500000273120122, -8.180482586598735395 ) ) ;
#15844 = CARTESIAN_POINT ( 'NONE',  ( 27.16883889988624290, 78.17500000273119554, 19.73931689729373673 ) ) ;
#15845 = DIRECTION ( 'NONE',  ( -0.000000000000000000, -1.000000000000000000, -0.000000000000000000 ) ) ;
#15846 = CARTESIAN_POINT ( 'NONE',  ( 10.37757302488624767, 75.97500000273120691, 31.93888565452638417 ) ) ;
#15847 = EDGE_LOOP ( 'NONE', ( #11055, #435, #13327, #1350 ) ) ;
#15848 =( BOUNDED_SURFACE ( )  B_SPLINE_SURFACE ( 1, 2, ( 
 ( #11137, #21606, #20937, #31386, #7876, #13197, #23674, #29142, #5646, #138, #10629, #26582, #482, #32049, #8550, #28639, #5135, #31550, #28979, #19528, #11622, #29809, #3739, #27580, #26907, #6137, #22105, #16955, #3904, #24666, #6310, #3571, #32550, #19195, #29978, #14210, #1310, #16455, #6483, #29634, #11297, #14544, #32713, #14042, #30139, #14373, #9210, #6643, #977, #9049, #24832, #1140, #17123, #27414, #11792, #19693, #22271, #3406, #4069, #25003, #1485, #19366, #22430, #11959, #32877, #19035, #29473, #816, #32385, #5978, #13878, #24345, #21776, #32223, #8712, #16622, #11461, #27076, #16788, #24503, #21935, #8880, #27246, #19857, #33227, #17806, #6981, #33405, #2171, #17631, #28432, #4922, #28264, #22775, #1651, #20212, #20034, #9726, #17984, #6809, #30480, #30828, #17464, #30652, #7322, #12477, #4750, #27751, #30312, #28092, #7149, #15227, #9556, #27924, #4581, #4407, #25171, #1825, #15402, #9902, #22598, #14884, #31003, #7500, #15058, #17288, #22947, #14713, #23115, #33052, #4239, #12126, #25345, #12303, #25525, #10077, #2002, #20379, #23293, #33578, #20557, #25690, #12644, #25858, #2347, #12822, #9376, #8173, #10418, #2864, #5094, #31516, #28938, #33927, #20895, #13333, #21067, #8010, #18495, #10253, #5437, #31344, #16091, #7666, #20734, #26542, #12994, #3037, #15581, #7836, #31176, #13510, #18153, #23973, #28595, #18829, #29274, #5775, #2698, #21237, #10926 ),
 ( #10589, #15918, #26374, #23807, #272, #26032, #2525, #443, #23634, #23465, #16255, #21400, #5267, #18326, #26711, #3208, #13676, #10759, #31846, #28771, #15749, #31680, #33761, #13158, #26204, #100, #18664, #29102, #5607, #8339, #19657, #1102, #13839, #29940, #6444, #16916, #3700, #24467, #8841, #24306, #21897, #8678, #6273, #32677, #9173, #19160, #11752, #3532, #32510, #29766, #24793, #942, #27037, #4030, #3865, #14337, #16750, #780, #32347, #9011, #29440, #1272, #19491, #11262, #27208, #5941, #19324, #14172, #21738, #32183, #24629, #11422, #11585, #22066, #607, #27376, #29599, #22233, #32013, #11099, #30100, #3369, #6606, #16422, #6101, #21568, #17083, #8509, #27543, #18996, #24140, #26874, #16582, #14004, #1965, #25655, #28225, #30789, #28054, #32843, #25310, #27886, #1783, #20171, #12260, #4542, #22737, #11924, #9335, #17765, #4369, #4202, #30964, #15192, #19996, #19820, #7463, #10042, #17946, #7110, #12609, #33010, #30444, #30614, #28395, #14844, #17253, #1446, #25486, #14674, #17592, #12440, #20519, #22910, #25134, #20339, #7282, #4711, #15016, #33187, #9690, #1611, #33366, #9515, #9862, #23078, #33539, #6942, #2134, #14505, #24964, #22394, #30272, #6772, #27714, #12089, #22558, #17425, #12953, #20696, #31303, #403, #5399, #18110, #5055, #26502, #2995, #28731, #25820, #7968, #10216, #18625, #28559, #2310, #12783, #31138, #15539, #21027, #13468, #23934, #33887 ) ),
 .UNSPECIFIED., .F., .F., .F. ) 
 B_SPLINE_SURFACE_WITH_KNOTS ( ( 2, 2 ),
 ( 3, 2, 2, 2, 2, 2, 2, 2, 2, 2, 2, 2, 2, 2, 2, 2, 2, 2, 2, 2, 2, 2, 2, 2, 2, 2, 2, 2, 2, 2, 2, 2, 2, 2, 2, 2, 2, 2, 2, 2, 2, 2, 2, 2, 2, 2, 2, 2, 2, 2, 2, 2, 2, 2, 2, 2, 2, 2, 2, 2, 2, 2, 2, 2, 2, 2, 2, 2, 2, 2, 2, 2, 2, 2, 2, 2, 2, 2, 2, 2, 2, 2, 2, 2, 2, 2, 2, 2, 2, 2, 3 ),
 ( 0.000000000000000000, 1.000000000000000000 ),
 ( 0.000000000000000000, 0.01111111111111111154, 0.02222222222222222307, 0.03333333333333333287, 0.04444444444444444614, 0.05555555555555555247, 0.06666666666666666574, 0.07777777777777777901, 0.08888888888888889228, 0.1000000000000000056, 0.1111111111111111049, 0.1222222222222222182, 0.1333333333333333315, 0.1444444444444444309, 0.1555555555555555580, 0.1666666666666666574, 0.1777777777777777846, 0.1888888888888888840, 0.2000000000000000111, 0.2111111111111111105, 0.2222222222222222099, 0.2333333333333333370, 0.2444444444444444364, 0.2555555555555555358, 0.2666666666666666630, 0.2777777777777777901, 0.2888888888888888618, 0.2999999999999999889, 0.3111111111111111160, 0.3222222222222222432, 0.3333333333333333148, 0.3444444444444444420, 0.3555555555555555691, 0.3666666666666666408, 0.3777777777777777679, 0.3888888888888888951, 0.4000000000000000222, 0.4111111111111110938, 0.4222222222222222210, 0.4333333333333333481, 0.4444444444444444198, 0.4555555555555555469, 0.4666666666666666741, 0.4777777777777778012, 0.4888888888888888729, 0.5000000000000000000, 0.5111111111111110716, 0.5222222222222222543, 0.5333333333333333259, 0.5444444444444443976, 0.5555555555555555802, 0.5666666666666666519, 0.5777777777777777235, 0.5888888888888889062, 0.5999999999999999778, 0.6111111111111111605, 0.6222222222222222321, 0.6333333333333333037, 0.6444444444444444864, 0.6555555555555555580, 0.6666666666666666297, 0.6777777777777778123, 0.6888888888888888840, 0.6999999999999999556, 0.7111111111111111382, 0.7222222222222222099, 0.7333333333333332815, 0.7444444444444444642, 0.7555555555555555358, 0.7666666666666667185, 0.7777777777777777901, 0.7888888888888888618, 0.8000000000000000444, 0.8111111111111111160, 0.8222222222222221877, 0.8333333333333333703, 0.8444444444444444420, 0.8555555555555555136, 0.8666666666666666963, 0.8777777777777777679, 0.8888888888888888395, 0.9000000000000000222, 0.9111111111111110938, 0.9222222222222222765, 0.9333333333333333481, 0.9444444444444444198, 0.9555555555555556024, 0.9666666666666666741, 0.9777777777777777457, 0.9888888888888889284, 1.000000000000000000 ),
 .UNSPECIFIED. ) 
 GEOMETRIC_REPRESENTATION_ITEM ( )  RATIONAL_B_SPLINE_SURFACE ( (
 ( 1.000000000000000000, 0.9510565162951535312, 1.000000000000000000, 0.9510565162951535312, 1.000000000000000000, 0.9510565162951535312, 1.000000000000000000, 0.9510565162951535312, 1.000000000000000000, 0.9510565162951535312, 1.000000000000000000, 0.9510565162951535312, 1.000000000000000000, 0.9510565162951535312, 1.000000000000000000, 0.9510565162951535312, 1.000000000000000000, 0.9510565162951535312, 1.000000000000000000, 0.9510565162951535312, 1.000000000000000000, 0.9510565162951535312, 1.000000000000000000, 0.9510565162951535312, 1.000000000000000000, 0.9510565162951535312, 1.000000000000000000, 0.9510565162951535312, 1.000000000000000000, 0.9510565162951535312, 1.000000000000000000, 0.9510565162951535312, 1.000000000000000000, 0.9510565162951535312, 1.000000000000000000, 0.9510565162951535312, 1.000000000000000000, 0.9510565162951535312, 1.000000000000000000, 0.9510565162951535312, 1.000000000000000000, 0.9510565162951535312, 1.000000000000000000, 0.9510565162951535312, 1.000000000000000000, 0.9510565162951535312, 1.000000000000000000, 0.9510565162951535312, 1.000000000000000000, 0.9510565162951535312, 1.000000000000000000, 0.9510565162951535312, 1.000000000000000000, 0.9510565162951535312, 1.000000000000000000, 0.9510565162951535312, 1.000000000000000000, 0.9510565162951535312, 1.000000000000000000, 0.9510565162951535312, 1.000000000000000000, 0.9510565162951535312, 1.000000000000000000, 0.9510565162951535312, 1.000000000000000000, 0.9510565162951535312, 1.000000000000000000, 0.9510565162951535312, 1.000000000000000000, 0.9510565162951535312, 1.000000000000000000, 0.9510565162951535312, 1.000000000000000000, 0.9510565162951535312, 1.000000000000000000, 0.9510565162951535312, 1.000000000000000000, 0.9510565162951535312, 1.000000000000000000, 0.9510565162951535312, 1.000000000000000000, 0.9510565162951535312, 1.000000000000000000, 0.9510565162951535312, 1.000000000000000000, 0.9510565162951535312, 1.000000000000000000, 0.9510565162951535312, 1.000000000000000000, 0.9510565162951535312, 1.000000000000000000, 0.9510565162951535312, 1.000000000000000000, 0.9510565162951535312, 1.000000000000000000, 0.9510565162951535312, 1.000000000000000000, 0.9510565162951535312, 1.000000000000000000, 0.9510565162951535312, 1.000000000000000000, 0.9510565162951535312, 1.000000000000000000, 0.9510565162951535312, 1.000000000000000000, 0.9510565162951535312, 1.000000000000000000, 0.9510565162951535312, 1.000000000000000000, 0.9510565162951535312, 1.000000000000000000, 0.9510565162951535312, 1.000000000000000000, 0.9510565162951535312, 1.000000000000000000, 0.9510565162951535312, 1.000000000000000000, 0.9510565162951535312, 1.000000000000000000, 0.9510565162951535312, 1.000000000000000000, 0.9510565162951535312, 1.000000000000000000, 0.9510565162951535312, 1.000000000000000000, 0.9510565162951535312, 1.000000000000000000, 0.9510565162951535312, 1.000000000000000000, 0.9510565162951535312, 1.000000000000000000, 0.9510565162951535312, 1.000000000000000000, 0.9510565162951535312, 1.000000000000000000, 0.9510565162951535312, 1.000000000000000000, 0.9510565162951535312, 1.000000000000000000, 0.9510565162951535312, 1.000000000000000000, 0.9510565162951535312, 1.000000000000000000, 0.9510565162951535312, 1.000000000000000000, 0.9510565162951535312, 1.000000000000000000, 0.9510565162951535312, 1.000000000000000000, 0.9510565162951535312, 1.000000000000000000, 0.9510565162951535312, 1.000000000000000000, 0.9510565162951535312, 1.000000000000000000, 0.9510565162951535312, 1.000000000000000000, 0.9510565162951535312, 1.000000000000000000, 0.9510565162951535312, 1.000000000000000000, 0.9510565162951535312, 1.000000000000000000, 0.9510565162951535312, 1.000000000000000000, 0.9510565162951535312, 1.000000000000000000, 0.9510565162951535312, 1.000000000000000000, 0.9510565162951535312, 1.000000000000000000, 0.9510565162951535312, 1.000000000000000000, 0.9510565162951535312, 1.000000000000000000, 0.9510565162951535312, 1.000000000000000000, 0.9510565162951535312, 1.000000000000000000, 0.9510565162951535312, 1.000000000000000000),
 ( 1.000000000000000000, 0.9510565162951535312, 1.000000000000000000, 0.9510565162951535312, 1.000000000000000000, 0.9510565162951535312, 1.000000000000000000, 0.9510565162951535312, 1.000000000000000000, 0.9510565162951535312, 1.000000000000000000, 0.9510565162951535312, 1.000000000000000000, 0.9510565162951535312, 1.000000000000000000, 0.9510565162951535312, 1.000000000000000000, 0.9510565162951535312, 1.000000000000000000, 0.9510565162951535312, 1.000000000000000000, 0.9510565162951535312, 1.000000000000000000, 0.9510565162951535312, 1.000000000000000000, 0.9510565162951535312, 1.000000000000000000, 0.9510565162951535312, 1.000000000000000000, 0.9510565162951535312, 1.000000000000000000, 0.9510565162951535312, 1.000000000000000000, 0.9510565162951535312, 1.000000000000000000, 0.9510565162951535312, 1.000000000000000000, 0.9510565162951535312, 1.000000000000000000, 0.9510565162951535312, 1.000000000000000000, 0.9510565162951535312, 1.000000000000000000, 0.9510565162951535312, 1.000000000000000000, 0.9510565162951535312, 1.000000000000000000, 0.9510565162951535312, 1.000000000000000000, 0.9510565162951535312, 1.000000000000000000, 0.9510565162951535312, 1.000000000000000000, 0.9510565162951535312, 1.000000000000000000, 0.9510565162951535312, 1.000000000000000000, 0.9510565162951535312, 1.000000000000000000, 0.9510565162951535312, 1.000000000000000000, 0.9510565162951535312, 1.000000000000000000, 0.9510565162951535312, 1.000000000000000000, 0.9510565162951535312, 1.000000000000000000, 0.9510565162951535312, 1.000000000000000000, 0.9510565162951535312, 1.000000000000000000, 0.9510565162951535312, 1.000000000000000000, 0.9510565162951535312, 1.000000000000000000, 0.9510565162951535312, 1.000000000000000000, 0.9510565162951535312, 1.000000000000000000, 0.9510565162951535312, 1.000000000000000000, 0.9510565162951535312, 1.000000000000000000, 0.9510565162951535312, 1.000000000000000000, 0.9510565162951535312, 1.000000000000000000, 0.9510565162951535312, 1.000000000000000000, 0.9510565162951535312, 1.000000000000000000, 0.9510565162951535312, 1.000000000000000000, 0.9510565162951535312, 1.000000000000000000, 0.9510565162951535312, 1.000000000000000000, 0.9510565162951535312, 1.000000000000000000, 0.9510565162951535312, 1.000000000000000000, 0.9510565162951535312, 1.000000000000000000, 0.9510565162951535312, 1.000000000000000000, 0.9510565162951535312, 1.000000000000000000, 0.9510565162951535312, 1.000000000000000000, 0.9510565162951535312, 1.000000000000000000, 0.9510565162951535312, 1.000000000000000000, 0.9510565162951535312, 1.000000000000000000, 0.9510565162951535312, 1.000000000000000000, 0.9510565162951535312, 1.000000000000000000, 0.9510565162951535312, 1.000000000000000000, 0.9510565162951535312, 1.000000000000000000, 0.9510565162951535312, 1.000000000000000000, 0.9510565162951535312, 1.000000000000000000, 0.9510565162951535312, 1.000000000000000000, 0.9510565162951535312, 1.000000000000000000, 0.9510565162951535312, 1.000000000000000000, 0.9510565162951535312, 1.000000000000000000, 0.9510565162951535312, 1.000000000000000000, 0.9510565162951535312, 1.000000000000000000, 0.9510565162951535312, 1.000000000000000000, 0.9510565162951535312, 1.000000000000000000, 0.9510565162951535312, 1.000000000000000000, 0.9510565162951535312, 1.000000000000000000, 0.9510565162951535312, 1.000000000000000000, 0.9510565162951535312, 1.000000000000000000, 0.9510565162951535312, 1.000000000000000000, 0.9510565162951535312, 1.000000000000000000, 0.9510565162951535312, 1.000000000000000000, 0.9510565162951535312, 1.000000000000000000, 0.9510565162951535312, 1.000000000000000000, 0.9510565162951535312, 1.000000000000000000, 0.9510565162951535312, 1.000000000000000000, 0.9510565162951535312, 1.000000000000000000, 0.9510565162951535312, 1.000000000000000000, 0.9510565162951535312, 1.000000000000000000, 0.9510565162951535312, 1.000000000000000000, 0.9510565162951535312, 1.000000000000000000, 0.9510565162951535312, 1.000000000000000000, 0.9510565162951535312, 1.000000000000000000, 0.9510565162951535312, 1.000000000000000000) ) ) 
 REPRESENTATION_ITEM ( '' )  SURFACE ( )  );
#15849 = CARTESIAN_POINT ( 'NONE',  ( 23.41746824999999887, 17.12499999726882649, 0.000000000000000000 ) ) ;
#15850 = CARTESIAN_POINT ( 'NONE',  ( -19.09188309203694445, 63.56249999999999289, -19.09188309203661049 ) ) ;
#15851 = CARTESIAN_POINT ( 'NONE',  ( 27.16883889988623935, 54.32500000273120122, -19.73931689729374384 ) ) ;
#15852 = CARTESIAN_POINT ( 'NONE',  ( -20.75514604977248112, 17.67500000273117422, 28.56700777964554661 ) ) ;
#15853 = CARTESIAN_POINT ( 'NONE',  ( -33.58253175000000113, 79.12500000273118417, 0.000000000000000000 ) ) ;
#15854 = CARTESIAN_POINT ( 'NONE',  ( 6.988114217768294445, 38.06770833333332860, 26.07999730980477437 ) ) ;
#15855 = CARTESIAN_POINT ( 'NONE',  ( 20.53372385742072481, 31.48475666759063074, -20.47846945139902175 ) ) ;
#15856 = CARTESIAN_POINT ( 'NONE',  ( 28.02196122052058413, 18.86940999907601935, 7.468012846824272799 ) ) ;
#15857 = CARTESIAN_POINT ( 'NONE',  ( 6.277390505771533514E-15, 71.00000000546235412, 34.17252228774368916 ) ) ;
#15858 = CARTESIAN_POINT ( 'NONE',  ( 33.25271216035365285, 52.00000000000002132, 3.649504031948850979 ) ) ;
#15859 = CARTESIAN_POINT ( 'NONE',  ( -33.58253175000000113, 37.02500000273116854, -10.91162601494193041 ) ) ;
#15860 = CARTESIAN_POINT ( 'NONE',  ( -24.18731323226221974, 44.22097249907603356, 14.01125832528330406 ) ) ;
#15861 = CARTESIAN_POINT ( 'NONE',  ( -7.236395654485757944, 9.224999997268806595, -22.27133577429736988 ) ) ;
#15862 = CARTESIAN_POINT ( 'NONE',  ( -10.04305231718578462, 2.900000005462366470, 30.90933677959249337 ) ) ;
#15863 = ORIENTED_EDGE ( 'NONE', *, *, #22368, .F. ) ;
#15864 = CARTESIAN_POINT ( 'NONE',  ( -20.75514604977248823, 55.07500000273117990, -28.56700777964554305 ) ) ;
#15865 = LINE ( 'NONE', #21352, #6409 ) ;
#15866 = CARTESIAN_POINT ( 'NONE',  ( 26.06988505166735592, 38.93267333425729504, 7.025853678916393896 ) ) ;
#15867 = CARTESIAN_POINT ( 'NONE',  ( -20.75514604977248823, 71.07500000273117280, -28.56700777964554305 ) ) ;
#15868 = VERTEX_POINT ( 'NONE', #13767 ) ;
#15869 = CARTESIAN_POINT ( 'NONE',  ( 33.58253175000000113, 24.22500000273119625, -10.91162601494193751 ) ) ;
#15870 = CARTESIAN_POINT ( 'NONE',  ( -15.01150461594642138, 12.14322916666666430, -26.00068869287340334 ) ) ;
#15871 = EDGE_LOOP ( 'NONE', ( #21495, #25163, #32628, #9642 ) ) ;
#15872 = CARTESIAN_POINT ( 'NONE',  ( 3.980102097228898626E-15, 80.00000000000001421, 32.50000000000000000 ) ) ;
#15873 = CARTESIAN_POINT ( 'NONE',  ( -33.58253175000000113, 63.22500000273119269, 10.91162601494193929 ) ) ;
#15874 = CARTESIAN_POINT ( 'NONE',  ( -26.00068869287340334, 45.65885416666666430, 15.01150461594643382 ) ) ;
#15875 = DIRECTION ( 'NONE',  ( 0.000000000000000000, 1.000000000000000000, 0.000000000000000000 ) ) ;
#15876 = CARTESIAN_POINT ( 'NONE',  ( -7.236395654485757944, 5.724999997268803931, -22.27133577429736988 ) ) ;
#15877 = CARTESIAN_POINT ( 'NONE',  ( 6.486482029760649416E-15, 1.625000002731185944, 35.31076352940723240 ) ) ;
#15878 = CARTESIAN_POINT ( 'NONE',  ( -33.58253175000000113, 31.37500000273119127, 0.000000000000000000 ) ) ;
#15879 = CARTESIAN_POINT ( 'NONE',  ( 0.000000000000000000, 16.99999999999998579, -24.50000000000000000 ) ) ;
#15880 = CARTESIAN_POINT ( 'NONE',  ( 28.02196122052058413, 60.11940999907602645, 7.468012846824272799 ) ) ;
#15881 = CARTESIAN_POINT ( 'NONE',  ( 1.555960095263670572E-15, 14.50000000000000178, -24.50000000000000000 ) ) ;
#15882 = CARTESIAN_POINT ( 'NONE',  ( 8.601468415847516980, 78.17500000273118133, -11.83890561707634781 ) ) ;
#15883 = CARTESIAN_POINT ( 'NONE',  ( 5.147494310547434893, 75.05125428700921475, 32.49999999999999289 ) ) ;
#15884 = EDGE_CURVE ( 'NONE', #25987, #1179, #4358, .T. ) ;
#15885 = CARTESIAN_POINT ( 'NONE',  ( -26.29305231718578995, 18.20000000000000639, 19.10302069950538595 ) ) ;
#15886 = CARTESIAN_POINT ( 'NONE',  ( -19.09188309203660694, 59.26562500000000000, 19.09188309203694800 ) ) ;
#15887 = CARTESIAN_POINT ( 'NONE',  ( 23.41746825000000243, 1.224999997268811480, -7.608796670333727974 ) ) ;
#15888 = CARTESIAN_POINT ( 'NONE',  ( -9.270509831248421762, 72.55000000546236549, 12.75976212528060039 ) ) ;
#15889 = CARTESIAN_POINT ( 'NONE',  ( 6.988114217768294445, 34.63020833333332860, 26.07999730980477437 ) ) ;
#15890 = CARTESIAN_POINT ( 'NONE',  ( 10.37757302488624767, 25.72500000273120335, 31.93888565452638417 ) ) ;
#15891 = CARTESIAN_POINT ( 'NONE',  ( -33.58253175000000113, 75.02500000273117564, -10.91162601494193218 ) ) ;
#15892 = CARTESIAN_POINT ( 'NONE',  ( 6.486482029760649416E-15, 37.87500000273117706, 35.31076352940723240 ) ) ;
#15893 = CARTESIAN_POINT ( 'NONE',  ( 27.16883889988624290, 14.17500000273119731, 19.73931689729373673 ) ) ;
#15894 = CARTESIAN_POINT ( 'NONE',  ( -32.50000000000000000, 64.10000000000000853, 10.55989012756946366 ) ) ;
#15895 = CARTESIAN_POINT ( 'NONE',  ( -24.18731323226248264, 54.54465250092398776, -14.01125832528284931 ) ) ;
#15896 = CARTESIAN_POINT ( 'NONE',  ( -10.37757302488624411, 76.72500000273119269, -31.93888565452638417 ) ) ;
#15897 = ADVANCED_FACE ( 'NONE', ( #21833 ), #11683, .T. ) ;
#15898 = FACE_OUTER_BOUND ( 'NONE', #9944, .T. ) ;
#15899 = CARTESIAN_POINT ( 'NONE',  ( -2.092463501923844636E-15, 53.50000000000000000, -34.17252228774368916 ) ) ;
#15900 = CARTESIAN_POINT ( 'NONE',  ( 5.779280353836490358E-15, 26.50000000000000711, 32.49999999999999289 ) ) ;
#15901 = CARTESIAN_POINT ( 'NONE',  ( 6.486482029760648627E-15, 55.62500000273119838, 35.31076352940722529 ) ) ;
#15902 = CARTESIAN_POINT ( 'NONE',  ( 14.47279130897151589, 8.824999997268804464, 19.92008829642072953 ) ) ;
#15903 = EDGE_LOOP ( 'NONE', ( #15573, #25298, #22938, #11293 ) ) ;
#15904 = CARTESIAN_POINT ( 'NONE',  ( 27.16883889988623935, 74.57500000273118701, -19.73931689729374384 ) ) ;
#15905 = CARTESIAN_POINT ( 'NONE',  ( -26.29305231718578995, 62.20000000000001705, 19.10302069950538595 ) ) ;
#15906 = CARTESIAN_POINT ( 'NONE',  ( 7.236395654485760609, 1.024999997268821739, -22.27133577429736633 ) ) ;
#15907 = CARTESIAN_POINT ( 'NONE',  ( -0.04044903254992426173, 12.14881916759064140, 27.95245687107223276 ) ) ;
#15908 =( BOUNDED_CURVE ( )  B_SPLINE_CURVE ( 2, ( #30386, #1395, #14120, #11371, #6555, #9122, #27831, #1217, #22504, #29711, #22181, #24909, #32457 ),
 .UNSPECIFIED., .F., .F. ) 
 B_SPLINE_CURVE_WITH_KNOTS ( ( 3, 2, 2, 2, 2, 2, 3 ),
 ( 0.04487179487179487197, 0.04615384615384615641, 0.04871794871794871834, 0.05128205128205128027, 0.05384615384615384914, 0.05641025641025641107, 0.05769230769230769551 ),
 .UNSPECIFIED. ) 
 CURVE ( )  GEOMETRIC_REPRESENTATION_ITEM ( )  RATIONAL_B_SPLINE_CURVE ( ( 0.9755282581475768211, 0.9755282581475768211, 1.000000000000000000, 0.9510565162951535312, 1.000000000000000000, 0.9510565162951535312, 1.000000000000000000, 0.9510565162951535312, 1.000000000000000000, 0.9510565162951535312, 1.000000000000000000, 0.9755282581475767101, 0.9755282581475768211 ) ) 
 REPRESENTATION_ITEM ( '' )  );
#15909 = ORIENTED_EDGE ( 'NONE', *, *, #14536, .T. ) ;
#15910 = CARTESIAN_POINT ( 'NONE',  ( 20.75514604977248467, 40.42500000273117422, -28.56700777964554305 ) ) ;
#15911 = CARTESIAN_POINT ( 'NONE',  ( -10.04305231718578462, 16.90000000546237757, 30.90933677959249337 ) ) ;
#15912 = ORIENTED_EDGE ( 'NONE', *, *, #33259, .T. ) ;
#15913 = CARTESIAN_POINT ( 'NONE',  ( -15.01150461594642138, 46.51822916666666430, -26.00068869287340334 ) ) ;
#15914 = DIRECTION ( 'NONE',  ( -0.000000000000000000, -1.000000000000000000, -0.000000000000000000 ) ) ;
#15915 = CARTESIAN_POINT ( 'NONE',  ( -32.50000000000000000, 4.600000005462372421, 10.55989012756946366 ) ) ;
#15916 = CARTESIAN_POINT ( 'NONE',  ( -10.04305231718578462, 72.40000000000001990, 30.90933677959249337 ) ) ;
#15917 = CARTESIAN_POINT ( 'NONE',  ( -26.00068869287340334, 21.59635416666666785, 15.01150461594643382 ) ) ;
#15918 = CARTESIAN_POINT ( 'NONE',  ( 24.50000000000000355, 0.09999999999999684142, -7.960532557706203605 ) ) ;
#15919 = CARTESIAN_POINT ( 'NONE',  ( 33.58253175000000823, 12.27500000273116854, 10.91162601494192863 ) ) ;
#15920 = CARTESIAN_POINT ( 'NONE',  ( 20.08610463437158344, 62.69999999999999574, 27.64615127144129403 ) ) ;
#15921 = CARTESIAN_POINT ( 'NONE',  ( -13.91746824999999887, 80.87500000273118417, 0.000000000000000000 ) ) ;
#15922 = DIRECTION ( 'NONE',  ( 0.000000000000000000, 1.000000000000000000, 0.000000000000000000 ) ) ;
#15923 = CARTESIAN_POINT ( 'NONE',  ( 30.02300923189239867, 32.47618083240936215, -0.04044903255044467877 ) ) ;
#15924 = CARTESIAN_POINT ( 'NONE',  ( -8.601468415847518756, 79.07500000273121543, -11.83890561707634781 ) ) ;
#15925 = CARTESIAN_POINT ( 'NONE',  ( -20.50609665440969209, 42.07812499999999289, 20.50609665441005092 ) ) ;
#15926 = ITEM_DEFINED_TRANSFORMATION ( 'NONE', 'NONE', #18899,  #1376 ) ;
#15927 = DIRECTION ( 'NONE',  ( -1.224646799147353454E-16, 1.000000000000000000, -0.000000000000000000 ) ) ;
#15928 = CARTESIAN_POINT ( 'NONE',  ( 26.29305231718578995, 65.20000000000000284, -19.10302069950538240 ) ) ;
#15929 = CARTESIAN_POINT ( 'NONE',  ( 32.50000000000000000, 3.099999999999989875, -10.55989012756945833 ) ) ;
#15930 = CARTESIAN_POINT ( 'NONE',  ( 5.779280353836490358E-15, 35.00000000546238255, 32.49999999999999289 ) ) ;
#15931 = CARTESIAN_POINT ( 'NONE',  ( -7.025853678916861966, 58.97357666574269786, -26.06988505166722803 ) ) ;
#15932 = CARTESIAN_POINT ( 'NONE',  ( 6.486482029760649416E-15, 51.62500000273120548, 35.31076352940723240 ) ) ;
#15933 = CARTESIAN_POINT ( 'NONE',  ( -13.91746824999999887, 78.87500000273118417, 0.000000000000000000 ) ) ;
#15934 = CARTESIAN_POINT ( 'NONE',  ( -2.162160676586881955E-15, 54.87500000273119127, -35.31076352940723240 ) ) ;
#15935 = CARTESIAN_POINT ( 'NONE',  ( -27.16883889988623935, 31.57500000273119767, 19.73931689729374739 ) ) ;
#15936 = FACE_OUTER_BOUND ( 'NONE', #31831, .T. ) ;
#15937 = CARTESIAN_POINT ( 'NONE',  ( 2.584737979205442066E-13, 17.58593749999999645, 27.95245687107223276 ) ) ;
#15938 = CARTESIAN_POINT ( 'NONE',  ( 1.836970198721029589E-15, 16.99999999999998579, 15.00000000000000000 ) ) ;
#15939 = CARTESIAN_POINT ( 'NONE',  ( 26.29305231718578995, 51.70000000546237828, -19.10302069950538240 ) ) ;
#15940 = CARTESIAN_POINT ( 'NONE',  ( 26.29305231718578995, 71.20000000000000284, -19.10302069950538240 ) ) ;
#15941 = CARTESIAN_POINT ( 'NONE',  ( 20.75514604977249178, 13.82500000273117813, 28.56700777964553950 ) ) ;
#15942 = CARTESIAN_POINT ( 'NONE',  ( -7.236395654485757944, 1.224999997268799712, -22.27133577429736988 ) ) ;
#15943 = CARTESIAN_POINT ( 'NONE',  ( 24.50000000000000000, 1.749999994537621006, 0.000000000000000000 ) ) ;
#15944 = CARTESIAN_POINT ( 'NONE',  ( -7.025853678916861966, 21.16107666574269075, -26.06988505166722803 ) ) ;
#15945 = CARTESIAN_POINT ( 'NONE',  ( 20.08610463437158344, 35.20000000546237828, 27.64615127144129403 ) ) ;
#15946 = EDGE_CURVE ( 'NONE', #29890, #9461, #4760, .T. ) ;
#15947 = CARTESIAN_POINT ( 'NONE',  ( -32.50000000000000000, 12.00000000000001066, 0.000000000000000000 ) ) ;
#15948 = CARTESIAN_POINT ( 'NONE',  ( 33.58253175000000113, 26.22500000273119625, -10.91162601494193574 ) ) ;
#15949 = CARTESIAN_POINT ( 'NONE',  ( -19.09188309203660694, 45.51562500000000000, 19.09188309203694800 ) ) ;
#15950 = VERTEX_POINT ( 'NONE', #3631 ) ;
#15951 = CARTESIAN_POINT ( 'NONE',  ( 10.37757302488624767, 59.72500000273119269, 31.93888565452638417 ) ) ;
#15952 = ORIENTED_EDGE ( 'NONE', *, *, #5240, .F. ) ;
#15953 = CARTESIAN_POINT ( 'NONE',  ( -7.543491769121417612, 63.85454833425732346, 28.00173670424549499 ) ) ;
#15954 = CARTESIAN_POINT ( 'NONE',  ( -28.00173670424549499, 13.15142333425730925, -7.543491769121417612 ) ) ;
#15955 = CARTESIAN_POINT ( 'NONE',  ( -10.37757302488623701, 3.525000002731190740, 31.93888565452638417 ) ) ;
#15956 = VERTEX_POINT ( 'NONE', #1202 ) ;
#15957 = CARTESIAN_POINT ( 'NONE',  ( 0.000000000000000000, 80.00000000000001421, 0.000000000000000000 ) ) ;
#15958 = CARTESIAN_POINT ( 'NONE',  ( 33.58253175000000113, 36.37500000273119838, -4.112674001490185761E-15 ) ) ;
#15959 = CARTESIAN_POINT ( 'NONE',  ( 26.29305231718579350, 39.30000000546237970, 19.10302069950537529 ) ) ;
#15960 = CARTESIAN_POINT ( 'NONE',  ( 9.270509831248423538, 73.30000000000001137, -12.75976212528059861 ) ) ;
#15961 = CARTESIAN_POINT ( 'NONE',  ( 0.000000000000000000, 80.00000000000001421, -32.50000000000000000 ) ) ;
#15962 = CARTESIAN_POINT ( 'NONE',  ( 7.570916362186207671, 5.349999994537613546, 23.30088464923126779 ) ) ;
#15963 = CARTESIAN_POINT ( 'NONE',  ( 33.58253175000000823, 40.27500000273118985, 10.91162601494192863 ) ) ;
#15964 = SURFACE_STYLE_USAGE ( .BOTH. , #318 ) ;
#15965 = CARTESIAN_POINT ( 'NONE',  ( 32.50000000000000711, 20.90000000000000924, 10.55989012756945122 ) ) ;
#15966 = CARTESIAN_POINT ( 'NONE',  ( -32.50000000000000000, 19.99999999999998934, 0.000000000000000000 ) ) ;
#15967 = CARTESIAN_POINT ( 'NONE',  ( 24.50000000000000355, 5.899999999999987921, 7.960532557706212486 ) ) ;
#15968 = CARTESIAN_POINT ( 'NONE',  ( 33.58253175000000823, 72.02500000273118985, 10.91162601494192863 ) ) ;
#15969 = CARTESIAN_POINT ( 'NONE',  ( -7.570916362186215665, 3.149999994537633352, 23.30088464923126423 ) ) ;
#15970 = CARTESIAN_POINT ( 'NONE',  ( -20.08610463437157989, 37.70000000000000284, -27.64615127144129758 ) ) ;
#15971 = CARTESIAN_POINT ( 'NONE',  ( 10.37757302488624767, 51.97500000273119980, 31.93888565452638417 ) ) ;
#15972 = CARTESIAN_POINT ( 'NONE',  ( 5.147494310547426899, 7.948745723915522809, -32.50000000000000000 ) ) ;
#15973 = CARTESIAN_POINT ( 'NONE',  ( -33.58253175000000113, 11.22500000273120335, 10.91162601494193929 ) ) ;
#15974 = CARTESIAN_POINT ( 'NONE',  ( -0.04044903254992426173, 32.77381916759064495, 27.95245687107223276 ) ) ;
#15975 = CARTESIAN_POINT ( 'NONE',  ( -10.35455269120598132, 66.99999999999998579, -31.92933819309194732 ) ) ;
#15976 = CARTESIAN_POINT ( 'NONE',  ( -23.31009017153187202, 52.00000000000001421, 23.30172593756756427 ) ) ;
#15977 = CARTESIAN_POINT ( 'NONE',  ( 6.486482029760649416E-15, 37.62500000273118417, 35.31076352940723240 ) ) ;
#15978 = AXIS2_PLACEMENT_3D ( 'NONE', #11142, #3743, #21781 ) ;
#15980 = AXIS2_PLACEMENT_3D ( 'NONE', #26250, #17209, #6898 ) ;
#15979 = CARTESIAN_POINT ( 'NONE',  ( -10.04305231718578462, 64.90000000546237402, 30.90933677959249337 ) ) ;
#15981 = DIRECTION ( 'NONE',  ( 0.000000000000000000, 0.000000000000000000, 1.000000000000000000 ) ) ;
#15982 = CARTESIAN_POINT ( 'NONE',  ( -11.25946833292375793, 79.07500000273121543, 8.180482586598737171 ) ) ;
#15983 = CARTESIAN_POINT ( 'NONE',  ( 25.98046417659831775, 49.37722249907602645, -15.04653450569338879 ) ) ;
#15984 = CARTESIAN_POINT ( 'NONE',  ( -20.08610463437156923, 54.80000000546237260, 27.64615127144130113 ) ) ;
#15985 = EDGE_CURVE ( 'NONE', #30034, #32793, #29694, .T. ) ;
#15986 = CARTESIAN_POINT ( 'NONE',  ( 11.25946833292375793, 76.17500000273119554, 8.180482586598731842 ) ) ;
#15987 = CARTESIAN_POINT ( 'NONE',  ( -2.428612866367529427E-13, 15.86718749999999645, -27.95245687107222921 ) ) ;
#15988 = EDGE_CURVE ( 'NONE', #30053, #17164, #21995, .T. ) ;
#15989 = CARTESIAN_POINT ( 'NONE',  ( -32.50000000000000000, 72.50000000546236834, 0.000000000000000000 ) ) ;
#15990 = CARTESIAN_POINT ( 'NONE',  ( -20.50609665441004736, 25.74999999999999645, -20.50609665440969565 ) ) ;
#15991 = CARTESIAN_POINT ( 'NONE',  ( -10.37757302488623701, 27.77500000273118275, 31.93888565452638417 ) ) ;
#15992 = CARTESIAN_POINT ( 'NONE',  ( 18.94512977948575738, 16.92499999726882010, 13.76444248337723408 ) ) ;
#15993 = VERTEX_POINT ( 'NONE', #11515 ) ;
#15994 = CARTESIAN_POINT ( 'NONE',  ( -30.02300923189239867, 43.94569416759065206, -0.04044903254991731589 ) ) ;
#15995 = CARTESIAN_POINT ( 'NONE',  ( 32.50000000000000711, 15.40000000546236514, 10.55989012756945122 ) ) ;
#15996 = CARTESIAN_POINT ( 'NONE',  ( -26.00068869287368756, 49.66927083333330728, -15.01150461594595775 ) ) ;
#15997 = CARTESIAN_POINT ( 'NONE',  ( 26.29305231718579350, 74.80000000000001137, 19.10302069950537529 ) ) ;
#15998 = CARTESIAN_POINT ( 'NONE',  ( 27.16883889988623935, 54.57500000273118701, -19.73931689729374384 ) ) ;
#15999 = CARTESIAN_POINT ( 'NONE',  ( 32.50000000000000000, 53.60000000546238397, -10.55989012756945833 ) ) ;
#16000 = CARTESIAN_POINT ( 'NONE',  ( 8.601468415847516980, 76.67500000273118133, -11.83890561707634781 ) ) ;
#16001 = CARTESIAN_POINT ( 'NONE',  ( 33.58253175000000823, 36.02500000273117564, 10.91162601494192863 ) ) ;
#16002 = CARTESIAN_POINT ( 'NONE',  ( -15.00000000000000000, 76.25000000546239676, 0.000000000000000000 ) ) ;
#16003 = VECTOR ( 'NONE', #31976, 1000.000000000000000 ) ;
#16004 = CARTESIAN_POINT ( 'NONE',  ( -20.75514604977248823, 67.07500000273118701, -28.56700777964554305 ) ) ;
#16005 = CARTESIAN_POINT ( 'NONE',  ( 0.000000000000000000, 102.0000000000000284, 0.000000000000000000 ) ) ;
#16006 = CARTESIAN_POINT ( 'NONE',  ( -33.58253175000000113, 59.02500000273120406, -10.91162601494193041 ) ) ;
#16007 = CARTESIAN_POINT ( 'NONE',  ( -26.00068869287340334, 18.15885416666666075, 15.01150461594643559 ) ) ;
#16008 = CARTESIAN_POINT ( 'NONE',  ( 10.04305231718578817, 39.39999999999999147, -30.90933677959249337 ) ) ;
#16009 = CARTESIAN_POINT ( 'NONE',  ( -14.47279130897151589, 7.324999997268822227, -19.92008829642072598 ) ) ;
#16010 =( BOUNDED_CURVE ( )  B_SPLINE_CURVE ( 2, ( #22450, #9580, #12500, #20058, #9230, #30161, #1848, #30503, #27774, #7003, #14905, #22968, #6665 ),
 .UNSPECIFIED., .F., .T. ) 
 B_SPLINE_CURVE_WITH_KNOTS ( ( 3, 2, 2, 2, 2, 2, 3 ),
 ( 0.1858974358974359031, 0.1871794871794871806, 0.1897435897435897356, 0.1923076923076923184, 0.1948717948717948734, 0.1974358974358974284, 0.1987179487179487336 ),
 .UNSPECIFIED. ) 
 CURVE ( )  GEOMETRIC_REPRESENTATION_ITEM ( )  RATIONAL_B_SPLINE_CURVE ( ( 0.9755282581475768211, 0.9755282581475768211, 1.000000000000000000, 0.9510565162951535312, 1.000000000000000000, 0.9510565162951535312, 1.000000000000000000, 0.9510565162951535312, 1.000000000000000000, 0.9510565162951535312, 1.000000000000000000, 0.9755282581475764880, 0.9755282581475768211 ) ) 
 REPRESENTATION_ITEM ( '' )  );
#16011 = CARTESIAN_POINT ( 'NONE',  ( -33.58253175000000113, 11.47500000273119625, 10.91162601494193929 ) ) ;
#16012 = CARTESIAN_POINT ( 'NONE',  ( 24.50000000000000000, 19.64999999453763024, 7.960532557706212486 ) ) ;
#16013 = CARTESIAN_POINT ( 'NONE',  ( -19.11951029504797006, 38.06211833240934084, -19.06425588902558133 ) ) ;
#16014 = CARTESIAN_POINT ( 'NONE',  ( -11.25946833292375793, 71.57500000273120122, 8.180482586598737171 ) ) ;
#16015 = CARTESIAN_POINT ( 'NONE',  ( 33.58253175000000823, 70.27500000273118985, 10.91162601494192685 ) ) ;
#16016 = LINE ( 'NONE', #26470, #33564 ) ;
#16017 = CARTESIAN_POINT ( 'NONE',  ( -27.16883889988623935, 71.57500000273118701, 19.73931689729374739 ) ) ;
#16018 = VERTEX_POINT ( 'NONE', #29374 ) ;
#16019 = DIRECTION ( 'NONE',  ( 0.000000000000000000, 1.000000000000000000, 0.000000000000000000 ) ) ;
#16020 = CARTESIAN_POINT ( 'NONE',  ( 13.97622843553633665, 61.98697916666665009, 24.20753774853730889 ) ) ;
#16021 = CARTESIAN_POINT ( 'NONE',  ( 10.37757302488624056, 54.52500000273118275, -31.93888565452638417 ) ) ;
#16022 = CARTESIAN_POINT ( 'NONE',  ( -20.75514604977248112, 19.67500000273119909, 28.56700777964554661 ) ) ;
#16023 = CARTESIAN_POINT ( 'NONE',  ( 33.58253175000000113, 4.375000002731193938, -4.112674001490185761E-15 ) ) ;
#16024 = CARTESIAN_POINT ( 'NONE',  ( 24.20753774853756113, 37.63802083333331439, 13.97622843553589789 ) ) ;
#16025 = CARTESIAN_POINT ( 'NONE',  ( 28.02196122052045268, 28.33371500092397355, -7.468012846824774620 ) ) ;
#16026 = CARTESIAN_POINT ( 'NONE',  ( 30.02300923189239867, 22.16368083240936215, -0.04044903255044467877 ) ) ;
#16027 = CARTESIAN_POINT ( 'NONE',  ( -20.08610463437157989, 74.20000000546238539, -27.64615127144129758 ) ) ;
#16028 = CARTESIAN_POINT ( 'NONE',  ( 2.708425130540434544, 52.00000000000002842, -32.46185396738157891 ) ) ;
#16029 = CARTESIAN_POINT ( 'NONE',  ( 6.486482029760648627E-15, 39.62500000273117706, 35.31076352940722529 ) ) ;
#16030 = CARTESIAN_POINT ( 'NONE',  ( 19.11951029504797006, 50.09336833240935505, 19.06425588902558133 ) ) ;
#16031 = CARTESIAN_POINT ( 'NONE',  ( 23.41746825000000243, 14.52499999726882685, 7.608796670333735079 ) ) ;
#16032 = DIRECTION ( 'NONE',  ( 0.000000000000000000, 0.000000000000000000, -1.000000000000000000 ) ) ;
#16033 = VERTEX_POINT ( 'NONE', #6542 ) ;
#16034 = CARTESIAN_POINT ( 'NONE',  ( 10.37757302488624056, 50.77500000273120406, -31.93888565452638417 ) ) ;
#16035 = CARTESIAN_POINT ( 'NONE',  ( 15.00000000000000000, 77.10000000000000853, -4.873795443493596835 ) ) ;
#16036 = CARTESIAN_POINT ( 'NONE',  ( -14.01125832528285109, 53.68527750092398065, 24.18731323226248264 ) ) ;
#16037 = CARTESIAN_POINT ( 'NONE',  ( 10.37757302488624056, 68.77500000273117564, -31.93888565452638417 ) ) ;
#16038 = ORIENTED_EDGE ( 'NONE', *, *, #9244, .T. ) ;
#16039 = CARTESIAN_POINT ( 'NONE',  ( -10.37757302488624411, 18.72500000273118204, -31.93888565452638417 ) ) ;
#16040 = CARTESIAN_POINT ( 'NONE',  ( 15.01150461594596308, 23.02864583333332149, -26.00068869287367335 ) ) ;
#16041 = ORIENTED_EDGE ( 'NONE', *, *, #12835, .F. ) ;
#16042 = AXIS2_PLACEMENT_3D ( 'NONE', #30856, #7349, #4777 ) ;
#16043 = CARTESIAN_POINT ( 'NONE',  ( 20.08610463437157279, 65.80000000546237970, -27.64615127144129758 ) ) ;
#16044 = CARTESIAN_POINT ( 'NONE',  ( -33.58253175000000113, 61.22500000273118559, 10.91162601494193929 ) ) ;
#16045 = CARTESIAN_POINT ( 'NONE',  ( -28.01184896238304134, 46.08854166666666430, -7.505752307972844761 ) ) ;
#16046 = CARTESIAN_POINT ( 'NONE',  ( 20.08610463437158344, 17.20000000546236762, 27.64615127144129403 ) ) ;
#16047 = CARTESIAN_POINT ( 'NONE',  ( -32.50000000000000000, 66.50000000546238255, 0.000000000000000000 ) ) ;
#16048 = CARTESIAN_POINT ( 'NONE',  ( -7.236395654485757944, 7.724999997268805707, -22.27133577429736988 ) ) ;
#16049 = EDGE_CURVE ( 'NONE', #20206, #28550, #16680, .T. ) ;
#16050 = CARTESIAN_POINT ( 'NONE',  ( 6.486482029760649416E-15, 5.625000002731175286, 35.31076352940723240 ) ) ;
#16051 = CARTESIAN_POINT ( 'NONE',  ( 20.75514604977248467, 30.67500000273119909, -28.56700777964554305 ) ) ;
#16052 = CARTESIAN_POINT ( 'NONE',  ( -1.778240108872766143E-15, 63.50000000000000000, -32.49999999999999289 ) ) ;
#16053 = CARTESIAN_POINT ( 'NONE',  ( -30.02300923189239867, 65.13243083240935505, 0.04044903255044988294 ) ) ;
#16054 = FACE_OUTER_BOUND ( 'NONE', #19267, .T. ) ;
#16055 = CARTESIAN_POINT ( 'NONE',  ( -10.04305231718578462, 32.39999999999998437, 30.90933677959249337 ) ) ;
#16056 = CARTESIAN_POINT ( 'NONE',  ( -20.08610463437156923, 18.30000000000000782, 27.64615127144130113 ) ) ;
#16057 = CARTESIAN_POINT ( 'NONE',  ( -19.09188309203694445, 56.68749999999998579, -19.09188309203661049 ) ) ;
#16058 = CARTESIAN_POINT ( 'NONE',  ( -7.236395654485757944, 3.724999997268802154, -22.27133577429736988 ) ) ;
#16059 = CARTESIAN_POINT ( 'NONE',  ( 13.91746824999999532, 73.97500000273119269, -4.522059556121118540 ) ) ;
#16060 = CARTESIAN_POINT ( 'NONE',  ( -13.97622843553588901, 35.05989583333332860, 24.20753774853756823 ) ) ;
#16061 = CARTESIAN_POINT ( 'NONE',  ( -10.37757302488623701, 25.52500000273119696, 31.93888565452638417 ) ) ;
#16062 = CARTESIAN_POINT ( 'NONE',  ( -10.37757302488624411, 72.72500000273117848, -31.93888565452638417 ) ) ;
#16063 = CARTESIAN_POINT ( 'NONE',  ( -27.16883889988623935, 37.57500000273118701, 19.73931689729374739 ) ) ;
#16064 = CARTESIAN_POINT ( 'NONE',  ( 33.58253175000000113, 12.37500000273117351, -4.112674001490185761E-15 ) ) ;
#16065 = CARTESIAN_POINT ( 'NONE',  ( -27.95245687107223986, 54.25819416759065206, -0.04044903254993292840 ) ) ;
#16066 = CARTESIAN_POINT ( 'NONE',  ( 33.58253175000000113, 70.12500000273119838, -4.112674001490185761E-15 ) ) ;
#16067 = CARTESIAN_POINT ( 'NONE',  ( -1.778240108872766143E-15, 4.000000005462373664, -32.49999999999999289 ) ) ;
#16068 = AXIS2_PLACEMENT_3D ( 'NONE', #20446, #30896, #17875 ) ;
#16069 = CARTESIAN_POINT ( 'NONE',  ( 32.50000000000000000, 55.00000000000000711, -3.980102097228898626E-15 ) ) ;
#16070 = CARTESIAN_POINT ( 'NONE',  ( 9.270509831248425314, 78.95000000546239960, 12.75976212528059683 ) ) ;
#16071 = CARTESIAN_POINT ( 'NONE',  ( -2.162160676586882350E-15, 60.62500000273118417, -35.31076352940722529 ) ) ;
#16072 = AXIS2_PLACEMENT_3D ( 'NONE', #4708, #20514, #7279 ) ;
#16073 = CARTESIAN_POINT ( 'NONE',  ( 23.41746825000000243, 15.22499999726880482, -7.608796670333727974 ) ) ;
#16074 = ORIENTED_EDGE ( 'NONE', *, *, #11926, .F. ) ;
#16075 = CARTESIAN_POINT ( 'NONE',  ( 20.75514604977248467, 68.67500000273119554, -28.56700777964554305 ) ) ;
#16076 = CARTESIAN_POINT ( 'NONE',  ( -10.04305231718578462, 62.39999999999999858, 30.90933677959249337 ) ) ;
#16077 = CARTESIAN_POINT ( 'NONE',  ( -7.236395654485763274, 2.024999997268822405, 22.27133577429736633 ) ) ;
#16078 = CARTESIAN_POINT ( 'NONE',  ( 6.950374756619721595, 15.44309000092397355, 26.09010956794232428 ) ) ;
#16079 = ADVANCED_FACE ( 'NONE', ( #11852 ), #32611, .T. ) ;
#16080 = ORIENTED_EDGE ( 'NONE', *, *, #15561, .T. ) ;
#16081 = CARTESIAN_POINT ( 'NONE',  ( 10.37757302488624056, 42.52500000273119696, -31.93888565452638417 ) ) ;
#16082 = CARTESIAN_POINT ( 'NONE',  ( -10.04305231718578462, 42.90000000546237402, 30.90933677959249337 ) ) ;
#16083 = VERTEX_POINT ( 'NONE', #17015 ) ;
#16084 = CARTESIAN_POINT ( 'NONE',  ( -15.01150461594595775, 38.49739583333332860, 26.00068869287368756 ) ) ;
#16085 = CARTESIAN_POINT ( 'NONE',  ( 10.37757302488624056, 66.77500000273118985, -31.93888565452638417 ) ) ;
#16086 = CARTESIAN_POINT ( 'NONE',  ( 20.08610463437158344, 5.200000005462368513, 27.64615127144129403 ) ) ;
#16087 = DIRECTION ( 'NONE',  ( 0.000000000000000000, 1.000000000000000000, 0.000000000000000000 ) ) ;
#16088 = CARTESIAN_POINT ( 'NONE',  ( -7.505752307972844761, 21.16666666666666430, 28.01184896238304134 ) ) ;
#16089 = EDGE_CURVE ( 'NONE', #20029, #25648, #27762, .T. ) ;
#16090 = EDGE_CURVE ( 'NONE', #1393, #4913, #19422, .T. ) ;
#16091 = CARTESIAN_POINT ( 'NONE',  ( 18.94512977948576093, 16.82499999726880091, -13.76444248337722875 ) ) ;
#16092 = CARTESIAN_POINT ( 'NONE',  ( 10.37757302488624056, 8.775000002731180970, -31.93888565452638417 ) ) ;
#16093 = CARTESIAN_POINT ( 'NONE',  ( 32.50000000000000000, 59.00000000000000000, -3.980102097228898626E-15 ) ) ;
#16094 = CARTESIAN_POINT ( 'NONE',  ( 11.25946833292375793, 79.67500000273119554, 8.180482586598731842 ) ) ;
#16095 = FACE_OUTER_BOUND ( 'NONE', #2279, .T. ) ;
#16096 = CARTESIAN_POINT ( 'NONE',  ( -0.04044903255044120238, 35.05430583240935505, -30.02300923189239867 ) ) ;
#16097 = CARTESIAN_POINT ( 'NONE',  ( -8.960552108402742093E-16, 74.87500000273116996, -14.63369212191046387 ) ) ;
#16098 = CARTESIAN_POINT ( 'NONE',  ( -7.505752307973343918, 50.09895833333332860, -28.01184896238290989 ) ) ;
#16099 = EDGE_CURVE ( 'NONE', #16699, #8792, #9683, .T. ) ;
#16100 = CARTESIAN_POINT ( 'NONE',  ( 3.469446951953614189E-15, -45.00000000000000000, 0.000000000000000000 ) ) ;
#16101 = CARTESIAN_POINT ( 'NONE',  ( -24.50000000000000000, -29.78157438140398838, 0.000000000000000000 ) ) ;
#16102 = CARTESIAN_POINT ( 'NONE',  ( 26.29305231718579350, 2.799999999999997158, 19.10302069950537529 ) ) ;
#16103 = DIRECTION ( 'NONE',  ( 0.000000000000000000, 0.000000000000000000, 1.000000000000000000 ) ) ;
#16104 = CARTESIAN_POINT ( 'NONE',  ( 6.950374756619257965, 59.26003499907601935, -26.09010956794244507 ) ) ;
#16105 = CARTESIAN_POINT ( 'NONE',  ( -27.16883889988624290, 40.92500000273119554, -19.73931689729374028 ) ) ;
#16106 = CARTESIAN_POINT ( 'NONE',  ( -4.300734207923755825, 79.27500000273118985, 13.23629886949340673 ) ) ;
#16107 = CARTESIAN_POINT ( 'NONE',  ( 10.37757302488624767, 55.97500000273118559, 31.93888565452638417 ) ) ;
#16108 = CARTESIAN_POINT ( 'NONE',  ( -33.58253175000000113, 33.37500000273119127, 0.000000000000000000 ) ) ;
#16109 = LINE ( 'NONE', #21255, #31951 ) ;
#16110 = CARTESIAN_POINT ( 'NONE',  ( -6.988114217768288228, 26.03645833333333215, -26.07999730980477437 ) ) ;
#16111 = CARTESIAN_POINT ( 'NONE',  ( -11.45223628611452504, -57.99999999999999289, 0.000000000000000000 ) ) ;
#16112 = CARTESIAN_POINT ( 'NONE',  ( -2.375766604868045029, 75.55125428154684641, -14.99999999999999822 ) ) ;
#16113 = CARTESIAN_POINT ( 'NONE',  ( 32.50000000000000000, 75.09999999999999432, -10.55989012756945833 ) ) ;
#16114 = CARTESIAN_POINT ( 'NONE',  ( 27.16883889988624290, 9.925000002731207971, 19.73931689729373673 ) ) ;
#16115 = CARTESIAN_POINT ( 'NONE',  ( 7.236395654485760609, 3.024999997268823293, -22.27133577429736633 ) ) ;
#16116 = CARTESIAN_POINT ( 'NONE',  ( -7.025853678916861966, 24.59857666574268720, -26.06988505166722803 ) ) ;
#16117 = DIRECTION ( 'NONE',  ( -0.8660254037844402619, 0.4999999999999970579, -0.000000000000000000 ) ) ;
#16118 = CARTESIAN_POINT ( 'NONE',  ( 10.37757302488624056, 22.52500000273119340, -31.93888565452638417 ) ) ;
#16119 = CARTESIAN_POINT ( 'NONE',  ( -26.07999730980477437, 45.80208333333333570, 6.988114217768305103 ) ) ;
#16120 = AXIS2_PLACEMENT_3D ( 'NONE', #9234, #9928, #6669 ) ;
#16121 = VERTEX_POINT ( 'NONE', #26807 ) ;
#16122 = CARTESIAN_POINT ( 'NONE',  ( -20.75514604977248112, 63.42500000273118133, 28.56700777964554661 ) ) ;
#16123 = VERTEX_POINT ( 'NONE', #3302 ) ;
#16124 = CARTESIAN_POINT ( 'NONE',  ( 7.505752307972854531, 16.01041666666666075, -28.01184896238303423 ) ) ;
#16125 = CARTESIAN_POINT ( 'NONE',  ( -28.00173670424549499, 16.58892333425730570, -7.543491769121417612 ) ) ;
#16126 = CARTESIAN_POINT ( 'NONE',  ( 6.486482029760649416E-15, 7.625000002731185056, 35.31076352940723240 ) ) ;
#16127 = ORIENTED_EDGE ( 'NONE', *, *, #29282, .T. ) ;
#16128 = CARTESIAN_POINT ( 'NONE',  ( 3.469446951953614189E-15, -45.00000000000000000, 0.000000000000000000 ) ) ;
#16129 = CARTESIAN_POINT ( 'NONE',  ( 20.75514604977249178, 26.07500000273119767, 28.56700777964553950 ) ) ;
#16130 = CARTESIAN_POINT ( 'NONE',  ( 32.50000000000000711, 37.40000000546236691, 10.55989012756945122 ) ) ;
#16131 = CARTESIAN_POINT ( 'NONE',  ( -26.29305231718579350, 75.80000000000001137, -19.10302069950537884 ) ) ;
#16132 = CARTESIAN_POINT ( 'NONE',  ( 26.29305231718578995, 33.70000000546238539, -19.10302069950538240 ) ) ;
#16133 = CARTESIAN_POINT ( 'NONE',  ( 32.50000000000000711, 76.89999999999999147, 10.55989012756945122 ) ) ;
#16134 = CARTESIAN_POINT ( 'NONE',  ( 10.37757302488624767, 43.97500000273119269, 31.93888565452638417 ) ) ;
#16135 = FILL_AREA_STYLE_COLOUR ( '', #17246 ) ;
#16136 = CARTESIAN_POINT ( 'NONE',  ( -32.50000000000000000, 24.00000000000000711, 0.000000000000000000 ) ) ;
#16137 = CARTESIAN_POINT ( 'NONE',  ( -26.29305231718579350, 21.79999999999998650, -19.10302069950537884 ) ) ;
#16138 = CARTESIAN_POINT ( 'NONE',  ( 1.577395562988744260E-15, 6.499999999999998224, -25.76082449383753925 ) ) ;
#16139 = CARTESIAN_POINT ( 'NONE',  ( 6.486482029760649416E-15, 63.62500000273117706, 35.31076352940723240 ) ) ;
#16140 = CARTESIAN_POINT ( 'NONE',  ( -32.50000000000000000, 78.00000000000001421, 0.000000000000000000 ) ) ;
#16141 = VECTOR ( 'NONE', #8565, 1000.000000000000000 ) ;
#16142 = CARTESIAN_POINT ( 'NONE',  ( -32.50000000000000000, 76.50000000546236834, 0.000000000000000000 ) ) ;
#16143 = CARTESIAN_POINT ( 'NONE',  ( 33.58253175000000113, 52.47500000273117848, -10.91162601494193574 ) ) ;
#16144 = CARTESIAN_POINT ( 'NONE',  ( 1.507698388325705758E-15, 5.124999997268805174, -24.62258325217400312 ) ) ;
#16145 = CARTESIAN_POINT ( 'NONE',  ( 15.14183272437242067, 3.699999999999999289, 20.84094480462498211 ) ) ;
#16146 = CARTESIAN_POINT ( 'NONE',  ( 10.37757302488624056, 10.52500000273118275, -31.93888565452638417 ) ) ;
#16147 = CARTESIAN_POINT ( 'NONE',  ( 7.025853678916403666, 31.19829833425730570, -26.06988505166735237 ) ) ;
#16148 = CARTESIAN_POINT ( 'NONE',  ( 7.570916362186213000, 2.149999994537632464, -23.30088464923126423 ) ) ;
#16149 = CARTESIAN_POINT ( 'NONE',  ( 10.35455269120621047, 52.00000000000001421, 31.92933819309184429 ) ) ;
#16150 = CARTESIAN_POINT ( 'NONE',  ( -33.58253175000000113, 35.12500000273117706, 0.000000000000000000 ) ) ;
#16151 = CARTESIAN_POINT ( 'NONE',  ( -5.147494310547322094, 56.05125428700920764, -32.50000000000003553 ) ) ;
#16152 = DIRECTION ( 'NONE',  ( -1.000000000000000000, 0.000000000000000000, 0.000000000000000000 ) ) ;
#16153 = CARTESIAN_POINT ( 'NONE',  ( 4.300734207923761154, 75.47500000273116427, 13.23629886949340495 ) ) ;
#16154 = CARTESIAN_POINT ( 'NONE',  ( 7.468012846824281681, 45.51003499907601935, -28.02196122052058058 ) ) ;
#16155 = CARTESIAN_POINT ( 'NONE',  ( 6.277390505771533514E-15, 57.00000000546238965, 34.17252228774368916 ) ) ;
#16156 = DIRECTION ( 'NONE',  ( -1.000000000000000000, 0.000000000000000000, 0.000000000000000000 ) ) ;
#16157 = CARTESIAN_POINT ( 'NONE',  ( 13.97622843553589966, 16.15364583333333215, -24.20753774853756113 ) ) ;
#16158 = CARTESIAN_POINT ( 'NONE',  ( 20.08610463437158344, 69.20000000546235697, 27.64615127144129403 ) ) ;
#16159 = CARTESIAN_POINT ( 'NONE',  ( 26.00068869287340334, 23.31510416666666430, -15.01150461594642316 ) ) ;
#16160 = CARTESIAN_POINT ( 'NONE',  ( -33.58253175000000113, 29.37500000273117351, 0.000000000000000000 ) ) ;
#16161 = CARTESIAN_POINT ( 'NONE',  ( -14.47279130897151767, 13.82499999726882045, -19.92008829642072598 ) ) ;
#16162 = ORIENTED_EDGE ( 'NONE', *, *, #29484, .F. ) ;
#16163 = CARTESIAN_POINT ( 'NONE',  ( 15.04653450569292872, 41.65402750092398065, -25.98046417659857710 ) ) ;
#16164 = CARTESIAN_POINT ( 'NONE',  ( -32.50000000000000000, 18.50000000546238255, 0.000000000000000000 ) ) ;
#16165 = CARTESIAN_POINT ( 'NONE',  ( 7.505752307973351023, 55.25520833333333570, 28.01184896238290278 ) ) ;
#16166 = CARTESIAN_POINT ( 'NONE',  ( -26.29305231718578995, 36.20000000000000995, 19.10302069950538595 ) ) ;
#16167 = CARTESIAN_POINT ( 'NONE',  ( -10.37757302488624411, 46.97500000273119269, -31.93888565452638417 ) ) ;
#16168 = CARTESIAN_POINT ( 'NONE',  ( -10.04305231718579172, 56.10000000546239107, -30.90933677959248982 ) ) ;
#16169 = CARTESIAN_POINT ( 'NONE',  ( 4.300734207923761154, 75.97500000273122112, 13.23629886949340495 ) ) ;
#16170 = CARTESIAN_POINT ( 'NONE',  ( -33.58253175000000113, 35.22500000273119980, 10.91162601494193929 ) ) ;
#16171 = CARTESIAN_POINT ( 'NONE',  ( -9.270509831248423538, 75.95000000546239960, -12.75976212528059861 ) ) ;
#16172 = CARTESIAN_POINT ( 'NONE',  ( 33.58253175000000113, 62.47500000273118559, -10.91162601494193751 ) ) ;
#16173 = CARTESIAN_POINT ( 'NONE',  ( 7.313012447739250820E-14, 13.24999999453762456, 24.50000000000000000 ) ) ;
#16174 = CARTESIAN_POINT ( 'NONE',  ( 31.04172217648528687, 52.00000000000000711, 12.81397374188273908 ) ) ;
#16175 = CARTESIAN_POINT ( 'NONE',  ( 20.50609665440969565, 23.17187499999999289, -20.50609665441004736 ) ) ;
#16176 = CARTESIAN_POINT ( 'NONE',  ( -32.50000000000000000, 42.00000000000000711, 0.000000000000000000 ) ) ;
#16177 = CARTESIAN_POINT ( 'NONE',  ( 23.41746825000000243, 4.524999997268823293, 7.608796670333735079 ) ) ;
#16178 = EDGE_CURVE ( 'NONE', #6976, #18620, #12978, .T. ) ;
#16179 = CARTESIAN_POINT ( 'NONE',  ( 20.75514604977249178, 6.075000002731190563, 28.56700777964553950 ) ) ;
#16180 = CARTESIAN_POINT ( 'NONE',  ( -5.485892052525789174E-07, 66.99999999999998579, 32.49999999999999289 ) ) ;
#16181 = DIRECTION ( 'NONE',  ( 0.000000000000000000, 1.000000000000000000, 0.000000000000000000 ) ) ;
#16182 = CARTESIAN_POINT ( 'NONE',  ( 33.58253175000000823, 74.27500000273118985, 10.91162601494192685 ) ) ;
#16183 = CARTESIAN_POINT ( 'NONE',  ( 0.000000000000000000, 80.00000000000001421, 0.000000000000000000 ) ) ;
#16184 = ADVANCED_FACE ( 'NONE', ( #11355 ), #11882, .T. ) ;
#16185 = CARTESIAN_POINT ( 'NONE',  ( -33.58253175000000113, 71.37500000273121259, 0.000000000000000000 ) ) ;
#16186 = ORIENTED_EDGE ( 'NONE', *, *, #24194, .F. ) ;
#16187 = DIRECTION ( 'NONE',  ( 0.000000000000000000, 0.000000000000000000, 1.000000000000000000 ) ) ;
#16188 = AXIS2_PLACEMENT_3D ( 'NONE', #24331, #3727, #806 ) ;
#16189 = CARTESIAN_POINT ( 'NONE',  ( 6.988114217767829928, 64.13541666666667140, -26.07999730980489872 ) ) ;
#16190 = CARTESIAN_POINT ( 'NONE',  ( 6.486482029760649416E-15, 51.62500000273120548, 35.31076352940723240 ) ) ;
#16191 = CARTESIAN_POINT ( 'NONE',  ( 20.75514604977249178, 12.07500000273119234, 28.56700777964553950 ) ) ;
#16192 = CARTESIAN_POINT ( 'NONE',  ( 20.75514604977248467, 4.675000002731191096, -28.56700777964554305 ) ) ;
#16193 = CARTESIAN_POINT ( 'NONE',  ( -26.07999730980477437, 38.92708333333333570, 6.988114217768305103 ) ) ;
#16194 = CARTESIAN_POINT ( 'NONE',  ( -26.02091320914849959, 26.47173583425730925, 14.97647472619947528 ) ) ;
#16195 = CARTESIAN_POINT ( 'NONE',  ( -7.543491769121917656, 21.16107666574269075, -28.00173670424536354 ) ) ;
#16196 = CARTESIAN_POINT ( 'NONE',  ( 20.08610463437158344, 73.20000000546235697, 27.64615127144129403 ) ) ;
#16197 = CARTESIAN_POINT ( 'NONE',  ( 24.23786831611837655, 51.99999999999999289, -22.37122307655969067 ) ) ;
#16198 = CARTESIAN_POINT ( 'NONE',  ( 10.37757302488624056, 38.52500000273118275, -31.93888565452638417 ) ) ;
#16199 = CARTESIAN_POINT ( 'NONE',  ( -27.95245687107223986, 47.94493083240935505, 0.04044903255043252877 ) ) ;
#16200 = CARTESIAN_POINT ( 'NONE',  ( 23.41746824999999887, 12.62499999726882116, 0.000000000000000000 ) ) ;
#16201 = CARTESIAN_POINT ( 'NONE',  ( 0.000000000000000000, -23.00000000000000000, 0.000000000000000000 ) ) ;
#16202 = ORIENTED_EDGE ( 'NONE', *, *, #32222, .F. ) ;
#16203 = CARTESIAN_POINT ( 'NONE',  ( -10.37757302488623701, 45.77500000273119696, 31.93888565452638417 ) ) ;
#16204 = CARTESIAN_POINT ( 'NONE',  ( -5.147494310547430452, 50.05125428700922185, -32.49999999999999289 ) ) ;
#16205 = CARTESIAN_POINT ( 'NONE',  ( 19.06425588902592239, 52.96913166759063785, 19.11951029504763611 ) ) ;
#16206 = CARTESIAN_POINT ( 'NONE',  ( 20.75514604977249178, 70.07500000273120122, 28.56700777964553950 ) ) ;
#16207 = ORIENTED_EDGE ( 'NONE', *, *, #26245, .F. ) ;
#16208 = CARTESIAN_POINT ( 'NONE',  ( -33.58253175000000113, 19.12500000273119483, 0.000000000000000000 ) ) ;
#16209 = CARTESIAN_POINT ( 'NONE',  ( -26.00068869287340334, 21.59635416666666785, 15.01150461594643382 ) ) ;
#16210 =( GEOMETRIC_REPRESENTATION_CONTEXT ( 3 ) GLOBAL_UNCERTAINTY_ASSIGNED_CONTEXT ( ( #14064 ) ) GLOBAL_UNIT_ASSIGNED_CONTEXT ( ( #361, #21982, #29858 ) ) REPRESENTATION_CONTEXT ( 'NONE', 'WORKASPACE' ) );
#16211 = ORIENTED_EDGE ( 'NONE', *, *, #29912, .T. ) ;
#16212 =( BOUNDED_CURVE ( )  B_SPLINE_CURVE ( 2, ( #21775, #26906, #29975, #14208, #19363, #32548, #32383, #16785, #14542, #27578, #29472, #4067, #815 ),
 .UNSPECIFIED., .F., .T. ) 
 B_SPLINE_CURVE_WITH_KNOTS ( ( 3, 2, 2, 2, 2, 2, 3 ),
 ( 0.8910256410256410797, 0.8923076923076923572, 0.8948717948717949122, 0.8974358974358974672, 0.9000000000000000222, 0.9025641025641025772, 0.9038461538461538547 ),
 .UNSPECIFIED. ) 
 CURVE ( )  GEOMETRIC_REPRESENTATION_ITEM ( )  RATIONAL_B_SPLINE_CURVE ( ( 0.9755282581475768211, 0.9755282581475778203, 1.000000000000000000, 0.9510565162951535312, 1.000000000000000000, 0.9510565162951535312, 1.000000000000000000, 0.9510565162951535312, 1.000000000000000000, 0.9510565162951535312, 1.000000000000000000, 0.9755282581475768211, 0.9755282581475768211 ) ) 
 REPRESENTATION_ITEM ( '' )  );
#16213 = CARTESIAN_POINT ( 'NONE',  ( -14.45873412499999944, 80.56250000409676204, 0.000000000000000000 ) ) ;
#16214 = CARTESIAN_POINT ( 'NONE',  ( 6.486482029760649416E-15, 55.62500000273119838, 35.31076352940723240 ) ) ;
#16215 = CARTESIAN_POINT ( 'NONE',  ( 2.740863092043355209E-13, 45.08593750000000711, 30.02300923189239512 ) ) ;
#16216 = CARTESIAN_POINT ( 'NONE',  ( 20.08610463437157279, 15.80000000546238326, -27.64615127144129758 ) ) ;
#16217 = DIRECTION ( 'NONE',  ( -0.000000000000000000, -1.000000000000000000, -0.000000000000000000 ) ) ;
#16218 = CARTESIAN_POINT ( 'NONE',  ( 7.236395654485755280, 10.72499999726880837, 22.27133577429736988 ) ) ;
#16219 = CARTESIAN_POINT ( 'NONE',  ( 20.75514604977249178, 32.07500000273117990, 28.56700777964553950 ) ) ;
#16220 = DIRECTION ( 'NONE',  ( -0.000000000000000000, 1.000000000000000000, -0.000000000000000000 ) ) ;
#16221 = CARTESIAN_POINT ( 'NONE',  ( -7.543491769121917656, 65.84857666574268364, -28.00173670424536354 ) ) ;
#16222 = CARTESIAN_POINT ( 'NONE',  ( -4.405589869732278832E-13, 32.49999999999997868, 32.50000000000000000 ) ) ;
#16223 = AXIS2_PLACEMENT_3D ( 'NONE', #25504, #4221, #12281 ) ;
#16224 = CARTESIAN_POINT ( 'NONE',  ( 2.489536152421872915E-14, 76.00000000546238255, -32.49999999999999289 ) ) ;
#16225 = CARTESIAN_POINT ( 'NONE',  ( 6.277390505771533514E-15, 8.499999999999992895, 34.17252228774368916 ) ) ;
#16226 = CARTESIAN_POINT ( 'NONE',  ( 26.07999730980477437, 61.27083333333332860, -6.988114217768290004 ) ) ;
#16227 = CARTESIAN_POINT ( 'NONE',  ( 24.50000000000000355, 19.64999999453763024, 7.960532557706212486 ) ) ;
#16228 = CARTESIAN_POINT ( 'NONE',  ( 4.300734207923757602, 76.27500000273118985, -13.23629886949340673 ) ) ;
#16229 = CARTESIAN_POINT ( 'NONE',  ( -24.20753774853756823, 35.91927083333332860, -13.97622843553588723 ) ) ;
#16230 = CARTESIAN_POINT ( 'NONE',  ( -27.16883889988623935, 25.32500000273119056, 19.73931689729374739 ) ) ;
#16231 = CARTESIAN_POINT ( 'NONE',  ( -33.58253175000000113, 75.12500000273118417, 0.000000000000000000 ) ) ;
#16232 = CARTESIAN_POINT ( 'NONE',  ( -20.75514604977248112, 37.67500000273118133, 28.56700777964554661 ) ) ;
#16233 = CARTESIAN_POINT ( 'NONE',  ( -20.75514604977248823, 17.07500000273119412, -28.56700777964554305 ) ) ;
#16234 = CARTESIAN_POINT ( 'NONE',  ( 19.11951029504763611, 58.98475666759065206, -19.06425588902591173 ) ) ;
#16235 = CARTESIAN_POINT ( 'NONE',  ( 33.58253175000000823, 68.02500000273117564, 10.91162601494192685 ) ) ;
#16236 = FACE_OUTER_BOUND ( 'NONE', #224, .T. ) ;
#16237 = CARTESIAN_POINT ( 'NONE',  ( -32.50000000000000000, 54.10000000000000853, 10.55989012756946366 ) ) ;
#16238 = CARTESIAN_POINT ( 'NONE',  ( 20.75514604977248467, 56.42500000273120264, -28.56700777964554305 ) ) ;
#16239 = CARTESIAN_POINT ( 'NONE',  ( -14.47279130897152122, 16.42499999726882365, 19.92008829642072243 ) ) ;
#16240 = ORIENTED_EDGE ( 'NONE', *, *, #7756, .T. ) ;
#16241 = CARTESIAN_POINT ( 'NONE',  ( 27.16883889988623935, 68.57500000273118701, -19.73931689729374384 ) ) ;
#16242 = CARTESIAN_POINT ( 'NONE',  ( 33.58253175000000823, 2.025000002731202287, 10.91162601494192685 ) ) ;
#16243 = VECTOR ( 'NONE', #4169, 1000.000000000000227 ) ;
#16244 = CARTESIAN_POINT ( 'NONE',  ( -23.41746825000000598, 3.724999997268819918, 7.608796670333726198 ) ) ;
#16245 = CARTESIAN_POINT ( 'NONE',  ( -24.18731323226248264, 27.04465250092397000, -14.01125832528284931 ) ) ;
#16246 = ORIENTED_EDGE ( 'NONE', *, *, #27184, .F. ) ;
#16247 = CARTESIAN_POINT ( 'NONE',  ( 27.16883889988624290, 35.92500000273117422, 19.73931689729373673 ) ) ;
#16248 = DIRECTION ( 'NONE',  ( -0.7202789989107549751, -0.6936844842780617304, 8.820873705091161919E-17 ) ) ;
#16249 = ORIENTED_EDGE ( 'NONE', *, *, #23732, .T. ) ;
#16250 = CARTESIAN_POINT ( 'NONE',  ( 2.740863092043355209E-13, 55.39843749999999289, 30.02300923189239512 ) ) ;
#16251 = CARTESIAN_POINT ( 'NONE',  ( -4.223320258572819786E-15, 17.50000000000000000, 24.50000000000000000 ) ) ;
#16252 = CARTESIAN_POINT ( 'NONE',  ( -19.82091636218621389, 3.200000000000008171, 14.40073868116558842 ) ) ;
#16253 = CARTESIAN_POINT ( 'NONE',  ( -27.16883889988623935, 75.32500000273117280, 19.73931689729374739 ) ) ;
#16254 = CARTESIAN_POINT ( 'NONE',  ( 30.02300923189239512, 20.16406249999999645, -2.619432448724977703E-13 ) ) ;
#16255 = CARTESIAN_POINT ( 'NONE',  ( -24.50000000000000000, 1.000000000000000888, -3.000384657911015469E-15 ) ) ;
#16256 = CARTESIAN_POINT ( 'NONE',  ( 27.16883889988624290, 8.175000002731191984, 19.73931689729373673 ) ) ;
#16257 = CARTESIAN_POINT ( 'NONE',  ( 33.58253175000000823, 26.02500000273120406, 10.91162601494192863 ) ) ;
#16258 = CARTESIAN_POINT ( 'NONE',  ( 13.91746824999999887, 79.87500000273118417, -1.704398294459741270E-15 ) ) ;
#16259 = CARTESIAN_POINT ( 'NONE',  ( 7.890940483122900408E-14, 18.24999999453761745, -24.50000000000000000 ) ) ;
#16260 = CARTESIAN_POINT ( 'NONE',  ( -30.02300923189239867, 37.63243083240935505, 0.04044903255044988294 ) ) ;
#16261 = CARTESIAN_POINT ( 'NONE',  ( 8.601468415847520532, 74.07500000273120122, 11.83890561707634781 ) ) ;
#16262 = CARTESIAN_POINT ( 'NONE',  ( -15.01150461594595775, 48.80989583333332860, 26.00068869287368756 ) ) ;
#16263 = PRODUCT_DEFINITION ( 'UNKNOWN', '', #6596, #29493 ) ;
#16264 = CARTESIAN_POINT ( 'NONE',  ( -19.82091636218621034, 10.80000000000000426, -14.40073868116559552 ) ) ;
#16265 = CARTESIAN_POINT ( 'NONE',  ( 5.147494310547408247, 70.55125428154684641, 32.50000000000000711 ) ) ;
#16266 = CARTESIAN_POINT ( 'NONE',  ( 26.09010956794244507, 63.55690999907603356, 6.950374756619249084 ) ) ;
#16267 = CARTESIAN_POINT ( 'NONE',  ( 20.75514604977248467, 42.42500000273117422, -28.56700777964554305 ) ) ;
#16268 = CARTESIAN_POINT ( 'NONE',  ( 11.25946833292375793, 80.07500000273121543, -8.180482586598735395 ) ) ;
#16269 = CARTESIAN_POINT ( 'NONE',  ( 27.16883889988624290, 54.17500000273118843, 19.73931689729373673 ) ) ;
#16270 = CARTESIAN_POINT ( 'NONE',  ( -20.75514604977248823, 33.07500000273118701, -28.56700777964554305 ) ) ;
#16271 = CARTESIAN_POINT ( 'NONE',  ( 13.39151655733673607, 16.99999999999997158, 19.69815938956502066 ) ) ;
#16272 = CARTESIAN_POINT ( 'NONE',  ( 24.20753774853731244, 26.75260416666666075, -13.97622843553633132 ) ) ;
#16273 = CARTESIAN_POINT ( 'NONE',  ( 0.000000000000000000, 3.673940397442059967E-15, -30.00000000000000000 ) ) ;
#16274 = AXIS2_PLACEMENT_3D ( 'NONE', #3963, #11194, #24892 ) ;
#16275 = CARTESIAN_POINT ( 'NONE',  ( 20.08610463437157279, 31.30000000000000071, -27.64615127144129758 ) ) ;
#16276 = CARTESIAN_POINT ( 'NONE',  ( 10.04305231718578817, 73.40000000000000568, -30.90933677959249337 ) ) ;
#16277 = CARTESIAN_POINT ( 'NONE',  ( 33.58253175000000113, 12.22500000273118381, -10.91162601494193751 ) ) ;
#16278 = CARTESIAN_POINT ( 'NONE',  ( 14.47279130897151944, 4.924999997268811214, -19.92008829642072598 ) ) ;
#16279 = CARTESIAN_POINT ( 'NONE',  ( -32.50000000000000000, 52.60000000546235555, 10.55989012756946366 ) ) ;
#16280 = CARTESIAN_POINT ( 'NONE',  ( 6.950374756619257965, 24.88503499907601935, -26.09010956794244507 ) ) ;
#16281 = CARTESIAN_POINT ( 'NONE',  ( -24.50000000000000711, 13.09999999999999432, 7.960532557706201828 ) ) ;
#16282 = CARTESIAN_POINT ( 'NONE',  ( 20.75514604977249178, 17.82500000273119767, 28.56700777964553950 ) ) ;
#16283 = CARTESIAN_POINT ( 'NONE',  ( -13.97622843553632421, 49.95572916666665009, -24.20753774853731599 ) ) ;
#16284 = ORIENTED_EDGE ( 'NONE', *, *, #4908, .F. ) ;
#16285 = CARTESIAN_POINT ( 'NONE',  ( -20.75514604977248112, 57.42500000273118843, 28.56700777964554661 ) ) ;
#16286 = VERTEX_POINT ( 'NONE', #13935 ) ;
#16287 = CARTESIAN_POINT ( 'NONE',  ( -7.505752307973343918, 19.16145833333332860, -28.01184896238290989 ) ) ;
#16288 = CARTESIAN_POINT ( 'NONE',  ( 28.00173670424549499, 11.43267333425730925, 7.543491769121417612 ) ) ;
#16289 = CARTESIAN_POINT ( 'NONE',  ( 20.75514604977248467, 2.425000002731189763, -28.56700777964554305 ) ) ;
#16290 = ORIENTED_EDGE ( 'NONE', *, *, #8518, .T. ) ;
#16291 = LINE ( 'NONE', #647, #23426 ) ;
#16292 = CARTESIAN_POINT ( 'NONE',  ( -33.58253175000000113, 29.47500000273117848, 10.91162601494193929 ) ) ;
#16293 = CARTESIAN_POINT ( 'NONE',  ( -26.29305231718578995, 32.70000000546238539, 19.10302069950538595 ) ) ;
#16294 = CARTESIAN_POINT ( 'NONE',  ( 10.04305231718578817, 77.39999999999999147, -30.90933677959249337 ) ) ;
#16295 = CARTESIAN_POINT ( 'NONE',  ( 5.779280353836490358E-15, 25.00000000546237899, 32.49999999999999289 ) ) ;
#16296 = CARTESIAN_POINT ( 'NONE',  ( 15.00000000000000000, 73.00000000000001421, -1.836970198721029589E-15 ) ) ;
#16297 = CARTESIAN_POINT ( 'NONE',  ( 10.37757302488624056, 42.77500000273118275, -31.93888565452638417 ) ) ;
#16298 = AXIS2_PLACEMENT_3D ( 'NONE', #30014, #32752, #14244 ) ;
#16299 = B_SPLINE_CURVE_WITH_KNOTS ( 'NONE', 3,
 ( #7728, #5327, #15975, #31066, #157, #23525, #28660, #31405, #23865, #10648, #332, #23182, #23358, #10818, #8066, #31738, #5156, #15641, #18723, #26092, #10478, #12882, #29159, #15808, #5666, #3098, #33645, #10142, #18045, #7561, #28489, #15467, #25920, #33819, #32069, #1162, #3424, #29998, #13896, #24363, #26768, #11154, #14062, #21955 ),
 .UNSPECIFIED., .F., .F.,
 ( 4, 2, 2, 2, 2, 2, 2, 2, 2, 2, 2, 2, 2, 2, 2, 2, 2, 2, 2, 2, 2, 4 ),
 ( 0.000000000000000000, 0.004064997385822684446, 0.008129994771645368892, 0.01219499215746805247, 0.01422749085037939600, 0.01625998954329073778, 0.02032498692911342136, 0.02235748562202476489, 0.02438998431493610147, 0.02845498170075878158, 0.03251997908658145475, 0.03455247777949279481, 0.03658497647240413486, 0.04064997385822680803, 0.04471497124404947426, 0.04877996862987214050, 0.05081246732278348055, 0.05284496601569481367, 0.05690996340151748684, 0.05894246209442883383, 0.06097496078734017388, 0.06503995817316285399 ),
 .UNSPECIFIED. ) ;
#16300 = CARTESIAN_POINT ( 'NONE',  ( -10.04305231718579172, 25.59999999999999787, -30.90933677959248982 ) ) ;
#16301 = CARTESIAN_POINT ( 'NONE',  ( 26.29305231718578995, 23.19999999999999929, -19.10302069950538240 ) ) ;
#16302 = CARTESIAN_POINT ( 'NONE',  ( -4.732186688966233175E-15, 9.499999999999991118, 25.76082449383753925 ) ) ;
#16303 = EDGE_CURVE ( 'NONE', #16782, #26616, #24399, .T. ) ;
#16304 = CARTESIAN_POINT ( 'NONE',  ( 33.58253175000000113, 60.12500000273119127, -4.112674001490185761E-15 ) ) ;
#16305 = CARTESIAN_POINT ( 'NONE',  ( 1.577395562988744260E-15, 8.249999994537613901, -25.76082449383753925 ) ) ;
#16306 = CARTESIAN_POINT ( 'NONE',  ( 11.56287504972942592, 74.00000000000000000, -7.975283324587876699 ) ) ;
#16307 = CARTESIAN_POINT ( 'NONE',  ( -20.75514604977248112, 51.67500000273117422, 28.56700777964554661 ) ) ;
#16308 = CARTESIAN_POINT ( 'NONE',  ( 14.47279130897151944, 6.924999997268805885, -19.92008829642072598 ) ) ;
#16309 = DIRECTION ( 'NONE',  ( -1.224646799147353454E-16, 1.000000000000000000, -0.000000000000000000 ) ) ;
#16310 = CARTESIAN_POINT ( 'NONE',  ( 10.37757302488624767, 5.725000002731183812, 31.93888565452638417 ) ) ;
#16311 = CARTESIAN_POINT ( 'NONE',  ( 27.95245687107223986, 35.35194416759064495, 0.04044903254993640479 ) ) ;
#16312 = CARTESIAN_POINT ( 'NONE',  ( 4.445600272181915325E-13, 26.00000000546237189, -32.50000000000000000 ) ) ;
#16313 = DIRECTION ( 'NONE',  ( -0.000000000000000000, -1.000000000000000000, -0.000000000000000000 ) ) ;
#16314 = CARTESIAN_POINT ( 'NONE',  ( 6.486482029760649416E-15, 29.62500000273120193, 35.31076352940723240 ) ) ;
#16315 = DIRECTION ( 'NONE',  ( 0.000000000000000000, 0.000000000000000000, 1.000000000000000000 ) ) ;
#16316 = CARTESIAN_POINT ( 'NONE',  ( -12.11607355459419821, -70.99969134886156041, 1.483791069686768580E-15 ) ) ;
#16317 = CARTESIAN_POINT ( 'NONE',  ( 5.779280353836490358E-15, 1.000000005462375885, 32.49999999999999289 ) ) ;
#16318 = CARTESIAN_POINT ( 'NONE',  ( -28.02196122052058413, 54.96315999907602645, -7.468012846824272799 ) ) ;
#16319 = CARTESIAN_POINT ( 'NONE',  ( 10.04305231718578817, 45.90000000546238823, -30.90933677959249337 ) ) ;
#16320 = DIRECTION ( 'NONE',  ( -1.224646799147353454E-16, 1.000000000000000000, -0.000000000000000000 ) ) ;
#16321 = CARTESIAN_POINT ( 'NONE',  ( -10.04305231718578462, 58.90000000546240244, 30.90933677959249337 ) ) ;
#16322 = CARTESIAN_POINT ( 'NONE',  ( -19.09188309203694445, 25.74999999999999645, -19.09188309203661049 ) ) ;
#16323 = AXIS2_PLACEMENT_3D ( 'NONE', #18864, #31883, #18704 ) ;
#16324 = CARTESIAN_POINT ( 'NONE',  ( -26.29305231718579350, 68.30000000546237970, -19.10302069950537884 ) ) ;
#16325 = CARTESIAN_POINT ( 'NONE',  ( 20.50609665440969565, 26.60937499999999645, -20.50609665441004736 ) ) ;
#16326 = CARTESIAN_POINT ( 'NONE',  ( -23.41746824999999887, 16.02499999726881086, -7.608796670333730638 ) ) ;
#16327 = ORIENTED_EDGE ( 'NONE', *, *, #12841, .T. ) ;
#16328 = CARTESIAN_POINT ( 'NONE',  ( -28.00173670424549499, 40.65142333425730214, -7.543491769121417612 ) ) ;
#16329 = CARTESIAN_POINT ( 'NONE',  ( 6.277390505771533514E-15, 17.00000000546237544, 34.17252228774368916 ) ) ;
#16330 = CARTESIAN_POINT ( 'NONE',  ( 30.02300923189239512, 54.53906249999998579, -2.619432448724977703E-13 ) ) ;
#16331 = CARTESIAN_POINT ( 'NONE',  ( 10.04305231718579705, 74.59999999999999432, 30.90933677959248982 ) ) ;
#16332 = CARTESIAN_POINT ( 'NONE',  ( -20.75514604977248823, 47.07500000273117990, -28.56700777964554305 ) ) ;
#16333 = CARTESIAN_POINT ( 'NONE',  ( 32.50000000000000711, 49.40000000546236691, 10.55989012756945122 ) ) ;
#16334 = CARTESIAN_POINT ( 'NONE',  ( -13.91746824999999532, 81.27500000273117564, -4.522059556121115875 ) ) ;
#16335 = CARTESIAN_POINT ( 'NONE',  ( -33.58253175000000113, 33.12500000273119127, 0.000000000000000000 ) ) ;
#16336 = CARTESIAN_POINT ( 'NONE',  ( 0.000000000000000000, 52.00000000000000711, 0.000000000000000000 ) ) ;
#16337 = CARTESIAN_POINT ( 'NONE',  ( 27.16883889988623935, 60.57500000273119412, -19.73931689729374384 ) ) ;
#16338 = CARTESIAN_POINT ( 'NONE',  ( 13.44965385310867312, 74.00000000000005684, 3.606845949684043706 ) ) ;
#16339 = CARTESIAN_POINT ( 'NONE',  ( -33.58253175000000113, 53.22500000273118559, 10.91162601494193929 ) ) ;
#16340 = CARTESIAN_POINT ( 'NONE',  ( -32.50000000000000000, 38.00000000000000711, 0.000000000000000000 ) ) ;
#16341 = CARTESIAN_POINT ( 'NONE',  ( 14.47279130897151767, 6.924999997268805885, -19.92008829642072598 ) ) ;
#16342 = CARTESIAN_POINT ( 'NONE',  ( -2.162160676586881955E-15, 6.875000002731195714, -35.31076352940723240 ) ) ;
#16343 = CARTESIAN_POINT ( 'NONE',  ( 26.29305231718579350, 35.30000000546237970, 19.10302069950537529 ) ) ;
#16344 = CARTESIAN_POINT ( 'NONE',  ( -13.91746824999999887, 73.37500000273119838, 0.000000000000000000 ) ) ;
#16345 = CARTESIAN_POINT ( 'NONE',  ( 27.16883889988623935, 72.57500000273120122, -19.73931689729374384 ) ) ;
#16346 = CARTESIAN_POINT ( 'NONE',  ( -3.880418787951142701, 19.19874571299078525, 24.49999999999999645 ) ) ;
#16347 = CARTESIAN_POINT ( 'NONE',  ( -20.75514604977248823, 71.07500000273117280, -28.56700777964554305 ) ) ;
#16348 = EDGE_LOOP ( 'NONE', ( #21605, #17280 ) ) ;
#16349 = FACE_OUTER_BOUND ( 'NONE', #6680, .T. ) ;
#16350 = AXIS2_PLACEMENT_3D ( 'NONE', #27224, #3225, #29786 ) ;
#16351 = CARTESIAN_POINT ( 'NONE',  ( 7.025853678916403666, 14.01079833425730747, -26.06988505166735237 ) ) ;
#16352 = DIRECTION ( 'NONE',  ( 0.000000000000000000, 0.000000000000000000, -1.000000000000000000 ) ) ;
#16353 = CARTESIAN_POINT ( 'NONE',  ( -20.75514604977248823, 44.82500000273117990, -28.56700777964554305 ) ) ;
#16354 = CARTESIAN_POINT ( 'NONE',  ( 6.486482029760649416E-15, 11.87500000273118062, 35.31076352940723240 ) ) ;
#16355 = CARTESIAN_POINT ( 'NONE',  ( 10.37757302488624767, 63.97500000273119269, 31.93888565452638417 ) ) ;
#16356 = CARTESIAN_POINT ( 'NONE',  ( 19.09188309203694800, 48.09375000000000000, 19.09188309203660694 ) ) ;
#16357 = CARTESIAN_POINT ( 'NONE',  ( -28.02196122052045268, 30.05246500092397000, 7.468012846824790607 ) ) ;
#16358 = CARTESIAN_POINT ( 'NONE',  ( -26.02091320914878025, 27.60638916574269075, -14.97647472619899389 ) ) ;
#16359 = CARTESIAN_POINT ( 'NONE',  ( -2.092463501923844636E-15, 72.00000000546236834, -34.17252228774368916 ) ) ;
#16360 = CARTESIAN_POINT ( 'NONE',  ( 2.205017735002230837E-13, 56.00000000546238255, -32.50000000000000000 ) ) ;
#16361 = CARTESIAN_POINT ( 'NONE',  ( 20.75514604977249178, 41.82500000273120122, 28.56700777964553950 ) ) ;
#16362 = CARTESIAN_POINT ( 'NONE',  ( 19.06425588902558133, 42.35899333240935505, -19.11951029504797006 ) ) ;
#16363 = CARTESIAN_POINT ( 'NONE',  ( -23.41746825000000243, 17.52499999726881796, -7.608796670333730638 ) ) ;
#16364 = CARTESIAN_POINT ( 'NONE',  ( 26.29305231718578995, 13.70000000546239782, -19.10302069950538240 ) ) ;
#16365 = ORIENTED_EDGE ( 'NONE', *, *, #9685, .T. ) ;
#16366 = EDGE_CURVE ( 'NONE', #17243, #32915, #26524, .T. ) ;
#16367 = CARTESIAN_POINT ( 'NONE',  ( -33.58253175000000113, 47.37500000273119127, 0.000000000000000000 ) ) ;
#16368 = CARTESIAN_POINT ( 'NONE',  ( 10.04305231718579705, 50.60000000000000853, 30.90933677959248982 ) ) ;
#16369 = CARTESIAN_POINT ( 'NONE',  ( 7.025853678916403666, 48.38579833425730925, -26.06988505166735237 ) ) ;
#16370 = CARTESIAN_POINT ( 'NONE',  ( -10.37757302488623701, 67.77500000273117564, 31.93888565452638417 ) ) ;
#16371 = EDGE_CURVE ( 'NONE', #31469, #16121, #18216, .T. ) ;
#16372 = ORIENTED_EDGE ( 'NONE', *, *, #2433, .F. ) ;
#16373 = CARTESIAN_POINT ( 'NONE',  ( -33.58253175000000113, 17.02500000273118985, -10.91162601494193218 ) ) ;
#16374 = CARTESIAN_POINT ( 'NONE',  ( 7.505752307973351023, 24.31770833333332504, 28.01184896238290278 ) ) ;
#16375 = VERTEX_POINT ( 'NONE', #17187 ) ;
#16376 = CARTESIAN_POINT ( 'NONE',  ( 10.04305231718579705, 65.10000000546240528, 30.90933677959248982 ) ) ;
#16377 = CARTESIAN_POINT ( 'NONE',  ( -33.58253175000000113, 55.22500000273117848, 10.91162601494193929 ) ) ;
#16378 = CARTESIAN_POINT ( 'NONE',  ( 28.01184896238304134, 51.24479166666666430, 7.505752307972846538 ) ) ;
#16379 = CARTESIAN_POINT ( 'NONE',  ( 32.50000000000000711, 15.40000000546236514, 10.55989012756945122 ) ) ;
#16380 = CARTESIAN_POINT ( 'NONE',  ( 15.14183272437242422, 16.04999999453762882, -20.84094480462497856 ) ) ;
#16381 = CARTESIAN_POINT ( 'NONE',  ( 14.47279130897151767, 10.82499999726879913, 19.92008829642072953 ) ) ;
#16382 = CARTESIAN_POINT ( 'NONE',  ( 27.16883889988623935, 24.57500000273119056, -19.73931689729374384 ) ) ;
#16383 = CARTESIAN_POINT ( 'NONE',  ( -5.147494310547430452, 63.55125428154684641, -32.49999999999999289 ) ) ;
#16384 = CARTESIAN_POINT ( 'NONE',  ( 28.02196122052058413, 66.99440999907601224, 7.468012846824272799 ) ) ;
#16385 = CARTESIAN_POINT ( 'NONE',  ( -8.601468415847518756, 78.57500000273120122, -11.83890561707634781 ) ) ;
#16386 = CARTESIAN_POINT ( 'NONE',  ( 26.29305231718578995, 15.19999999999999218, -19.10302069950538240 ) ) ;
#16387 = CARTESIAN_POINT ( 'NONE',  ( -10.04305231718578462, 10.40000000000000568, 30.90933677959249337 ) ) ;
#16388 = ORIENTED_EDGE ( 'NONE', *, *, #32529, .F. ) ;
#16389 = CARTESIAN_POINT ( 'NONE',  ( 7.570916362186207671, 17.34999999453762243, 23.30088464923126779 ) ) ;
#16390 = CARTESIAN_POINT ( 'NONE',  ( -8.960552108402742093E-16, 72.37500000273116996, -14.63369212191046387 ) ) ;
#16391 = CARTESIAN_POINT ( 'NONE',  ( 26.07999730980490227, 34.05729166666666430, 6.988114217767821046 ) ) ;
#16392 = CARTESIAN_POINT ( 'NONE',  ( -2.162160676586881955E-15, 24.62500000273118772, -35.31076352940723240 ) ) ;
#16393 = CARTESIAN_POINT ( 'NONE',  ( -20.75514604977248823, 70.82500000273117280, -28.56700777964554305 ) ) ;
#16394 = CARTESIAN_POINT ( 'NONE',  ( -27.16883889988624290, 33.17500000273120264, -19.73931689729374028 ) ) ;
#16395 = CARTESIAN_POINT ( 'NONE',  ( 33.58253175000000113, 18.37500000273119127, -4.112674001490185761E-15 ) ) ;
#16396 = CARTESIAN_POINT ( 'NONE',  ( -27.16883889988623935, 15.57500000273118168, 19.73931689729374739 ) ) ;
#16397 = CARTESIAN_POINT ( 'NONE',  ( 19.06425588902592239, 59.84413166759065206, 19.11951029504763611 ) ) ;
#16398 = CARTESIAN_POINT ( 'NONE',  ( 10.37757302488624767, 69.72500000273117848, 31.93888565452638417 ) ) ;
#16399 = CYLINDRICAL_SURFACE ( 'NONE', #30994, 32.50000000000000000 ) ;
#16400 = CARTESIAN_POINT ( 'NONE',  ( -11.25946833292375793, 75.57500000273120122, 8.180482586598737171 ) ) ;
#16401 = CARTESIAN_POINT ( 'NONE',  ( -10.04305231718579172, 55.59999999999999432, -30.90933677959248982 ) ) ;
#16402 = CARTESIAN_POINT ( 'NONE',  ( -1.778240108872766143E-15, 63.50000000000000000, -32.49999999999999289 ) ) ;
#16403 = CARTESIAN_POINT ( 'NONE',  ( 27.16883889988624290, 55.92500000273120975, 19.73931689729373673 ) ) ;
#16404 = CARTESIAN_POINT ( 'NONE',  ( -18.94512977948576093, 12.32499999726879913, 13.76444248337722698 ) ) ;
#16405 = EDGE_CURVE ( 'NONE', #7955, #7360, #20443, .T. ) ;
#16406 = ORIENTED_EDGE ( 'NONE', *, *, #30108, .F. ) ;
#16407 = CARTESIAN_POINT ( 'NONE',  ( -20.75514604977248823, 67.07500000273118701, -28.56700777964554305 ) ) ;
#16408 =( BOUNDED_CURVE ( )  B_SPLINE_CURVE ( 2, ( #26935, #3433, #13906, #24372, #844, #29664, #9238 ),
 .UNSPECIFIED., .F., .T. ) 
 B_SPLINE_CURVE_WITH_KNOTS ( ( 3, 2, 2, 3 ),
 ( 0.9166666666666667407, 0.9222222222222221655, 0.9333333333333329040, 0.9444444444444436426 ),
 .UNSPECIFIED. ) 
 CURVE ( )  GEOMETRIC_REPRESENTATION_ITEM ( )  RATIONAL_B_SPLINE_CURVE ( ( 0.9755282581475768211, 0.9755282581475770431, 1.000000000000000000, 0.9510565162951535312, 1.000000000000000000, 0.9510565162951569729, 0.9999999999999965583 ) ) 
 REPRESENTATION_ITEM ( '' )  );
#16409 = CARTESIAN_POINT ( 'NONE',  ( 33.58253175000000113, 2.125000002731192161, -4.112674001490185761E-15 ) ) ;
#16410 = CARTESIAN_POINT ( 'NONE',  ( -7.236395654485757944, 7.224999997268804819, -22.27133577429736988 ) ) ;
#16411 = CARTESIAN_POINT ( 'NONE',  ( -7.025853678916393008, 22.60454833425730925, 26.06988505166735592 ) ) ;
#16412 = EDGE_CURVE ( 'NONE', #19608, #17758, #13600, .T. ) ;
#16413 = VERTEX_POINT ( 'NONE', #27817 ) ;
#16414 = CARTESIAN_POINT ( 'NONE',  ( -33.58253175000000113, 39.12500000273118417, 0.000000000000000000 ) ) ;
#16415 = CYLINDRICAL_SURFACE ( 'NONE', #29658, 32.50000000000000000 ) ;
#16416 = ORIENTED_EDGE ( 'NONE', *, *, #655, .F. ) ;
#16417 = CARTESIAN_POINT ( 'NONE',  ( 15.01150461594596308, 53.96614583333333570, -26.00068869287367335 ) ) ;
#16418 = CARTESIAN_POINT ( 'NONE',  ( -10.37757302488624411, 66.97500000273119269, -31.93888565452638417 ) ) ;
#16419 = DIRECTION ( 'NONE',  ( 0.000000000000000000, -1.000000000000000000, 0.000000000000000000 ) ) ;
#16420 = CARTESIAN_POINT ( 'NONE',  ( 27.16883889988624290, 75.92500000273119554, 19.73931689729373673 ) ) ;
#16421 = CARTESIAN_POINT ( 'NONE',  ( -7.505752307972844761, 17.72916666666666430, 28.01184896238304134 ) ) ;
#16422 = CARTESIAN_POINT ( 'NONE',  ( 15.14183272437242245, 8.300000000000000711, -20.84094480462497856 ) ) ;
#16423 = CARTESIAN_POINT ( 'NONE',  ( -33.58253175000000113, 7.275000002731181858, -10.91162601494193218 ) ) ;
#16424 = CARTESIAN_POINT ( 'NONE',  ( -33.58253175000000113, 19.02500000273118630, -10.91162601494193218 ) ) ;
#16425 = CARTESIAN_POINT ( 'NONE',  ( 13.91746825000000065, 79.77500000273118985, 4.522059556121115875 ) ) ;
#16426 = CARTESIAN_POINT ( 'NONE',  ( 5.779280353836490358E-15, 65.00000000546236834, 32.49999999999999289 ) ) ;
#16427 = CARTESIAN_POINT ( 'NONE',  ( 26.02091320914876960, 36.20013916574269075, 14.97647472619900455 ) ) ;
#16428 = CARTESIAN_POINT ( 'NONE',  ( -15.00000000000000000, 78.10000000000000853, 4.873795443493597723 ) ) ;
#16429 = CARTESIAN_POINT ( 'NONE',  ( -28.01184896238304134, 46.08854166666666430, -7.505752307972844761 ) ) ;
#16430 = CARTESIAN_POINT ( 'NONE',  ( -3.880418787951136483, 8.301254276084460315, -24.50000000000000000 ) ) ;
#16431 = CARTESIAN_POINT ( 'NONE',  ( 26.29305231718579350, 49.30000000546236549, 19.10302069950537529 ) ) ;
#16432 = CARTESIAN_POINT ( 'NONE',  ( 19.11951029504797006, 60.40586833240935505, 19.06425588902558133 ) ) ;
#16433 = CARTESIAN_POINT ( 'NONE',  ( 33.58253175000000113, 42.12500000273116996, -4.112674001490185761E-15 ) ) ;
#16434 = CARTESIAN_POINT ( 'NONE',  ( 4.300734207923761154, 79.47500000273116427, 13.23629886949340495 ) ) ;
#16435 = CARTESIAN_POINT ( 'NONE',  ( 33.58253175000000823, 48.27500000273119696, 10.91162601494192863 ) ) ;
#16436 = CARTESIAN_POINT ( 'NONE',  ( -2.162160676586882350E-15, 34.87500000273117706, -35.31076352940722529 ) ) ;
#16437 = CARTESIAN_POINT ( 'NONE',  ( 20.64299112944278036, 16.99999999999997868, 11.19067762888292350 ) ) ;
#16438 = CARTESIAN_POINT ( 'NONE',  ( 13.97622843553589966, 23.02864583333332504, -24.20753774853756113 ) ) ;
#16439 = CARTESIAN_POINT ( 'NONE',  ( -9.270509831248423538, 79.95000000546238539, -12.75976212528059861 ) ) ;
#16440 = CARTESIAN_POINT ( 'NONE',  ( -10.04305231718578462, 70.40000000000000568, 30.90933677959249337 ) ) ;
#16441 = CARTESIAN_POINT ( 'NONE',  ( -27.16883889988623935, 9.325000002731190563, 19.73931689729374739 ) ) ;
#16442 = CARTESIAN_POINT ( 'NONE',  ( 23.41746824999999887, 4.624999997268814056, 0.000000000000000000 ) ) ;
#16443 = FACE_OUTER_BOUND ( 'NONE', #6937, .T. ) ;
#16444 = CARTESIAN_POINT ( 'NONE',  ( 6.950374756619257965, 28.32253499907601579, -26.09010956794244507 ) ) ;
#16445 = CARTESIAN_POINT ( 'NONE',  ( -26.29305231718579350, 59.79999999999999005, -19.10302069950537884 ) ) ;
#16446 = CARTESIAN_POINT ( 'NONE',  ( 27.16883889988624290, 17.92500000273117422, 19.73931689729373673 ) ) ;
#16447 = CARTESIAN_POINT ( 'NONE',  ( -14.47279130897152122, 8.424999997268816543, 19.92008829642072243 ) ) ;
#16448 = CARTESIAN_POINT ( 'NONE',  ( -26.07999730980490583, 56.40104166666666430, -6.988114217767815717 ) ) ;
#16449 = ORIENTED_EDGE ( 'NONE', *, *, #26976, .F. ) ;
#16450 = CARTESIAN_POINT ( 'NONE',  ( 6.486482029760649416E-15, 55.62500000273119838, 35.31076352940723240 ) ) ;
#16451 = ORIENTED_EDGE ( 'NONE', *, *, #21264, .T. ) ;
#16452 = CARTESIAN_POINT ( 'NONE',  ( 2.740863092043355209E-13, 27.89843750000000000, 30.02300923189239512 ) ) ;
#16453 = CARTESIAN_POINT ( 'NONE',  ( 15.04653450569292872, 24.46652750092397355, -25.98046417659857710 ) ) ;
#16454 = CARTESIAN_POINT ( 'NONE',  ( 1.836970198721029589E-15, 74.00000000000001421, -15.00000000000000000 ) ) ;
#16455 = CARTESIAN_POINT ( 'NONE',  ( 14.47279130897151589, 4.324999997268801799, 19.92008829642072953 ) ) ;
#16456 = CARTESIAN_POINT ( 'NONE',  ( -27.16883889988623935, 31.57500000273119767, 19.73931689729374739 ) ) ;
#16457 = CARTESIAN_POINT ( 'NONE',  ( 20.08610463437158344, 33.20000000546238539, 27.64615127144129403 ) ) ;
#16458 = CARTESIAN_POINT ( 'NONE',  ( 32.50000000000000711, 78.89999999999999147, 10.55989012756945122 ) ) ;
#16459 = CARTESIAN_POINT ( 'NONE',  ( 0.000000000000000000, 82.00000000000001421, 0.000000000000000000 ) ) ;
#16460 = DIRECTION ( 'NONE',  ( -0.000000000000000000, 1.000000000000000000, -0.000000000000000000 ) ) ;
#16461 = CARTESIAN_POINT ( 'NONE',  ( -33.58253175000000113, 41.47500000273117138, 10.91162601494193929 ) ) ;
#16462 = CARTESIAN_POINT ( 'NONE',  ( -26.29305231718579350, 21.80000000000000071, -19.10302069950537884 ) ) ;
#16463 = CARTESIAN_POINT ( 'NONE',  ( 10.04305231718579705, 18.60000000000000497, 30.90933677959248982 ) ) ;
#16464 = CARTESIAN_POINT ( 'NONE',  ( -7.570916362186210335, 14.60000000000000142, -23.30088464923126779 ) ) ;
#16465 = CARTESIAN_POINT ( 'NONE',  ( 27.16883889988623935, 62.32500000273119412, -19.73931689729374384 ) ) ;
#16466 = CARTESIAN_POINT ( 'NONE',  ( 27.16883889988624290, 52.17500000273117422, 19.73931689729373673 ) ) ;
#16467 = CARTESIAN_POINT ( 'NONE',  ( -23.41746825000000243, 11.72499999726879949, 7.608796670333725309 ) ) ;
#16468 = CARTESIAN_POINT ( 'NONE',  ( -19.82091636218621034, 8.800000000000002487, -14.40073868116559552 ) ) ;
#16469 = CARTESIAN_POINT ( 'NONE',  ( 10.37757302488624056, 4.525000002731205839, -31.93888565452638417 ) ) ;
#16470 = CARTESIAN_POINT ( 'NONE',  ( 27.95245687107223986, 38.78944416759064495, 0.04044903254993640479 ) ) ;
#16471 = CARTESIAN_POINT ( 'NONE',  ( 22.66806446082019733, 16.99999999999997868, -6.072923278005473158 ) ) ;
#16472 = CARTESIAN_POINT ( 'NONE',  ( 11.64495469945098627, 52.00000000000000000, 31.50463004621144947 ) ) ;
#16473 = CARTESIAN_POINT ( 'NONE',  ( 27.16883889988623935, 28.32500000273117990, -19.73931689729374384 ) ) ;
#16474 = CARTESIAN_POINT ( 'NONE',  ( -32.50000000000000000, 56.50000000546238965, 0.000000000000000000 ) ) ;
#16475 = CARTESIAN_POINT ( 'NONE',  ( -10.04305231718579172, 30.10000000546236976, -30.90933677959248982 ) ) ;
#16476 = CARTESIAN_POINT ( 'NONE',  ( 28.00173670424535644, 59.83295166574269075, -7.543491769121920321 ) ) ;
#16477 = CARTESIAN_POINT ( 'NONE',  ( 32.50000000000000000, 45.50000000546238255, -3.980102097228898626E-15 ) ) ;
#16478 = CARTESIAN_POINT ( 'NONE',  ( 20.08610463437158344, 48.70000000000000284, 27.64615127144129403 ) ) ;
#16479 = CARTESIAN_POINT ( 'NONE',  ( -5.147494310547423346, 58.94874572391554324, 32.50000000000000000 ) ) ;
#16480 = CARTESIAN_POINT ( 'NONE',  ( -13.97622843553588901, 28.18489583333332860, 24.20753774853756823 ) ) ;
#16481 = ORIENTED_EDGE ( 'NONE', *, *, #28656, .F. ) ;
#16482 = CARTESIAN_POINT ( 'NONE',  ( -33.58253175000000113, 77.22500000273117848, 10.91162601494193929 ) ) ;
#16483 = CARTESIAN_POINT ( 'NONE',  ( 28.01184896238304134, 30.61979166666666075, 7.505752307972846538 ) ) ;
#16484 = CARTESIAN_POINT ( 'NONE',  ( 11.45223628611453215, -57.99999999999999289, 1.402494451086933009E-15 ) ) ;
#16485 = ORIENTED_EDGE ( 'NONE', *, *, #31598, .F. ) ;
#16486 = CARTESIAN_POINT ( 'NONE',  ( -14.97647472619946285, 47.95611083425732346, -26.02091320914851025 ) ) ;
#16487 = CARTESIAN_POINT ( 'NONE',  ( 26.29305231718579350, 15.30000000546237438, 19.10302069950537529 ) ) ;
#16488 = EDGE_CURVE ( 'NONE', #26696, #9328, #20408, .T. ) ;
#16489 = CARTESIAN_POINT ( 'NONE',  ( -7.505752307973343918, 53.53645833333332860, -28.01184896238290989 ) ) ;
#16490 = CARTESIAN_POINT ( 'NONE',  ( -5.147494310547423346, 36.44874571845313227, 32.50000000000000000 ) ) ;
#16491 = CARTESIAN_POINT ( 'NONE',  ( 33.58253175000000113, 50.47500000273117848, -10.91162601494193751 ) ) ;
#16492 = CARTESIAN_POINT ( 'NONE',  ( -26.29305231718578995, 50.70000000546237828, 19.10302069950538595 ) ) ;
#16493 =( BOUNDED_CURVE ( )  B_SPLINE_CURVE ( 2, ( #9662, #30587, #1242, #17567, #14475, #3834, #11720, #1417, #14648, #30072, #14815, #28024, #25280 ),
 .UNSPECIFIED., .F., .F. ) 
 B_SPLINE_CURVE_WITH_KNOTS ( ( 3, 2, 2, 2, 2, 2, 3 ),
 ( 0.08333333333333334259, 0.08461538461538462008, 0.08717948717948717507, 0.08974358974358974395, 0.09230769230769231282, 0.09487179487179486781, 0.09615384615384615918 ),
 .UNSPECIFIED. ) 
 CURVE ( )  GEOMETRIC_REPRESENTATION_ITEM ( )  RATIONAL_B_SPLINE_CURVE ( ( 0.9755282581475767101, 0.9755282581475768211, 1.000000000000000000, 0.9510565162951535312, 1.000000000000000000, 0.9510565162951535312, 1.000000000000000000, 0.9510565162951535312, 1.000000000000000000, 0.9510565162951535312, 1.000000000000000000, 0.9755282581475765991, 0.9755282581475767101 ) ) 
 REPRESENTATION_ITEM ( '' )  );
#16494 = CARTESIAN_POINT ( 'NONE',  ( 4.300734207923761154, 79.97500000273122112, 13.23629886949340495 ) ) ;
#16495 = CARTESIAN_POINT ( 'NONE',  ( -33.58253175000000113, 33.02500000273118275, -10.91162601494193218 ) ) ;
#16496 = FACE_OUTER_BOUND ( 'NONE', #8084, .T. ) ;
#16497 = CARTESIAN_POINT ( 'NONE',  ( -2.162160676586881955E-15, 60.87500000273116996, -35.31076352940723240 ) ) ;
#16498 = SURFACE_STYLE_FILL_AREA ( #17003 ) ;
#16499 = EDGE_CURVE ( 'NONE', #13970, #29891, #19926, .T. ) ;
#16500 = CARTESIAN_POINT ( 'NONE',  ( 20.08610463437158344, 40.69999999999999574, 27.64615127144129403 ) ) ;
#16501 = CARTESIAN_POINT ( 'NONE',  ( 1.507698388325705758E-15, 13.12499999726881228, -24.62258325217400312 ) ) ;
#16502 = CARTESIAN_POINT ( 'NONE',  ( 20.75514604977248467, 2.675000002731181770, -28.56700777964554305 ) ) ;
#16503 = CARTESIAN_POINT ( 'NONE',  ( 10.04305231718578817, 13.39999999999999503, -30.90933677959249337 ) ) ;
#16504 = CARTESIAN_POINT ( 'NONE',  ( 4.300734207923757602, 72.77500000273118985, -13.23629886949340673 ) ) ;
#16505 = CARTESIAN_POINT ( 'NONE',  ( 27.16883889988623935, 70.57500000273120122, -19.73931689729374384 ) ) ;
#16506 = CARTESIAN_POINT ( 'NONE',  ( -24.50000000000000711, 5.100000000000012967, 7.960532557706201828 ) ) ;
#16507 = EDGE_CURVE ( 'NONE', #12563, #13367, #9620, .T. ) ;
#16508 = CARTESIAN_POINT ( 'NONE',  ( 33.58253175000000823, 68.27500000273120406, 10.91162601494192863 ) ) ;
#16509 = ORIENTED_EDGE ( 'NONE', *, *, #18928, .F. ) ;
#16510 = CARTESIAN_POINT ( 'NONE',  ( -15.14183272437242600, 7.049999994537622605, 20.84094480462497856 ) ) ;
#16511 = CARTESIAN_POINT ( 'NONE',  ( -0.04044903254992426173, 12.14881916759064140, 27.95245687107223276 ) ) ;
#16512 = CARTESIAN_POINT ( 'NONE',  ( 3.980102097228898626E-15, 52.00000000000000711, -32.50000000000000000 ) ) ;
#16513 = CARTESIAN_POINT ( 'NONE',  ( 33.58253175000000113, 50.12500000273119127, -4.112674001490185761E-15 ) ) ;
#16514 = CARTESIAN_POINT ( 'NONE',  ( -33.58253175000000113, 9.375000002731184168, 0.000000000000000000 ) ) ;
#16515 = CARTESIAN_POINT ( 'NONE',  ( -2.162160676586882350E-15, 64.87500000273119838, -35.31076352940722529 ) ) ;
#16516 = CARTESIAN_POINT ( 'NONE',  ( -19.09188309203694445, 53.25000000000000000, -19.09188309203661049 ) ) ;
#16517 = CARTESIAN_POINT ( 'NONE',  ( 28.00173670424549499, 38.93267333425729504, 7.543491769121417612 ) ) ;
#16518 = CARTESIAN_POINT ( 'NONE',  ( 15.04653450569339945, 29.61159749907602290, 25.98046417659831775 ) ) ;
#16519 = CARTESIAN_POINT ( 'NONE',  ( -2.092463501923844636E-15, 68.00000000546236834, -34.17252228774368916 ) ) ;
#16520 = AXIS2_PLACEMENT_3D ( 'NONE', #21816, #3450, #13920 ) ;
#16521 = CARTESIAN_POINT ( 'NONE',  ( 4.300734207923757602, 80.27500000273118985, -13.23629886949340673 ) ) ;
#16522 = CARTESIAN_POINT ( 'NONE',  ( 26.06988505166722803, 56.39545166574268364, -7.025853678916862854 ) ) ;
#16523 = CARTESIAN_POINT ( 'NONE',  ( -14.47279130897151589, 13.32499999726880624, -19.92008829642072598 ) ) ;
#16524 = CARTESIAN_POINT ( 'NONE',  ( 20.08610463437157279, 59.30000000000001847, -27.64615127144129758 ) ) ;
#16525 = ORIENTED_EDGE ( 'NONE', *, *, #15453, .F. ) ;
#16526 = CARTESIAN_POINT ( 'NONE',  ( 33.58253175000000113, 48.47500000273118559, -10.91162601494193751 ) ) ;
#16527 = DIRECTION ( 'NONE',  ( 0.000000000000000000, -1.000000000000000000, 0.000000000000000000 ) ) ;
#16528 = CIRCLE ( 'NONE', #7752, 2.000000000000000000 ) ;
#16529 = VECTOR ( 'NONE', #9594, 1000.000000000000114 ) ;
#16530 = CARTESIAN_POINT ( 'NONE',  ( -6.950374756619716266, 51.53684000092397355, -26.09010956794232428 ) ) ;
#16531 = CARTESIAN_POINT ( 'NONE',  ( 33.58253175000000113, 72.37500000273116996, -4.112674001490185761E-15 ) ) ;
#16532 = EDGE_LOOP ( 'NONE', ( #2207, #22987, #22164, #25604 ) ) ;
#16533 = CARTESIAN_POINT ( 'NONE',  ( -20.75514604977248823, 14.82500000273117635, -28.56700777964554305 ) ) ;
#16534 = CARTESIAN_POINT ( 'NONE',  ( 20.50609665440969565, 26.60937499999999645, -20.50609665441004736 ) ) ;
#16535 = EDGE_LOOP ( 'NONE', ( #6634, #3360, #3523, #20640, #33266, #30090 ) ) ;
#16536 = EDGE_LOOP ( 'NONE', ( #29868, #7784, #6223, #5562 ) ) ;
#16537 = CARTESIAN_POINT ( 'NONE',  ( -15.14183272437242778, 3.049999994537633263, 20.84094480462497856 ) ) ;
#16538 = CARTESIAN_POINT ( 'NONE',  ( 10.37757302488624767, 53.72500000273117138, 31.93888565452638417 ) ) ;
#16539 = CARTESIAN_POINT ( 'NONE',  ( -2.584737979205441561E-13, 53.67968750000000000, -30.02300923189239512 ) ) ;
#16540 = CARTESIAN_POINT ( 'NONE',  ( -26.29305231718579350, 12.30000000546238681, -19.10302069950537884 ) ) ;
#16541 = CARTESIAN_POINT ( 'NONE',  ( 24.50000000000000000, 15.84999999453763664, -7.960532557706203605 ) ) ;
#16542 = CARTESIAN_POINT ( 'NONE',  ( 7.236395654485760609, 7.524999997268800200, -22.27133577429736633 ) ) ;
#16543 = CARTESIAN_POINT ( 'NONE',  ( 10.37757302488624767, 23.97500000273117138, 31.93888565452638417 ) ) ;
#16544 = SURFACE_STYLE_FILL_AREA ( #19123 ) ;
#16545 = CARTESIAN_POINT ( 'NONE',  ( 26.06988505166722803, 15.14545166574268897, -7.025853678916862854 ) ) ;
#16546 = CARTESIAN_POINT ( 'NONE',  ( -10.04305231718579172, 31.59999999999999076, -30.90933677959248982 ) ) ;
#16547 = CARTESIAN_POINT ( 'NONE',  ( 20.08610463437158344, 14.70000000000000107, 27.64615127144129403 ) ) ;
#16548 = CARTESIAN_POINT ( 'NONE',  ( 32.50000000000000711, 10.89999999999998792, 10.55989012756945122 ) ) ;
#16549 = VERTEX_POINT ( 'NONE', #21125 ) ;
#16550 = CARTESIAN_POINT ( 'NONE',  ( -24.50000000000001066, 18.84999999453762953, 7.960532557706201828 ) ) ;
#16551 = CARTESIAN_POINT ( 'NONE',  ( 11.25946833292375793, 73.67500000273119554, 8.180482586598731842 ) ) ;
#16552 = CARTESIAN_POINT ( 'NONE',  ( 24.20753774853756113, 41.07552083333331439, 13.97622843553589789 ) ) ;
#16553 = EDGE_CURVE ( 'NONE', #16741, #6266, #21717, .T. ) ;
#16554 = CARTESIAN_POINT ( 'NONE',  ( 6.486482029760649416E-15, 27.62500000273118062, 35.31076352940723240 ) ) ;
#16555 = CARTESIAN_POINT ( 'NONE',  ( -27.16883889988623935, 69.32500000273118701, 19.73931689729374739 ) ) ;
#16556 = CARTESIAN_POINT ( 'NONE',  ( -10.37757302488623701, 27.77500000273118275, 31.93888565452638417 ) ) ;
#16557 = CARTESIAN_POINT ( 'NONE',  ( -20.75514604977248823, 19.07500000273118701, -28.56700777964554305 ) ) ;
#16558 = CARTESIAN_POINT ( 'NONE',  ( -33.58253175000000113, 7.275000002731180970, -10.91162601494193041 ) ) ;
#16559 = CARTESIAN_POINT ( 'NONE',  ( 19.06425588902592239, 63.28163166759064495, 19.11951029504763611 ) ) ;
#16560 = CARTESIAN_POINT ( 'NONE',  ( -10.37757302488624411, 72.72500000273119269, -31.93888565452638417 ) ) ;
#16561 = CARTESIAN_POINT ( 'NONE',  ( 7.505752307973351023, 51.81770833333332860, 28.01184896238290278 ) ) ;
#16562 = CARTESIAN_POINT ( 'NONE',  ( 3.980102097228898626E-15, 80.00000000000001421, 32.50000000000000000 ) ) ;
#16563 = CARTESIAN_POINT ( 'NONE',  ( -13.91746824999999887, 77.37500000273116996, 0.000000000000000000 ) ) ;
#16564 = CARTESIAN_POINT ( 'NONE',  ( 10.04305231718578817, 47.39999999999998437, -30.90933677959249337 ) ) ;
#16565 = DIRECTION ( 'NONE',  ( -0.5000000000000002220, 0.000000000000000000, -0.8660254037844384856 ) ) ;
#16566 = CARTESIAN_POINT ( 'NONE',  ( 10.37757302488624767, 57.72500000273117848, 31.93888565452638417 ) ) ;
#16567 = CARTESIAN_POINT ( 'NONE',  ( 7.236395654485755280, 16.72499999726881370, 22.27133577429736988 ) ) ;
#16568 = ORIENTED_EDGE ( 'NONE', *, *, #22998, .F. ) ;
#16569 = CARTESIAN_POINT ( 'NONE',  ( 33.58253175000000113, 64.47500000273120691, -10.91162601494193751 ) ) ;
#16570 = CARTESIAN_POINT ( 'NONE',  ( -27.16883889988623935, 3.325000002731171023, 19.73931689729374739 ) ) ;
#16571 = CARTESIAN_POINT ( 'NONE',  ( -18.94512977948576093, 5.824999997268820451, 13.76444248337722698 ) ) ;
#16572 = CARTESIAN_POINT ( 'NONE',  ( -7.025853678916393008, 26.04204833425729859, 26.06988505166735592 ) ) ;
#16573 = ORIENTED_EDGE ( 'NONE', *, *, #31799, .F. ) ;
#16574 = CARTESIAN_POINT ( 'NONE',  ( -20.75514604977248112, 37.42500000273118843, 28.56700777964554661 ) ) ;
#16575 = CARTESIAN_POINT ( 'NONE',  ( -5.147494310547430452, 68.05125428700922896, -32.49999999999999289 ) ) ;
#16576 = ORIENTED_EDGE ( 'NONE', *, *, #22664, .T. ) ;
#16577 = CARTESIAN_POINT ( 'NONE',  ( 20.50609665440969565, 54.10937499999999289, -20.50609665441004736 ) ) ;
#16578 = CARTESIAN_POINT ( 'NONE',  ( 20.75514604977249178, 60.07500000273119412, 28.56700777964553950 ) ) ;
#16579 = CARTESIAN_POINT ( 'NONE',  ( 5.147494310547434893, 58.55125428154683220, 32.49999999999999289 ) ) ;
#16580 = CARTESIAN_POINT ( 'NONE',  ( -10.37757302488623701, 71.52500000273120406, 31.93888565452638417 ) ) ;
#16581 = CARTESIAN_POINT ( 'NONE',  ( -26.00068869287340334, 31.90885416666666430, 15.01150461594643382 ) ) ;
#16582 = CARTESIAN_POINT ( 'NONE',  ( -19.82091636218621389, 9.199999999999985079, 14.40073868116558842 ) ) ;
#16583 = CARTESIAN_POINT ( 'NONE',  ( 33.58253175000000113, 12.37500000273117351, -4.112674001490185761E-15 ) ) ;
#16584 = CARTESIAN_POINT ( 'NONE',  ( 10.37757302488624056, 16.52500000273118985, -31.93888565452638417 ) ) ;
#16585 = CARTESIAN_POINT ( 'NONE',  ( 5.779280353836490358E-15, 57.00000000546238965, 32.49999999999999289 ) ) ;
#16586 = CARTESIAN_POINT ( 'NONE',  ( 15.00000000000000000, 77.35000000546233423, -4.873795443493596835 ) ) ;
#16587 = CARTESIAN_POINT ( 'NONE',  ( -7.543491769121917656, 41.78607666574268364, -28.00173670424536354 ) ) ;
#16588 = CARTESIAN_POINT ( 'NONE',  ( 8.601468415847520532, 72.07500000273120122, 11.83890561707634781 ) ) ;
#16589 = CARTESIAN_POINT ( 'NONE',  ( 7.505752307973351023, 51.81770833333332860, 28.01184896238290278 ) ) ;
#16590 = DIRECTION ( 'NONE',  ( 0.000000000000000000, 0.000000000000000000, -1.000000000000000000 ) ) ;
#16591 = CARTESIAN_POINT ( 'NONE',  ( -32.50000000000000000, 38.50000000546238965, 0.000000000000000000 ) ) ;
#16592 = CARTESIAN_POINT ( 'NONE',  ( -19.06425588902558133, 68.14024333240935505, 19.11951029504797006 ) ) ;
#16593 = ADVANCED_FACE ( 'NONE', ( #31236 ), #18551, .F. ) ;
#16594 = CARTESIAN_POINT ( 'NONE',  ( 33.58253175000000113, 46.22500000273119269, -10.91162601494193751 ) ) ;
#16595 = CONICAL_SURFACE ( 'NONE', #25894, 32.63512777199724724, 0.7853981633974471688 ) ;
#16596 = CARTESIAN_POINT ( 'NONE',  ( 8.601468415847516980, 78.17500000273120975, -11.83890561707634781 ) ) ;
#16597 = CARTESIAN_POINT ( 'NONE',  ( 33.58253175000000113, 50.37500000273119127, -4.112674001490185761E-15 ) ) ;
#16598 = CARTESIAN_POINT ( 'NONE',  ( 27.16883889988623935, 28.57500000273119412, -19.73931689729374384 ) ) ;
#16599 = CARTESIAN_POINT ( 'NONE',  ( 15.26205751043174885, 16.99999999999997868, 18.11263815609570926 ) ) ;
#16600 = EDGE_CURVE ( 'NONE', #10964, #28042, #19303, .T. ) ;
#16601 = AXIS2_PLACEMENT_3D ( 'NONE', #12606, #5224, #33536 ) ;
#16602 = CARTESIAN_POINT ( 'NONE',  ( -24.20753774853730889, 21.59635416666666430, 13.97622843553634020 ) ) ;
#16603 = CARTESIAN_POINT ( 'NONE',  ( -15.00000000000000000, 76.10000000000000853, 4.873795443493597723 ) ) ;
#16604 =( BOUNDED_CURVE ( )  B_SPLINE_CURVE ( 2, ( #23802, #3365, #26539, #21062, #24303, #24136, #31512, #3033, #8335, #5771, #5603, #10585, #13506 ),
 .UNSPECIFIED., .F., .T. ) 
 B_SPLINE_CURVE_WITH_KNOTS ( ( 3, 2, 2, 2, 2, 2, 3 ),
 ( 0.9551282051282051766, 0.9564102564102564541, 0.9589743589743590091, 0.9615384615384615641, 0.9641025641025641191, 0.9666666666666666741, 0.9679487179487179516 ),
 .UNSPECIFIED. ) 
 CURVE ( )  GEOMETRIC_REPRESENTATION_ITEM ( )  RATIONAL_B_SPLINE_CURVE ( ( 0.9755282581475768211, 0.9755282581475768211, 1.000000000000000000, 0.9510565162951535312, 1.000000000000000000, 0.9510565162951535312, 1.000000000000000000, 0.9510565162951535312, 1.000000000000000000, 0.9510565162951535312, 1.000000000000000000, 0.9755282581475768211, 0.9755282581475768211 ) ) 
 REPRESENTATION_ITEM ( '' )  );
#16605 = CARTESIAN_POINT ( 'NONE',  ( 20.08610463437158344, 74.70000000000000284, 27.64615127144129403 ) ) ;
#16606 = CARTESIAN_POINT ( 'NONE',  ( 33.58253175000000113, 8.125000002731184168, -4.112674001490185761E-15 ) ) ;
#16607 = CARTESIAN_POINT ( 'NONE',  ( 14.47279130897151767, 6.324999997268824892, 19.92008829642072953 ) ) ;
#16608 = DIRECTION ( 'NONE',  ( 0.000000000000000000, 0.000000000000000000, 1.000000000000000000 ) ) ;
#16609 = CARTESIAN_POINT ( 'NONE',  ( -0.04044903255042732459, 31.61680583240936215, -27.95245687107223986 ) ) ;
#16610 = CARTESIAN_POINT ( 'NONE',  ( -20.08610463437157989, 65.69999999999998863, -27.64615127144129758 ) ) ;
#16611 = CARTESIAN_POINT ( 'NONE',  ( 20.75514604977248467, 18.42500000273117777, -28.56700777964554305 ) ) ;
#16612 = CARTESIAN_POINT ( 'NONE',  ( -18.94512977948576093, 6.324999997268820451, 13.76444248337722698 ) ) ;
#16613 = CARTESIAN_POINT ( 'NONE',  ( 19.09188309203694800, 54.96875000000000000, 19.09188309203660694 ) ) ;
#16614 = ORIENTED_EDGE ( 'NONE', *, *, #28032, .F. ) ;
#16615 = CARTESIAN_POINT ( 'NONE',  ( 20.75514604977248467, 54.42500000273117422, -28.56700777964554305 ) ) ;
#16616 = ORIENTED_EDGE ( 'NONE', *, *, #757, .T. ) ;
#16617 = CARTESIAN_POINT ( 'NONE',  ( -15.01150461594642138, 22.45572916666666430, -26.00068869287340334 ) ) ;
#16618 = CARTESIAN_POINT ( 'NONE',  ( 20.47846945139902530, 25.46913166759064140, 20.53372385742071771 ) ) ;
#16619 = TOROIDAL_SURFACE ( 'NONE', #6190, 12.11000150615021553, 1.999999999999992228 ) ;
#16620 = CARTESIAN_POINT ( 'NONE',  ( 19.82091636218621389, 15.94999999453763984, -14.40073868116559197 ) ) ;
#16621 = CARTESIAN_POINT ( 'NONE',  ( 19.82091636218621389, 15.94999999453763984, -14.40073868116559197 ) ) ;
#16622 = CARTESIAN_POINT ( 'NONE',  ( -4.523095164977116484E-15, 8.124999997268826490, 24.62258325217400312 ) ) ;
#16623 = CARTESIAN_POINT ( 'NONE',  ( -27.16883889988624290, 29.17500000273118133, -19.73931689729374028 ) ) ;
#16624 = CARTESIAN_POINT ( 'NONE',  ( 32.50000000000000000, 33.50000000546238255, -3.980102097228898626E-15 ) ) ;
#16625 = CARTESIAN_POINT ( 'NONE',  ( 32.50000000000000711, 72.90000000000000568, 10.55989012756945122 ) ) ;
#16626 = FACE_OUTER_BOUND ( 'NONE', #7533, .T. ) ;
#16627 = DIRECTION ( 'NONE',  ( -0.000000000000000000, -1.000000000000000000, -0.000000000000000000 ) ) ;
#16628 = CARTESIAN_POINT ( 'NONE',  ( -28.02196122052045268, 54.11496500092397355, 7.468012846824790607 ) ) ;
#16629 = CARTESIAN_POINT ( 'NONE',  ( 10.37757302488624056, 40.77500000273118275, -31.93888565452638417 ) ) ;
#16630 = CARTESIAN_POINT ( 'NONE',  ( -23.41746825000000243, 8.024999997268801977, -7.608796670333730638 ) ) ;
#16631 = CARTESIAN_POINT ( 'NONE',  ( -32.50000000000000000, 18.00000000000001421, 0.000000000000000000 ) ) ;
#16632 = CARTESIAN_POINT ( 'NONE',  ( -4.732186688966233175E-15, 13.50000000000001066, 25.76082449383753925 ) ) ;
#16633 = CARTESIAN_POINT ( 'NONE',  ( 13.94119854578893580, 31.90326416574268364, -24.22776226481265383 ) ) ;
#16634 = CARTESIAN_POINT ( 'NONE',  ( -20.75514604977248823, 64.82500000273120122, -28.56700777964554305 ) ) ;
#16635 = CARTESIAN_POINT ( 'NONE',  ( 6.486482029760648627E-15, 51.87500000273119127, 35.31076352940722529 ) ) ;
#16636 = CARTESIAN_POINT ( 'NONE',  ( 23.41746824999999887, 12.72499999726882791, -7.608796670333727974 ) ) ;
#16637 = CARTESIAN_POINT ( 'NONE',  ( 20.08610463437158344, 39.20000000546237118, 27.64615127144129403 ) ) ;
#16638 = CARTESIAN_POINT ( 'NONE',  ( 33.58253175000000823, 4.025000002731196957, 10.91162601494192863 ) ) ;
#16639 = EDGE_CURVE ( 'NONE', #1221, #21685, #16299, .T. ) ;
#16640 = EDGE_CURVE ( 'NONE', #19648, #21685, #28871, .T. ) ;
#16641 = CARTESIAN_POINT ( 'NONE',  ( 19.11951029504763611, 34.92225666759063074, -19.06425588902591173 ) ) ;
#16642 = CARTESIAN_POINT ( 'NONE',  ( 18.59695232317482905, 16.99999999999998224, -14.25184196307220219 ) ) ;
#16643 = CARTESIAN_POINT ( 'NONE',  ( 0.3462681986485906527, 52.00000000000000000, 33.37691080753738504 ) ) ;
#16644 = CARTESIAN_POINT ( 'NONE',  ( -10.37757302488624411, 30.72500000273119269, -31.93888565452638417 ) ) ;
#16645 = CARTESIAN_POINT ( 'NONE',  ( 5.779280353836490358E-15, 56.49999999999998579, 32.49999999999999289 ) ) ;
#16646 = CARTESIAN_POINT ( 'NONE',  ( -32.50000000000000000, 58.60000000546236265, 10.55989012756946366 ) ) ;
#16647 = VECTOR ( 'NONE', #23361, 1000.000000000000000 ) ;
#16648 = CARTESIAN_POINT ( 'NONE',  ( 19.82091636218621034, 13.80000000000000604, 14.40073868116559730 ) ) ;
#16649 = CARTESIAN_POINT ( 'NONE',  ( -7.543491769121917656, 55.53607666574269075, -28.00173670424536354 ) ) ;
#16650 = CARTESIAN_POINT ( 'NONE',  ( -32.50000000000000000, 50.60000000546236265, 10.55989012756946366 ) ) ;
#16651 = CARTESIAN_POINT ( 'NONE',  ( 5.147494310547426899, 49.44874571845315359, -32.50000000000000000 ) ) ;
#16652 =( NAMED_UNIT ( * ) SI_UNIT ( $, .STERADIAN. ) SOLID_ANGLE_UNIT ( ) );
#16653 = CARTESIAN_POINT ( 'NONE',  ( 6.988114217767829928, 22.88541666666666430, -26.07999730980489872 ) ) ;
#16654 = CARTESIAN_POINT ( 'NONE',  ( 33.58253175000000113, 78.22500000273119269, -10.91162601494193751 ) ) ;
#16655 = CARTESIAN_POINT ( 'NONE',  ( -26.00068869287340334, 31.90885416666666430, 15.01150461594643382 ) ) ;
#16656 = CYLINDRICAL_SURFACE ( 'NONE', #18486, 30.00000000000004974 ) ;
#16657 = ORIENTED_EDGE ( 'NONE', *, *, #29829, .F. ) ;
#16658 = CARTESIAN_POINT ( 'NONE',  ( 25.98046417659858420, 52.82590250092398065, 15.04653450569292872 ) ) ;
#16659 = CARTESIAN_POINT ( 'NONE',  ( -32.50000000000000000, 12.50000000546237722, 0.000000000000000000 ) ) ;
#16660 = CARTESIAN_POINT ( 'NONE',  ( -7.505752307973343918, 60.41145833333332149, -28.01184896238290989 ) ) ;
#16661 = CARTESIAN_POINT ( 'NONE',  ( -20.08610463437156923, 46.80000000546235839, 27.64615127144130113 ) ) ;
#16662 = CARTESIAN_POINT ( 'NONE',  ( 10.37757302488624767, 47.97500000273119269, 31.93888565452638417 ) ) ;
#16663 = CARTESIAN_POINT ( 'NONE',  ( 10.04305231718578817, 47.90000000546238113, -30.90933677959249337 ) ) ;
#16664 = CARTESIAN_POINT ( 'NONE',  ( 8.601468415847516980, 80.67500000273118133, -11.83890561707634781 ) ) ;
#16665 = CARTESIAN_POINT ( 'NONE',  ( -33.58253175000000113, 37.02500000273117564, -10.91162601494193218 ) ) ;
#16666 = CARTESIAN_POINT ( 'NONE',  ( -1.053607264507113999E-13, 63.00000000546238255, 32.50000000000000711 ) ) ;
#16667 = CARTESIAN_POINT ( 'NONE',  ( 33.58253175000000113, 60.47500000273118559, -10.91162601494193751 ) ) ;
#16668 = AXIS2_PLACEMENT_3D ( 'NONE', #33194, #9697, #14681 ) ;
#16669 = CARTESIAN_POINT ( 'NONE',  ( 32.50000000000000711, 40.89999999999998437, 10.55989012756945122 ) ) ;
#16670 = CARTESIAN_POINT ( 'NONE',  ( -7.236395654485757944, 13.22499999726881015, -22.27133577429736988 ) ) ;
#16671 = CARTESIAN_POINT ( 'NONE',  ( -10.37757302488623701, 1.775000002731175197, 31.93888565452638417 ) ) ;
#16672 = LINE ( 'NONE', #32769, #11809 ) ;
#16673 = CARTESIAN_POINT ( 'NONE',  ( 8.601468415847516980, 76.67500000273118133, -11.83890561707634603 ) ) ;
#16674 = CARTESIAN_POINT ( 'NONE',  ( 10.37757302488624056, 72.77500000273118985, -31.93888565452638417 ) ) ;
#16675 = CARTESIAN_POINT ( 'NONE',  ( 0.000000000000000000, 80.00000000000001421, 0.000000000000000000 ) ) ;
#16676 = CARTESIAN_POINT ( 'NONE',  ( -27.16883889988624290, 71.17500000273118133, -19.73931689729374028 ) ) ;
#16677 = ORIENTED_EDGE ( 'NONE', *, *, #15026, .T. ) ;
#16678 = CARTESIAN_POINT ( 'NONE',  ( -19.82091636218621034, 4.549999994537618164, -14.40073868116559552 ) ) ;
#16679 = CARTESIAN_POINT ( 'NONE',  ( 19.09188309203694800, 65.28125000000000000, 19.09188309203660694 ) ) ;
#16680 = LINE ( 'NONE', #22167, #24485 ) ;
#16681 = CARTESIAN_POINT ( 'NONE',  ( 27.16883889988623935, 44.32500000273119412, -19.73931689729374384 ) ) ;
#16682 = CARTESIAN_POINT ( 'NONE',  ( 33.58253175000000113, 8.375000002731184168, -4.112674001490185761E-15 ) ) ;
#16683 = CARTESIAN_POINT ( 'NONE',  ( -10.37757302488624411, 64.97500000273119269, -31.93888565452638417 ) ) ;
#16684 = CARTESIAN_POINT ( 'NONE',  ( -24.20753774853756823, 46.23177083333332149, -13.97622843553588723 ) ) ;
#16685 = CARTESIAN_POINT ( 'NONE',  ( 14.97647472619947351, 39.36236083425731636, 26.02091320914850314 ) ) ;
#16686 = CARTESIAN_POINT ( 'NONE',  ( -7.543491769121917656, 24.59857666574268720, -28.00173670424536354 ) ) ;
#16687 = CARTESIAN_POINT ( 'NONE',  ( -10.04305231718579172, 70.10000000546239107, -30.90933677959248982 ) ) ;
#16688 = CARTESIAN_POINT ( 'NONE',  ( 8.601468415847516980, 80.17500000273113869, -11.83890561707634781 ) ) ;
#16689 = AXIS2_PLACEMENT_3D ( 'NONE', #3476, #3810, #13947 ) ;
#16690 = CARTESIAN_POINT ( 'NONE',  ( 26.06988505166722803, 59.83295166574269075, -7.025853678916862854 ) ) ;
#16691 = CARTESIAN_POINT ( 'NONE',  ( 18.94512977948576093, 16.82499999726880091, -13.76444248337722875 ) ) ;
#16692 = CARTESIAN_POINT ( 'NONE',  ( 32.50000000000000000, 59.00000000000000000, -3.980102097228898626E-15 ) ) ;
#16693 = ORIENTED_EDGE ( 'NONE', *, *, #29548, .F. ) ;
#16694 = CARTESIAN_POINT ( 'NONE',  ( -33.58253175000000113, 47.27500000273116143, -10.91162601494193218 ) ) ;
#16695 =( BOUNDED_CURVE ( )  B_SPLINE_CURVE ( 2, ( #32742, #838, #19057, #26775, #16648, #1339, #24859, #29496, #11320, #19556, #27102, #3264, #6508 ),
 .UNSPECIFIED., .F., .T. ) 
 B_SPLINE_CURVE_WITH_KNOTS ( ( 3, 2, 2, 2, 2, 2, 3 ),
 ( 0.7500000000000000000, 0.7555555555555555358, 0.7666666666666667185, 0.7777777777777777901, 0.7888888888888888618, 0.8000000000000000444, 0.8055555555555555802 ),
 .UNSPECIFIED. ) 
 CURVE ( )  GEOMETRIC_REPRESENTATION_ITEM ( )  RATIONAL_B_SPLINE_CURVE ( ( 0.9755282581475768211, 0.9755282581475768211, 1.000000000000000000, 0.9510565162951535312, 1.000000000000000000, 0.9510565162951535312, 1.000000000000000000, 0.9510565162951535312, 1.000000000000000000, 0.9510565162951535312, 1.000000000000000000, 0.9755282581475768211, 0.9755282581475768211 ) ) 
 REPRESENTATION_ITEM ( '' )  );
#16696 = CARTESIAN_POINT ( 'NONE',  ( -7.236395654485757944, 3.724999997268802154, -22.27133577429736988 ) ) ;
#16697 = CARTESIAN_POINT ( 'NONE',  ( 14.01125832528286352, 48.52902750092398065, -24.18731323226246843 ) ) ;
#16698 = CARTESIAN_POINT ( 'NONE',  ( 26.29305231718579350, 29.30000000546238681, 19.10302069950537529 ) ) ;
#16699 = VERTEX_POINT ( 'NONE', #29831 ) ;
#16700 = CARTESIAN_POINT ( 'NONE',  ( -2.162160676586881955E-15, 20.62500000273119483, -35.31076352940723240 ) ) ;
#16701 = ADVANCED_FACE ( 'NONE', ( #27096 ), #21625, .T. ) ;
#16702 = CARTESIAN_POINT ( 'NONE',  ( 7.505752307973351023, 31.19270833333333215, 28.01184896238290278 ) ) ;
#16703 = ORIENTED_EDGE ( 'NONE', *, *, #24751, .T. ) ;
#16704 = DIRECTION ( 'NONE',  ( 0.8660254037844402619, 0.4999999999999970579, -0.000000000000000000 ) ) ;
#16705 = CARTESIAN_POINT ( 'NONE',  ( -33.58253175000000113, 53.22500000273118559, 10.91162601494193929 ) ) ;
#16706 = CARTESIAN_POINT ( 'NONE',  ( 26.00068869287367335, 54.82552083333331439, 15.01150461594596308 ) ) ;
#16707 = CARTESIAN_POINT ( 'NONE',  ( -2.092463501923844636E-15, 14.00000000546237899, -34.17252228774368916 ) ) ;
#16708 = CARTESIAN_POINT ( 'NONE',  ( -1.778240108872766143E-15, 45.49999999999999289, -32.49999999999999289 ) ) ;
#16709 = CARTESIAN_POINT ( 'NONE',  ( 14.47279130897151767, 12.82499999726882400, 19.92008829642072953 ) ) ;
#16710 =( GEOMETRIC_REPRESENTATION_CONTEXT ( 3 ) GLOBAL_UNCERTAINTY_ASSIGNED_CONTEXT ( ( #3100 ) ) GLOBAL_UNIT_ASSIGNED_CONTEXT ( ( #27441, #19393, #13736 ) ) REPRESENTATION_CONTEXT ( 'NONE', 'WORKASPACE' ) );
#16711 = CARTESIAN_POINT ( 'NONE',  ( -32.50000000000000000, 57.99999999999999289, 0.000000000000000000 ) ) ;
#16712 = CARTESIAN_POINT ( 'NONE',  ( -20.75514604977248823, 25.07500000273120122, -28.56700777964554305 ) ) ;
#16713 = CARTESIAN_POINT ( 'NONE',  ( -32.50000000000000000, 24.60000000546236620, 10.55989012756946366 ) ) ;
#16714 = CARTESIAN_POINT ( 'NONE',  ( 26.06988505166722803, 18.58295166574268364, -7.025853678916862854 ) ) ;
#16715 = CARTESIAN_POINT ( 'NONE',  ( -4.300734207923759378, 76.47500000273119269, -13.23629886949340495 ) ) ;
#16716 = CARTESIAN_POINT ( 'NONE',  ( -1.778240108872766143E-15, 65.50000000000000000, -32.49999999999999289 ) ) ;
#16717 = CARTESIAN_POINT ( 'NONE',  ( -26.29305231718578995, 28.70000000546238539, 19.10302069950538595 ) ) ;
#16718 = CARTESIAN_POINT ( 'NONE',  ( -20.08610463437157989, 9.699999999999999289, -27.64615127144129758 ) ) ;
#16719 = ORIENTED_EDGE ( 'NONE', *, *, #30107, .F. ) ;
#16720 = CARTESIAN_POINT ( 'NONE',  ( 14.47279130897151589, 8.824999997268804464, 19.92008829642072953 ) ) ;
#16721 = CARTESIAN_POINT ( 'NONE',  ( -13.91746824999999532, 74.77500000273117564, -4.522059556121115875 ) ) ;
#16722 = CARTESIAN_POINT ( 'NONE',  ( -26.07999730980477437, 45.80208333333333570, 6.988114217768305103 ) ) ;
#16723 = CARTESIAN_POINT ( 'NONE',  ( 20.75514604977249178, 15.82500000273117102, 28.56700777964553950 ) ) ;
#16724 = CARTESIAN_POINT ( 'NONE',  ( -20.75514604977248112, 67.42500000273118133, 28.56700777964554661 ) ) ;
#16725 = CARTESIAN_POINT ( 'NONE',  ( 10.37757302488624767, 29.97500000273119269, 31.93888565452638417 ) ) ;
#16726 = CARTESIAN_POINT ( 'NONE',  ( -10.37757302488623701, 19.77500000273117564, 31.93888565452638417 ) ) ;
#16727 = CARTESIAN_POINT ( 'NONE',  ( 33.58253175000000113, 6.375000002731168181, -4.112674001490185761E-15 ) ) ;
#16728 = CARTESIAN_POINT ( 'NONE',  ( 0.04044903254992426173, 10.43006916759064495, -30.02300923189239867 ) ) ;
#16729 = CARTESIAN_POINT ( 'NONE',  ( 26.00068869287367335, 58.26302083333332149, 15.01150461594596308 ) ) ;
#16730 = LINE ( 'NONE', #6251, #13284 ) ;
#16731 = CARTESIAN_POINT ( 'NONE',  ( 4.300734207923757602, 74.77500000273118985, -13.23629886949340673 ) ) ;
#16732 = CARTESIAN_POINT ( 'NONE',  ( 20.08610463437157279, 49.29999999999998295, -27.64615127144129758 ) ) ;
#16733 = CARTESIAN_POINT ( 'NONE',  ( 32.50000000000000000, 63.10000000000001563, -10.55989012756945833 ) ) ;
#16734 = CARTESIAN_POINT ( 'NONE',  ( 10.37757302488624056, 48.52500000273118985, -31.93888565452638417 ) ) ;
#16735 = CARTESIAN_POINT ( 'NONE',  ( 23.41746824999999887, 13.12499999726882116, 0.000000000000000000 ) ) ;
#16736 = ORIENTED_EDGE ( 'NONE', *, *, #9990, .T. ) ;
#16737 = CARTESIAN_POINT ( 'NONE',  ( 6.486482029760649416E-15, 67.87500000273116996, 35.31076352940723240 ) ) ;
#16738 = CARTESIAN_POINT ( 'NONE',  ( -10.04305231718578462, 2.400000000000013234, 30.90933677959249337 ) ) ;
#16739 = CARTESIAN_POINT ( 'NONE',  ( 7.236395654485760609, 7.024999997268799312, -22.27133577429736633 ) ) ;
#16740 = CARTESIAN_POINT ( 'NONE',  ( -26.09010956794232428, 26.61496500092397355, 6.950374756619732253 ) ) ;
#16741 = VERTEX_POINT ( 'NONE', #3759 ) ;
#16742 = CARTESIAN_POINT ( 'NONE',  ( -2.162160676586881955E-15, 36.62500000273119127, -35.31076352940723240 ) ) ;
#16743 = CARTESIAN_POINT ( 'NONE',  ( -26.29305231718579350, 42.30000000546238681, -19.10302069950537884 ) ) ;
#16744 = ORIENTED_EDGE ( 'NONE', *, *, #25075, .T. ) ;
#16745 = CARTESIAN_POINT ( 'NONE',  ( -26.00068869287368756, 53.10677083333331439, -15.01150461594595775 ) ) ;
#16746 = CARTESIAN_POINT ( 'NONE',  ( -20.75514604977248823, 59.07500000273119412, -28.56700777964554305 ) ) ;
#16747 = CARTESIAN_POINT ( 'NONE',  ( 4.635254915624209993, 75.65000000546234560, -14.26584774442730463 ) ) ;
#16748 = CARTESIAN_POINT ( 'NONE',  ( 33.58253175000000113, 76.12500000273119838, -4.112674001490185761E-15 ) ) ;
#16749 = CARTESIAN_POINT ( 'NONE',  ( 30.02300923189239512, 30.47656250000000355, -2.619432448724977703E-13 ) ) ;
#16750 = CARTESIAN_POINT ( 'NONE',  ( 7.570916362186207671, 5.599999999999994316, 23.30088464923126779 ) ) ;
#16751 = CARTESIAN_POINT ( 'NONE',  ( 33.58253175000000113, 4.475000002731183812, -10.91162601494193751 ) ) ;
#16752 = CARTESIAN_POINT ( 'NONE',  ( -10.37757302488623701, 17.52500000273118985, 31.93888565452638417 ) ) ;
#16753 = DIRECTION ( 'NONE',  ( 0.000000000000000000, -1.000000000000000000, 0.000000000000000000 ) ) ;
#16754 = CARTESIAN_POINT ( 'NONE',  ( -28.02196122052058413, 48.08815999907601935, -7.468012846824272799 ) ) ;
#16755 = CARTESIAN_POINT ( 'NONE',  ( -4.300734207923759378, 72.97500000273119269, -13.23629886949340495 ) ) ;
#16756 = CARTESIAN_POINT ( 'NONE',  ( -30.02300923189239867, 52.82031249999998579, 2.654126918244514854E-13 ) ) ;
#16757 = CARTESIAN_POINT ( 'NONE',  ( -7.570916362186210335, 16.34999999453762243, -23.30088464923126779 ) ) ;
#16758 = CARTESIAN_POINT ( 'NONE',  ( 5.147494310547426899, 49.94874572391552903, -32.50000000000000000 ) ) ;
#16759 = CARTESIAN_POINT ( 'NONE',  ( 14.01125832528330051, 67.42409749907601224, 24.18731323226221974 ) ) ;
#16760 = CARTESIAN_POINT ( 'NONE',  ( -20.75514604977248823, 34.82500000273118701, -28.56700777964554305 ) ) ;
#16761 = CARTESIAN_POINT ( 'NONE',  ( -11.25946833292375793, 73.07500000273120122, 8.180482586598737171 ) ) ;
#16762 = CARTESIAN_POINT ( 'NONE',  ( 33.58253175000000823, 52.27500000273118985, 10.91162601494192863 ) ) ;
#16763 = CARTESIAN_POINT ( 'NONE',  ( 20.75514604977249178, 30.07500000273118701, 28.56700777964553950 ) ) ;
#16764 = CARTESIAN_POINT ( 'NONE',  ( 16.34000363327193384, 17.00000000000000000, 17.09839857644911731 ) ) ;
#16765 = CARTESIAN_POINT ( 'NONE',  ( -19.09188309203660694, 21.45312499999999645, 19.09188309203694800 ) ) ;
#16766 = FACE_OUTER_BOUND ( 'NONE', #2650, .T. ) ;
#16767 = CARTESIAN_POINT ( 'NONE',  ( -4.635254915624211769, 75.59999999999999432, -14.26584774442730286 ) ) ;
#16768 = CARTESIAN_POINT ( 'NONE',  ( 20.08610463437157279, 65.29999999999999716, -27.64615127144129758 ) ) ;
#16769 = CARTESIAN_POINT ( 'NONE',  ( -20.75514604977248823, 6.825000002731195892, -28.56700777964554305 ) ) ;
#16770 = CARTESIAN_POINT ( 'NONE',  ( 23.41746824999999887, 2.524999997268799312, 7.608796670333735079 ) ) ;
#16771 = CARTESIAN_POINT ( 'NONE',  ( -20.47846945139866648, 23.45274333240935150, 20.53372385742108008 ) ) ;
#16772 = CARTESIAN_POINT ( 'NONE',  ( -15.14183272437242778, 11.04999999453761284, 20.84094480462497856 ) ) ;
#16773 = CARTESIAN_POINT ( 'NONE',  ( -24.22776226481266448, 27.60638916574269075, -13.94119854578892514 ) ) ;
#16774 = CARTESIAN_POINT ( 'NONE',  ( -12.13525491562421088, 76.05000000546239391, -8.816778784387096835 ) ) ;
#16775 = CARTESIAN_POINT ( 'NONE',  ( -20.75514604977248823, 20.82500000273119056, -28.56700777964554305 ) ) ;
#16776 = CARTESIAN_POINT ( 'NONE',  ( 18.94512977948576093, 5.324999997268820451, -13.76444248337722875 ) ) ;
#16777 = CARTESIAN_POINT ( 'NONE',  ( -19.09188309203694445, 56.68749999999998579, -19.09188309203661049 ) ) ;
#16778 = ORIENTED_EDGE ( 'NONE', *, *, #28224, .T. ) ;
#16779 = CARTESIAN_POINT ( 'NONE',  ( 27.16883889988624290, 57.92500000273119554, 19.73931689729373673 ) ) ;
#16780 = CARTESIAN_POINT ( 'NONE',  ( 33.58253175000000823, 30.27500000273118630, 10.91162601494192863 ) ) ;
#16781 = EDGE_CURVE ( 'NONE', #7065, #8583, #11378, .T. ) ;
#16782 = VERTEX_POINT ( 'NONE', #21792 ) ;
#16783 = CARTESIAN_POINT ( 'NONE',  ( 7.505752307973351023, 24.31770833333332504, 28.01184896238290278 ) ) ;
#16784 = CARTESIAN_POINT ( 'NONE',  ( -20.53372385742071771, 22.89100666759064495, 20.47846945139902530 ) ) ;
#16785 = CARTESIAN_POINT ( 'NONE',  ( -32.50000000000000000, 9.899999999999979039, -10.55989012756945300 ) ) ;
#16786 = CARTESIAN_POINT ( 'NONE',  ( 7.570916362186213000, 14.14999999453761603, -23.30088464923126423 ) ) ;
#16787 = ADVANCED_FACE ( 'NONE', ( #6157 ), #21458, .T. ) ;
#16788 = CARTESIAN_POINT ( 'NONE',  ( 18.94512977948575738, 8.424999997268811214, 13.76444248337723408 ) ) ;
#16789 = CARTESIAN_POINT ( 'NONE',  ( 27.16883889988623935, 30.57500000273119412, -19.73931689729374384 ) ) ;
#16790 = CARTESIAN_POINT ( 'NONE',  ( 10.04305231718579705, 33.10000000546236976, 30.90933677959248982 ) ) ;
#16791 = CARTESIAN_POINT ( 'NONE',  ( 6.277390505771533514E-15, 74.50000000000000000, 34.17252228774368916 ) ) ;
#16792 = CARTESIAN_POINT ( 'NONE',  ( -10.04305231718578462, 6.900000005462370467, 30.90933677959249337 ) ) ;
#16793 = CARTESIAN_POINT ( 'NONE',  ( -7.570916362186215665, 11.39999999999999325, 23.30088464923126423 ) ) ;
#16794 = CARTESIAN_POINT ( 'NONE',  ( -28.00173670424549499, 54.40142333425730925, -7.543491769121417612 ) ) ;
#16795 = CARTESIAN_POINT ( 'NONE',  ( -2.162160676586881955E-15, 38.87500000273120548, -35.31076352940723240 ) ) ;
#16796 = CARTESIAN_POINT ( 'NONE',  ( 15.01150461594643382, 24.17447916666666075, 26.00068869287340334 ) ) ;
#16797 =( BOUNDED_CURVE ( )  B_SPLINE_CURVE ( 2, ( #15599, #31364, #5115, #15248, #2191, #21087, #7687, #7521, #292, #18515, #23316, #12665, #2887 ),
 .UNSPECIFIED., .F., .T. ) 
 B_SPLINE_CURVE_WITH_KNOTS ( ( 3, 2, 2, 2, 2, 2, 3 ),
 ( 0.4722222222222222099, 0.4777777777777778012, 0.4888888888888888729, 0.5000000000000000000, 0.5111111111111110716, 0.5222222222222222543, 0.5277777777777777901 ),
 .UNSPECIFIED. ) 
 CURVE ( )  GEOMETRIC_REPRESENTATION_ITEM ( )  RATIONAL_B_SPLINE_CURVE ( ( 0.9755282581475765991, 0.9755282581475765991, 1.000000000000000000, 0.9510565162951535312, 1.000000000000000000, 0.9510565162951535312, 1.000000000000000000, 0.9510565162951535312, 1.000000000000000000, 0.9510565162951535312, 1.000000000000000000, 0.9755282581475768211, 0.9755282581475768211 ) ) 
 REPRESENTATION_ITEM ( '' )  );
#16798 = SHAPE_REPRESENTATION_RELATIONSHIP ( 'NONE' , 'NONE' ,  #3268, #29162 ) ;
#16799 = CARTESIAN_POINT ( 'NONE',  ( -23.41746825000000598, 8.224999997268824359, 7.608796670333726198 ) ) ;
#16800 = CARTESIAN_POINT ( 'NONE',  ( 26.29305231718578995, 17.19999999999999218, -19.10302069950538240 ) ) ;
#16801 = CARTESIAN_POINT ( 'NONE',  ( -15.14183272437242600, 9.299999999999998934, 20.84094480462497856 ) ) ;
#16802 = CARTESIAN_POINT ( 'NONE',  ( 14.01125832528330051, 46.79909749907603356, 24.18731323226221974 ) ) ;
#16803 =( BOUNDED_CURVE ( )  B_SPLINE_CURVE ( 2, ( #32344, #3696, #16747, #19488, #18993, #777, #5938, #6441, #24626, #11419, #29437, #1099, #8838 ),
 .UNSPECIFIED., .F., .T. ) 
 B_SPLINE_CURVE_WITH_KNOTS ( ( 3, 2, 2, 2, 2, 2, 3 ),
 ( 0.4500000000000000111, 0.4600000000000000200, 0.4799999999999999822, 0.5000000000000000000, 0.5200000000000000178, 0.5400000000000000355, 0.5500000000000000444 ),
 .UNSPECIFIED. ) 
 CURVE ( )  GEOMETRIC_REPRESENTATION_ITEM ( )  RATIONAL_B_SPLINE_CURVE ( ( 0.9755282581475768211, 0.9755282581475768211, 1.000000000000000000, 0.9510565162951535312, 1.000000000000000000, 0.9510565162951535312, 1.000000000000000000, 0.9510565162951535312, 1.000000000000000000, 0.9510565162951535312, 1.000000000000000000, 0.9755282581475768211, 0.9755282581475768211 ) ) 
 REPRESENTATION_ITEM ( '' )  );
#16804 = CARTESIAN_POINT ( 'NONE',  ( -20.75514604977248112, 63.42500000273118133, 28.56700777964554661 ) ) ;
#16805 = CARTESIAN_POINT ( 'NONE',  ( -33.58253175000000113, 45.27500000273117564, -10.91162601494193041 ) ) ;
#16806 = CARTESIAN_POINT ( 'NONE',  ( -7.236395654485757944, 9.224999997268806595, -22.27133577429736988 ) ) ;
#16807 = CARTESIAN_POINT ( 'NONE',  ( -3.712076227271900841E-14, 8.499999999999994671, -24.50000000000000000 ) ) ;
#16808 = CARTESIAN_POINT ( 'NONE',  ( 20.75514604977248467, 8.425000002731204418, -28.56700777964554305 ) ) ;
#16809 = CARTESIAN_POINT ( 'NONE',  ( 0.04044903254993986036, 41.36756916759064495, -27.95245687107223986 ) ) ;
#16810 = CARTESIAN_POINT ( 'NONE',  ( 26.29305231718578995, 25.70000000546238184, -19.10302069950538240 ) ) ;
#16811 = CARTESIAN_POINT ( 'NONE',  ( -31.32135535759083567, 52.00000000000002132, 9.352374566761922026 ) ) ;
#16812 = UNCERTAINTY_MEASURE_WITH_UNIT (LENGTH_MEASURE( 1.000000000000000082E-05 ), #6530, 'distance_accuracy_value', 'NONE');
#16813 = CARTESIAN_POINT ( 'NONE',  ( 33.58253175000000113, 28.12500000273120193, -4.112674001490185761E-15 ) ) ;
#16814 = CARTESIAN_POINT ( 'NONE',  ( -5.147494310547423346, 18.94874572391552903, 32.50000000000000000 ) ) ;
#16815 = DIRECTION ( 'NONE',  ( 0.000000000000000000, 0.000000000000000000, -1.000000000000000000 ) ) ;
#16816 = FACE_OUTER_BOUND ( 'NONE', #26828, .T. ) ;
#16817 = CARTESIAN_POINT ( 'NONE',  ( -28.02196122052058413, 58.40065999907601935, -7.468012846824272799 ) ) ;
#16818 = CARTESIAN_POINT ( 'NONE',  ( -2.092463501923844636E-15, 46.00000000546238965, -34.17252228774368916 ) ) ;
#16819 = CARTESIAN_POINT ( 'NONE',  ( 1.469576158976824144E-15, 102.0000000000000284, 12.00000000000000178 ) ) ;
#16820 = CARTESIAN_POINT ( 'NONE',  ( 6.988114217767829928, 29.76041666666666430, -26.07999730980489872 ) ) ;
#16821 = ORIENTED_EDGE ( 'NONE', *, *, #23007, .F. ) ;
#16822 = CARTESIAN_POINT ( 'NONE',  ( 33.58253175000000823, 76.02500000273118985, 10.91162601494192863 ) ) ;
#16823 = CARTESIAN_POINT ( 'NONE',  ( -20.50609665440969209, 35.20312500000000000, 20.50609665441005092 ) ) ;
#16824 = EDGE_CURVE ( 'NONE', #14840, #16549, #2368, .T. ) ;
#16825 = DIRECTION ( 'NONE',  ( 1.000000000000000000, -0.000000000000000000, 0.000000000000000000 ) ) ;
#16826 = VERTEX_POINT ( 'NONE', #1505 ) ;
#16827 = CARTESIAN_POINT ( 'NONE',  ( -28.02196122052045268, 50.67746500092398065, 7.468012846824790607 ) ) ;
#16828 = CARTESIAN_POINT ( 'NONE',  ( 10.04305231718578817, 11.90000000546235981, -30.90933677959249337 ) ) ;
#16829 = AXIS2_PLACEMENT_3D ( 'NONE', #32292, #9458, #8786 ) ;
#16830 = CARTESIAN_POINT ( 'NONE',  ( 20.50609665440969565, 60.98437499999999289, -20.50609665441004736 ) ) ;
#16831 = CARTESIAN_POINT ( 'NONE',  ( -10.04305231718579172, 46.10000000546238397, -30.90933677959248982 ) ) ;
#16832 = CARTESIAN_POINT ( 'NONE',  ( -10.37757302488623701, 49.77500000273118985, 31.93888565452638417 ) ) ;
#16833 = CARTESIAN_POINT ( 'NONE',  ( -20.08610463437156923, 48.80000000546235128, 27.64615127144130113 ) ) ;
#16834 = CARTESIAN_POINT ( 'NONE',  ( 11.25946833292375793, 72.57500000273120122, -8.180482586598735395 ) ) ;
#16835 = CARTESIAN_POINT ( 'NONE',  ( -20.75514604977248112, 31.42500000273120619, 28.56700777964554661 ) ) ;
#16836 = CARTESIAN_POINT ( 'NONE',  ( 3.880418787951172011, 11.55125428154683576, 24.49999999999998579 ) ) ;
#16837 = CARTESIAN_POINT ( 'NONE',  ( 33.58253175000000113, 62.37500000273119127, -4.112674001490185761E-15 ) ) ;
#16838 = CARTESIAN_POINT ( 'NONE',  ( -32.50000000000000000, 37.99999999999999289, 0.000000000000000000 ) ) ;
#16839 = CARTESIAN_POINT ( 'NONE',  ( -32.50000000000000000, 36.10000000000000142, 10.55989012756946366 ) ) ;
#16840 = CARTESIAN_POINT ( 'NONE',  ( 23.41746825000000243, 14.52499999726882685, 7.608796670333735079 ) ) ;
#16841 = CARTESIAN_POINT ( 'NONE',  ( -2.162160676586881955E-15, 4.875000002731200155, -35.31076352940723240 ) ) ;
#16842 = DIRECTION ( 'NONE',  ( -1.000000000000000000, -1.122425893913996568E-16, 0.000000000000000000 ) ) ;
#16843 = CARTESIAN_POINT ( 'NONE',  ( -13.91746824999999532, 81.27500000273117564, -4.522059556121115875 ) ) ;
#16844 = CARTESIAN_POINT ( 'NONE',  ( -2.162160676586882350E-15, 64.87500000273119838, -35.31076352940722529 ) ) ;
#16845 = LINE ( 'NONE', #11349, #18788 ) ;
#16846 = CARTESIAN_POINT ( 'NONE',  ( -27.16883889988623935, 63.57500000273117990, 19.73931689729374739 ) ) ;
#16847 = ORIENTED_EDGE ( 'NONE', *, *, #16412, .T. ) ;
#16848 = CARTESIAN_POINT ( 'NONE',  ( 15.14183272437242245, 6.049999994537625270, -20.84094480462497856 ) ) ;
#16849 = CARTESIAN_POINT ( 'NONE',  ( -13.97622843553588901, 65.99739583333334281, 24.20753774853756823 ) ) ;
#16850 = CARTESIAN_POINT ( 'NONE',  ( 9.270509831248425314, 74.70000000000000284, 12.75976212528059683 ) ) ;
#16851 = CARTESIAN_POINT ( 'NONE',  ( -2.162160676586881955E-15, 46.62500000273119127, -35.31076352940723240 ) ) ;
#16852 = CARTESIAN_POINT ( 'NONE',  ( -27.16883889988623935, 11.57500000273119234, 19.73931689729374739 ) ) ;
#16853 = CARTESIAN_POINT ( 'NONE',  ( -27.16883889988624290, 63.17500000273117422, -19.73931689729374028 ) ) ;
#16854 = CARTESIAN_POINT ( 'NONE',  ( -13.97622843553632777, 46.51822916666666430, -24.20753774853731599 ) ) ;
#16855 = CARTESIAN_POINT ( 'NONE',  ( 7.543491769121427382, 34.63579833425730925, -28.00173670424548433 ) ) ;
#16856 = CARTESIAN_POINT ( 'NONE',  ( 14.97647472619900455, 25.02826416574268720, -26.02091320914876960 ) ) ;
#16857 = CARTESIAN_POINT ( 'NONE',  ( 10.04305231718578817, 65.90000000546237402, -30.90933677959249337 ) ) ;
#16858 = CARTESIAN_POINT ( 'NONE',  ( 0.000000000000000000, 0.000000000000000000, 0.000000000000000000 ) ) ;
#16859 = CARTESIAN_POINT ( 'NONE',  ( -0.04044903255042732459, 55.67930583240935505, -27.95245687107223986 ) ) ;
#16860 = CARTESIAN_POINT ( 'NONE',  ( 0.000000000000000000, 0.000000000000000000, 0.000000000000000000 ) ) ;
#16861 = CARTESIAN_POINT ( 'NONE',  ( 5.878266837044421923E-15, -70.99969134886156041, 0.000000000000000000 ) ) ;
#16862 = EDGE_LOOP ( 'NONE', ( #20121, #24868, #1751, #31959 ) ) ;
#16863 = CARTESIAN_POINT ( 'NONE',  ( 33.58253175000000113, 42.47500000273119980, -10.91162601494193751 ) ) ;
#16864 = CARTESIAN_POINT ( 'NONE',  ( -14.47279130897152299, 2.424999997268802332, 19.92008829642072243 ) ) ;
#16865 = CARTESIAN_POINT ( 'NONE',  ( -10.04305231718578462, 26.90000000546237402, 30.90933677959249337 ) ) ;
#16866 = EDGE_LOOP ( 'NONE', ( #12595, #11579, #26825, #24299, #11256, #13503 ) ) ;
#16867 = CARTESIAN_POINT ( 'NONE',  ( 30.02300923189239512, 37.35156249999997868, -2.619432448724977703E-13 ) ) ;
#16868 = ORIENTED_EDGE ( 'NONE', *, *, #23060, .F. ) ;
#16869 = CARTESIAN_POINT ( 'NONE',  ( -26.29305231718578995, 74.70000000546239960, 19.10302069950538595 ) ) ;
#16870 = CARTESIAN_POINT ( 'NONE',  ( 33.58253175000000823, 58.02500000273117564, 10.91162601494192863 ) ) ;
#16871 = CARTESIAN_POINT ( 'NONE',  ( 7.505752307973351023, 58.69270833333332860, 28.01184896238290278 ) ) ;
#16872 = CARTESIAN_POINT ( 'NONE',  ( 32.50000000000000000, 11.60000000546236798, -10.55989012756945833 ) ) ;
#16873 = FACE_OUTER_BOUND ( 'NONE', #28153, .T. ) ;
#16874 = CARTESIAN_POINT ( 'NONE',  ( 1.507698388325705758E-15, 13.62499999726882649, -24.62258325217400312 ) ) ;
#16875 = CARTESIAN_POINT ( 'NONE',  ( -10.04305231718578462, 62.40000000000001279, 30.90933677959249337 ) ) ;
#16876 = CARTESIAN_POINT ( 'NONE',  ( 27.16883889988623935, 20.57500000273118701, -19.73931689729374384 ) ) ;
#16877 =( LENGTH_UNIT ( ) NAMED_UNIT ( * ) SI_UNIT ( .MILLI., .METRE. ) );
#16878 = CARTESIAN_POINT ( 'NONE',  ( 14.01125832528330051, 15.86159749907602112, 24.18731323226221974 ) ) ;
#16879 = CARTESIAN_POINT ( 'NONE',  ( -4.300734207923755825, 75.27500000273118985, 13.23629886949340673 ) ) ;
#16880 = LINE ( 'NONE', #16101, #6905 ) ;
#16881 = CARTESIAN_POINT ( 'NONE',  ( 20.08610463437157279, 15.29999999999998472, -27.64615127144129758 ) ) ;
#16882 = CARTESIAN_POINT ( 'NONE',  ( 20.08610463437158344, 8.700000000000002842, 27.64615127144129403 ) ) ;
#16883 = EDGE_LOOP ( 'NONE', ( #16485, #3667, #32087, #24948 ) ) ;
#16884 = CARTESIAN_POINT ( 'NONE',  ( 23.41746825000000243, 5.224999997268802154, -7.608796670333727974 ) ) ;
#16885 = FACE_OUTER_BOUND ( 'NONE', #25341, .T. ) ;
#16886 = CARTESIAN_POINT ( 'NONE',  ( 19.09188309203694800, 37.78124999999999289, 19.09188309203660694 ) ) ;
#16887 = CARTESIAN_POINT ( 'NONE',  ( 27.16883889988624290, 15.92500000273117067, 19.73931689729373673 ) ) ;
#16888 = CARTESIAN_POINT ( 'NONE',  ( 10.37757302488624767, 67.72500000273116427, 31.93888565452638417 ) ) ;
#16889 = CARTESIAN_POINT ( 'NONE',  ( -20.75514604977248823, 29.07500000273119056, -28.56700777964554305 ) ) ;
#16890 = CARTESIAN_POINT ( 'NONE',  ( 20.75514604977249178, 14.07500000273119944, 28.56700777964553950 ) ) ;
#16891 = CARTESIAN_POINT ( 'NONE',  ( 20.75514604977249178, 10.07500000273117990, 28.56700777964553950 ) ) ;
#16892 = CARTESIAN_POINT ( 'NONE',  ( 14.97647472619947351, 11.86236083425730925, 26.02091320914850314 ) ) ;
#16893 = CARTESIAN_POINT ( 'NONE',  ( 15.01150461594643204, 55.11197916666664298, 26.00068869287340334 ) ) ;
#16894 = CARTESIAN_POINT ( 'NONE',  ( -2.375766604868044141, 81.55125428154683220, -14.99999999999999822 ) ) ;
#16895 =( BOUNDED_CURVE ( )  B_SPLINE_CURVE ( 2, ( #10781, #31703, #8030, #10610, #18346, #12667, #18516, #31198, #15424, #23317, #28790, #7522, #118 ),
 .UNSPECIFIED., .F., .T. ) 
 B_SPLINE_CURVE_WITH_KNOTS ( ( 3, 2, 2, 2, 2, 2, 3 ),
 ( 0.7115384615384615641, 0.7128205128205128416, 0.7153846153846153966, 0.7179487179487179516, 0.7205128205128205066, 0.7230769230769230616, 0.7243589743589743390 ),
 .UNSPECIFIED. ) 
 CURVE ( )  GEOMETRIC_REPRESENTATION_ITEM ( )  RATIONAL_B_SPLINE_CURVE ( ( 0.9755282581475768211, 0.9755282581475768211, 1.000000000000000000, 0.9510565162951535312, 1.000000000000000000, 0.9510565162951535312, 1.000000000000000000, 0.9510565162951535312, 1.000000000000000000, 0.9510565162951535312, 1.000000000000000000, 0.9755282581475768211, 0.9755282581475768211 ) ) 
 REPRESENTATION_ITEM ( '' )  );
#16896 = CARTESIAN_POINT ( 'NONE',  ( 13.91746824999999532, 74.47500000273117848, -4.522059556121118540 ) ) ;
#16897 = CARTESIAN_POINT ( 'NONE',  ( -26.29305231718579350, 45.79999999999999005, -19.10302069950537884 ) ) ;
#16898 = CARTESIAN_POINT ( 'NONE',  ( -15.14183272437242778, 3.049999994537633263, 20.84094480462497856 ) ) ;
#16899 = CARTESIAN_POINT ( 'NONE',  ( -33.58253175000000113, 51.12500000273117706, 0.000000000000000000 ) ) ;
#16900 = CARTESIAN_POINT ( 'NONE',  ( 14.47279130897151767, 4.924999997268811214, -19.92008829642072598 ) ) ;
#16901 = VERTEX_POINT ( 'NONE', #14734 ) ;
#16902 = CARTESIAN_POINT ( 'NONE',  ( -27.16883889988624290, 61.17500000273119554, -19.73931689729374028 ) ) ;
#16903 = CARTESIAN_POINT ( 'NONE',  ( -5.147494310547423346, 2.448745718453165132, 32.50000000000000000 ) ) ;
#16904 = CARTESIAN_POINT ( 'NONE',  ( 14.47279130897151589, 8.324999997268818674, 19.92008829642072953 ) ) ;
#16905 = CARTESIAN_POINT ( 'NONE',  ( 0.04044903254993986036, 34.49256916759064495, -27.95245687107223986 ) ) ;
#16906 = EDGE_LOOP ( 'NONE', ( #350, #3158, #15912, #556 ) ) ;
#16907 = CARTESIAN_POINT ( 'NONE',  ( -33.58253175000000113, 35.12500000273117706, 0.000000000000000000 ) ) ;
#16908 = CARTESIAN_POINT ( 'NONE',  ( -4.635254915624208216, 74.40000000000001990, 14.26584774442730463 ) ) ;
#16909 = ORIENTED_EDGE ( 'NONE', *, *, #29977, .F. ) ;
#16910 = CARTESIAN_POINT ( 'NONE',  ( -20.50609665440969209, 52.39062499999999289, 20.50609665441005092 ) ) ;
#16911 = CARTESIAN_POINT ( 'NONE',  ( -10.37757302488623701, 59.77500000273119696, 31.93888565452638417 ) ) ;
#16912 = CARTESIAN_POINT ( 'NONE',  ( 20.08610463437158344, 69.20000000546237118, 27.64615127144129403 ) ) ;
#16913 = CARTESIAN_POINT ( 'NONE',  ( 27.16883889988624290, 73.92500000273119554, 19.73931689729373673 ) ) ;
#16914 = CARTESIAN_POINT ( 'NONE',  ( 26.00068869287340334, 30.19010416666665719, -15.01150461594642316 ) ) ;
#16915 = EDGE_CURVE ( 'NONE', #19128, #6559, #17095, .T. ) ;
#16916 = CARTESIAN_POINT ( 'NONE',  ( -4.732186688966233175E-15, 3.500000000000005329, 25.76082449383753925 ) ) ;
#16917 = CARTESIAN_POINT ( 'NONE',  ( 27.16883889988623935, 4.575000002731199444, -19.73931689729374384 ) ) ;
#16918 = CARTESIAN_POINT ( 'NONE',  ( 33.58253175000000113, 16.22500000273118914, -10.91162601494193751 ) ) ;
#16919 = CARTESIAN_POINT ( 'NONE',  ( 8.601468415847516980, 74.17500000273119554, -11.83890561707634603 ) ) ;
#16920 = CARTESIAN_POINT ( 'NONE',  ( 7.543491769121922985, 40.06732666574268364, 28.00173670424535644 ) ) ;
#16921 = CARTESIAN_POINT ( 'NONE',  ( 11.25946833292375793, 72.57500000273120122, -8.180482586598735395 ) ) ;
#16922 = CARTESIAN_POINT ( 'NONE',  ( -7.505752307972844761, 55.54166666666667140, 28.01184896238304134 ) ) ;
#16923 = EDGE_CURVE ( 'NONE', #1690, #5766, #16010, .T. ) ;
#16924 = EDGE_CURVE ( 'NONE', #476, #14840, #14644, .T. ) ;
#16925 = CARTESIAN_POINT ( 'NONE',  ( 5.147494310547434893, 53.05125428700921475, 32.49999999999999289 ) ) ;
#16926 = CARTESIAN_POINT ( 'NONE',  ( 19.82091636218621034, 7.549999994537620829, 14.40073868116559730 ) ) ;
#16927 = CARTESIAN_POINT ( 'NONE',  ( -1.778240108872766143E-15, 71.50000000000001421, -32.49999999999999289 ) ) ;
#16928 = CARTESIAN_POINT ( 'NONE',  ( 0.04044903255044120238, 67.71055583240935505, 27.95245687107223276 ) ) ;
#16929 = CARTESIAN_POINT ( 'NONE',  ( -2.162160676586881955E-15, 38.62500000273118417, -35.31076352940723240 ) ) ;
#16930 = CARTESIAN_POINT ( 'NONE',  ( -8.601468415847515203, 77.17500000273118133, 11.83890561707634959 ) ) ;
#16931 = CARTESIAN_POINT ( 'NONE',  ( 33.58253175000000113, 48.47500000273118559, -10.91162601494193751 ) ) ;
#16932 = CARTESIAN_POINT ( 'NONE',  ( -10.37757302488623701, 29.77500000273120051, 31.93888565452638417 ) ) ;
#16933 = CARTESIAN_POINT ( 'NONE',  ( -13.41233651847560182, 16.99999999999998934, 20.39142027516456679 ) ) ;
#16934 = CARTESIAN_POINT ( 'NONE',  ( -13.97622843553632777, 32.76822916666666430, -24.20753774853731599 ) ) ;
#16935 = CARTESIAN_POINT ( 'NONE',  ( 19.82091636218621034, 1.799999999999996048, 14.40073868116559730 ) ) ;
#16936 =( BOUNDED_CURVE ( )  B_SPLINE_CURVE ( 2, ( #16807, #14059, #11151, #24029, #16468, #8226, #24684, #27263, #29156, #18879, #19214, #29328, #32065 ),
 .UNSPECIFIED., .F., .F. ) 
 B_SPLINE_CURVE_WITH_KNOTS ( ( 3, 2, 2, 2, 2, 2, 3 ),
 ( 0.4722222222222222654, 0.4777777777777778012, 0.4888888888888888729, 0.5000000000000000000, 0.5111111111111110716, 0.5222222222222222543, 0.5277777777777777901 ),
 .UNSPECIFIED. ) 
 CURVE ( )  GEOMETRIC_REPRESENTATION_ITEM ( )  RATIONAL_B_SPLINE_CURVE ( ( 0.9755282581475767101, 0.9755282581475768211, 1.000000000000000000, 0.9510565162951535312, 1.000000000000000000, 0.9510565162951535312, 1.000000000000000000, 0.9510565162951535312, 1.000000000000000000, 0.9510565162951535312, 1.000000000000000000, 0.9755282581475768211, 0.9755282581475768211 ) ) 
 REPRESENTATION_ITEM ( '' )  );
#16937 = CARTESIAN_POINT ( 'NONE',  ( 26.29305231718579350, 78.79999999999998295, 19.10302069950537529 ) ) ;
#16938 = CARTESIAN_POINT ( 'NONE',  ( 6.277390505771533514E-15, 68.50000000000002842, 34.17252228774368916 ) ) ;
#16939 = CARTESIAN_POINT ( 'NONE',  ( 14.47279130897151767, 8.324999997268818674, 19.92008829642072953 ) ) ;
#16940 = CARTESIAN_POINT ( 'NONE',  ( 7.468012846824281681, 24.88503499907601935, -28.02196122052058058 ) ) ;
#16941 = CARTESIAN_POINT ( 'NONE',  ( -20.08610463437156923, 52.80000000546237260, 27.64615127144130113 ) ) ;
#16942 = CARTESIAN_POINT ( 'NONE',  ( 24.18731323226221974, 35.62722249907602645, -14.01125832528328985 ) ) ;
#16943 = CARTESIAN_POINT ( 'NONE',  ( -3.880418787951136483, 12.55125428154685174, -24.50000000000000000 ) ) ;
#16944 = CARTESIAN_POINT ( 'NONE',  ( -27.16883889988623935, 11.32500000273117813, 19.73931689729374739 ) ) ;
#16945 = CARTESIAN_POINT ( 'NONE',  ( -14.47279130897152122, 4.424999997268826313, 19.92008829642072243 ) ) ;
#16946 = CARTESIAN_POINT ( 'NONE',  ( -2.428612866367529427E-13, 57.11718750000000711, -27.95245687107222921 ) ) ;
#16947 = ORIENTED_EDGE ( 'NONE', *, *, #13790, .T. ) ;
#16948 = CARTESIAN_POINT ( 'NONE',  ( -33.58253175000000113, 53.22500000273118559, 10.91162601494193929 ) ) ;
#16949 = CARTESIAN_POINT ( 'NONE',  ( 20.75514604977248467, 30.67500000273119909, -28.56700777964554305 ) ) ;
#16950 = VERTEX_POINT ( 'NONE', #7857 ) ;
#16951 = CARTESIAN_POINT ( 'NONE',  ( 20.50609665440969565, 26.60937499999999645, -20.50609665441004736 ) ) ;
#16952 = CARTESIAN_POINT ( 'NONE',  ( -7.468012846824771955, 20.59934000092397355, -28.02196122052045624 ) ) ;
#16953 = CARTESIAN_POINT ( 'NONE',  ( 7.570916362186213000, 16.14999999453761603, -23.30088464923126423 ) ) ;
#16954 = CARTESIAN_POINT ( 'NONE',  ( -15.14183272437242600, 19.04999999453762172, 20.84094480462497856 ) ) ;
#16955 = CARTESIAN_POINT ( 'NONE',  ( -14.47279130897151589, 3.324999997268803131, -19.92008829642072598 ) ) ;
#16956 = CARTESIAN_POINT ( 'NONE',  ( 33.58253175000000113, 22.47500000273119625, -10.91162601494193751 ) ) ;
#16957 = CARTESIAN_POINT ( 'NONE',  ( -10.04305231718579172, 30.10000000546236976, -30.90933677959248982 ) ) ;
#16958 = CARTESIAN_POINT ( 'NONE',  ( -32.50000000000000000, 73.90000000000003411, -10.55989012756945478 ) ) ;
#16959 = CARTESIAN_POINT ( 'NONE',  ( 32.50000000000000711, 47.40000000546237402, 10.55989012756945122 ) ) ;
#16960 = CARTESIAN_POINT ( 'NONE',  ( 12.13525491562420910, 73.19999999999998863, -8.816778784387098611 ) ) ;
#16961 = CARTESIAN_POINT ( 'NONE',  ( 30.02300923189239867, 59.41444416759064495, 0.04044903254992252006 ) ) ;
#16962 = CARTESIAN_POINT ( 'NONE',  ( 33.58253175000000823, 38.27500000273118985, 10.91162601494192863 ) ) ;
#16963 = CARTESIAN_POINT ( 'NONE',  ( 20.75514604977248467, 52.42500000273118133, -28.56700777964554305 ) ) ;
#16964 = CARTESIAN_POINT ( 'NONE',  ( 30.02300923189239867, 33.91406249999998579, -2.619432448724978208E-13 ) ) ;
#16965 = CARTESIAN_POINT ( 'NONE',  ( 7.236395654485755280, 10.72499999726880837, 22.27133577429736988 ) ) ;
#16966 = CARTESIAN_POINT ( 'NONE',  ( 32.50000000000000000, 17.00000000000001421, -3.980102097228898626E-15 ) ) ;
#16967 = CARTESIAN_POINT ( 'NONE',  ( -4.732186688966233175E-15, 11.49999999999998579, 25.76082449383753925 ) ) ;
#16968 = CARTESIAN_POINT ( 'NONE',  ( -26.06988505166722803, 47.80170166574269786, 7.025853678916877953 ) ) ;
#16969 = CARTESIAN_POINT ( 'NONE',  ( 10.37757302488624767, 53.72500000273117138, 31.93888565452638417 ) ) ;
#16970 = CARTESIAN_POINT ( 'NONE',  ( 20.75514604977248467, 44.67500000273118843, -28.56700777964554305 ) ) ;
#16971 = CARTESIAN_POINT ( 'NONE',  ( 23.41746824999999887, 12.62499999726882116, 0.000000000000000000 ) ) ;
#16972 = CARTESIAN_POINT ( 'NONE',  ( 26.29305231718578995, 67.70000000546238539, -19.10302069950538240 ) ) ;
#16973 = CARTESIAN_POINT ( 'NONE',  ( 10.37757302488624056, 8.525000002731180970, -31.93888565452638417 ) ) ;
#16974 = CARTESIAN_POINT ( 'NONE',  ( 0.04044903254993986036, 37.93006916759064495, -27.95245687107223986 ) ) ;
#16975 = EDGE_CURVE ( 'NONE', #19688, #33879, #16895, .T. ) ;
#16976 = CARTESIAN_POINT ( 'NONE',  ( 15.46695104312588498, 16.99999999999998224, -17.59928039462594640 ) ) ;
#16977 = CARTESIAN_POINT ( 'NONE',  ( 0.000000000000000000, 74.00000000000001421, 0.000000000000000000 ) ) ;
#16978 = CARTESIAN_POINT ( 'NONE',  ( -33.58253175000000113, 25.12500000273119838, 0.000000000000000000 ) ) ;
#16979 = CARTESIAN_POINT ( 'NONE',  ( 32.50000000000000000, 67.10000000000000853, -10.55989012756945833 ) ) ;
#16980 = FACE_OUTER_BOUND ( 'NONE', #32753, .T. ) ;
#16981 = CARTESIAN_POINT ( 'NONE',  ( 20.08610463437157279, 61.30000000000001137, -27.64615127144129758 ) ) ;
#16982 = CARTESIAN_POINT ( 'NONE',  ( 28.00173670424535644, 52.95795166574269075, -7.543491769121920321 ) ) ;
#16983 = CARTESIAN_POINT ( 'NONE',  ( -26.29305231718579350, 46.30000000546237260, -19.10302069950537884 ) ) ;
#16984 = FILL_AREA_STYLE ('',( #32414 ) ) ;
#16985 = CARTESIAN_POINT ( 'NONE',  ( -27.16883889988623935, 31.32500000273119412, 19.73931689729374739 ) ) ;
#16986 = CARTESIAN_POINT ( 'NONE',  ( -6.988114217768288228, 29.47395833333332860, -26.07999730980477437 ) ) ;
#16987 = CARTESIAN_POINT ( 'NONE',  ( -20.75514604977248112, 77.42500000273119554, 28.56700777964554661 ) ) ;
#16988 = CARTESIAN_POINT ( 'NONE',  ( 28.01184896238290278, 26.89583333333332860, -7.505752307973347470 ) ) ;
#16989 = CARTESIAN_POINT ( 'NONE',  ( 3.980102097228898626E-15, 52.00000000000000711, -32.50000000000000000 ) ) ;
#16990 = ORIENTED_EDGE ( 'NONE', *, *, #16405, .T. ) ;
#16991 = CARTESIAN_POINT ( 'NONE',  ( -28.02196122052045268, 54.11496500092397355, 7.468012846824790607 ) ) ;
#16992 = CARTESIAN_POINT ( 'NONE',  ( -10.04305231718578462, 10.90000000546235981, 30.90933677959249337 ) ) ;
#16993 =( BOUNDED_CURVE ( )  B_SPLINE_CURVE ( 2, ( #19438, #21847, #27659, #19269, #4148, #6215, #19939, #29886, #12034, #30218, #25077, #32791, #19604, #16864, #14621, #17030, #32955, #27489, #3979, #11529, #1558, #24741, #11869, #11697, #22344, #9284, #16696, #27152, #19768, #24577, #6719, #1049, #14789, #890, #27325, #3813, #14285, #31082, #7578, #18057, #4828, #25603, #4487, #28502, #18231, #33485, #1728, #15139, #33659, #22853, #15308, #4999, #9986, #10330, #25767, #15482, #25936, #25253, #14963, #28677, #28000, #17713, #20806, #2253, #25429, #12208, #30910, #20459, #5174, #2082, #12897, #20117, #12557, #12727, #12384, #22679, #10157, #1907, #7404, #2429, #23028, #20639, #33130, #23197, #20287, #17890, #9634, #28343, #23372, #33833, #31250, #7742, #30561, #7058, #9810, #33311, #17540, #30734, #7227, #28171, #4659, #2939, #26107, #23878, #3, #5343, #32086, #10832, #28844, #23542, #2769, #21311, #13233, #2605, #8411, #10493, #18900, #20970, #683, #11169, #31752, #31421, #8243, #23707, #18736, #31919, #13066, #16161, #15824, #7914, #21640, #29346, #29178, #5683, #10663, #173, #26615, #13410, #24046, #5847, #18398, #8582, #3112, #26278, #21142, #31583, #13584, #8083, #18570, #16326, #29011, #26782, #5511, #19066, #29506, #515, #11002, #15657, #15992, #3273, #13741 ),
 .UNSPECIFIED., .F., .F. ) 
 B_SPLINE_CURVE_WITH_KNOTS ( ( 3, 2, 2, 2, 2, 2, 2, 2, 2, 2, 2, 2, 2, 2, 2, 2, 2, 2, 2, 2, 2, 2, 2, 2, 2, 2, 2, 2, 2, 2, 2, 2, 2, 2, 2, 2, 2, 2, 2, 2, 2, 2, 2, 2, 2, 2, 2, 2, 2, 2, 2, 2, 2, 2, 2, 2, 2, 2, 2, 2, 2, 2, 2, 2, 2, 2, 2, 2, 2, 2, 2, 2, 2, 2, 2, 2, 2, 2, 2, 2, 3 ),
 ( 0.000000000000000000, 0.01111111111111111154, 0.02222222222222222307, 0.03333333333333333287, 0.04444444444444444614, 0.05555555555555555247, 0.06666666666666666574, 0.07777777777777779289, 0.08888888888888889228, 0.1000000000000000056, 0.1111111111111111049, 0.1222222222222222182, 0.1333333333333333315, 0.1444444444444444309, 0.1555555555555555858, 0.1666666666666666574, 0.1777777777777777846, 0.1888888888888888840, 0.2000000000000000111, 0.2111111111111111105, 0.2222222222222222099, 0.2333333333333333370, 0.2444444444444444364, 0.2555555555555555358, 0.2666666666666666630, 0.2777777777777777901, 0.2888888888888888618, 0.2999999999999999889, 0.3111111111111111716, 0.3222222222222222432, 0.3333333333333333148, 0.3444444444444444420, 0.3555555555555555691, 0.3666666666666666408, 0.3777777777777777679, 0.3888888888888888951, 0.4000000000000000222, 0.4111111111111110938, 0.4222222222222222210, 0.4333333333333333481, 0.4444444444444444198, 0.4555555555555555469, 0.4666666666666666741, 0.4777777777777777457, 0.4888888888888888729, 0.5000000000000000000, 0.5111111111111110716, 0.5222222222222222543, 0.5333333333333333259, 0.5444444444444443976, 0.5555555555555555802, 0.5666666666666666519, 0.5777777777777777235, 0.5888888888888889062, 0.5999999999999999778, 0.6111111111111111605, 0.6222222222222223431, 0.6333333333333333037, 0.6444444444444444864, 0.6555555555555555580, 0.6666666666666666297, 0.6777777777777778123, 0.6888888888888888840, 0.6999999999999999556, 0.7111111111111111382, 0.7222222222222222099, 0.7333333333333332815, 0.7444444444444445752, 0.7555555555555555358, 0.7666666666666667185, 0.7777777777777777901, 0.7888888888888888618, 0.8000000000000000444, 0.8111111111111111160, 0.8222222222222221877, 0.8333333333333332593, 0.8444444444444444420, 0.8555555555555555136, 0.8666666666666666963, 0.8777777777777777679, 0.8819764054827600175 ),
 .UNSPECIFIED. ) 
 CURVE ( )  GEOMETRIC_REPRESENTATION_ITEM ( )  RATIONAL_B_SPLINE_CURVE ( ( 1.000000000000000000, 0.9510565162951535312, 1.000000000000000000, 0.9510565162951535312, 1.000000000000000000, 0.9510565162951535312, 1.000000000000000000, 0.9510565162951535312, 1.000000000000000000, 0.9510565162951535312, 1.000000000000000000, 0.9510565162951535312, 1.000000000000000000, 0.9510565162951535312, 1.000000000000000000, 0.9510565162951535312, 1.000000000000000000, 0.9510565162951535312, 1.000000000000000000, 0.9510565162951535312, 1.000000000000000000, 0.9510565162951535312, 1.000000000000000000, 0.9510565162951535312, 1.000000000000000000, 0.9510565162951535312, 1.000000000000000000, 0.9510565162951535312, 1.000000000000000000, 0.9510565162951535312, 1.000000000000000000, 0.9510565162951535312, 1.000000000000000000, 0.9510565162951535312, 1.000000000000000000, 0.9510565162951535312, 1.000000000000000000, 0.9510565162951535312, 1.000000000000000000, 0.9510565162951535312, 1.000000000000000000, 0.9510565162951535312, 1.000000000000000000, 0.9510565162951535312, 1.000000000000000000, 0.9510565162951535312, 1.000000000000000000, 0.9510565162951535312, 1.000000000000000000, 0.9510565162951535312, 1.000000000000000000, 0.9510565162951535312, 1.000000000000000000, 0.9510565162951535312, 1.000000000000000000, 0.9510565162951535312, 1.000000000000000000, 0.9510565162951535312, 1.000000000000000000, 0.9510565162951535312, 1.000000000000000000, 0.9510565162951535312, 1.000000000000000000, 0.9510565162951535312, 1.000000000000000000, 0.9510565162951535312, 1.000000000000000000, 0.9510565162951535312, 1.000000000000000000, 0.9510565162951535312, 1.000000000000000000, 0.9510565162951535312, 1.000000000000000000, 0.9510565162951535312, 1.000000000000000000, 0.9510565162951535312, 1.000000000000000000, 0.9510565162951535312, 1.000000000000000000, 0.9510565162951535312, 1.000000000000000000, 0.9510565162951535312, 1.000000000000000000, 0.9510565162951535312, 1.000000000000000000, 0.9510565162951535312, 1.000000000000000000, 0.9510565162951535312, 1.000000000000000000, 0.9510565162951535312, 1.000000000000000000, 0.9510565162951535312, 1.000000000000000000, 0.9510565162951535312, 1.000000000000000000, 0.9510565162951535312, 1.000000000000000000, 0.9510565162951535312, 1.000000000000000000, 0.9510565162951535312, 1.000000000000000000, 0.9510565162951535312, 1.000000000000000000, 0.9510565162951535312, 1.000000000000000000, 0.9510565162951535312, 1.000000000000000000, 0.9510565162951535312, 1.000000000000000000, 0.9510565162951535312, 1.000000000000000000, 0.9510565162951535312, 1.000000000000000000, 0.9510565162951535312, 1.000000000000000000, 0.9510565162951535312, 1.000000000000000000, 0.9510565162951535312, 1.000000000000000000, 0.9510565162951535312, 1.000000000000000000, 0.9510565162951535312, 1.000000000000000000, 0.9510565162951535312, 1.000000000000000000, 0.9510565162951535312, 1.000000000000000000, 0.9510565162951535312, 1.000000000000000000, 0.9510565162951535312, 1.000000000000000000, 0.9510565162951535312, 1.000000000000000000, 0.9510565162951535312, 1.000000000000000000, 0.9510565162951535312, 1.000000000000000000, 0.9510565162951535312, 1.000000000000000000, 0.9510565162951535312, 1.000000000000000000, 0.9510565162951535312, 1.000000000000000000, 0.9510565162951535312, 1.000000000000000000, 0.9510565162951535312, 1.000000000000000000, 0.9510565162951535312, 1.000000000000000000, 0.9510565162951535312, 1.000000000000000000, 0.9510565162951535312, 1.000000000000000000, 0.9510565162951535312, 1.000000000000000000, 0.9510565162951535312, 1.000000000000000000, 0.9510565162951535312, 1.000000000000000000, 0.9815054080004634862, 0.9769881591460145565 ) ) 
 REPRESENTATION_ITEM ( '' )  );
#16994 = CARTESIAN_POINT ( 'NONE',  ( 28.01184896238290278, 64.70833333333334281, -7.505752307973347470 ) ) ;
#16995 = CARTESIAN_POINT ( 'NONE',  ( 10.04305231718579705, 20.60000000000000853, 30.90933677959248982 ) ) ;
#16996 = CARTESIAN_POINT ( 'NONE',  ( 33.58253175000000113, 42.37500000273119838, -4.112674001490185761E-15 ) ) ;
#16997 = CARTESIAN_POINT ( 'NONE',  ( -26.29305231718578995, 52.70000000546237828, 19.10302069950538595 ) ) ;
#16998 =( BOUNDED_CURVE ( )  B_SPLINE_CURVE ( 2, ( #21826, #1198, #29866, #24722, #29688, #14100, #27131, #32273, #5868, #24070, #8766, #16346, #11510 ),
 .UNSPECIFIED., .F., .T. ) 
 B_SPLINE_CURVE_WITH_KNOTS ( ( 3, 2, 2, 2, 2, 2, 3 ),
 ( 0.9166666666666666297, 0.9222222222222222765, 0.9333333333333333481, 0.9444444444444444198, 0.9555555555555556024, 0.9666666666666666741, 0.9722222222222222099 ),
 .UNSPECIFIED. ) 
 CURVE ( )  GEOMETRIC_REPRESENTATION_ITEM ( )  RATIONAL_B_SPLINE_CURVE ( ( 0.9755282581475768211, 0.9755282581475765991, 1.000000000000000000, 0.9510565162951535312, 1.000000000000000000, 0.9510565162951535312, 1.000000000000000000, 0.9510565162951535312, 1.000000000000000000, 0.9510565162951535312, 1.000000000000000000, 0.9755282581475768211, 0.9755282581475768211 ) ) 
 REPRESENTATION_ITEM ( '' )  );
#16999 = CARTESIAN_POINT ( 'NONE',  ( 13.91746824999999887, 74.37500000273116996, -1.704398294459741270E-15 ) ) ;
#17000 = CARTESIAN_POINT ( 'NONE',  ( 27.16883889988623935, 32.32500000273119412, -19.73931689729374384 ) ) ;
#17001 = CARTESIAN_POINT ( 'NONE',  ( -32.50000000000000000, 62.40000000546236691, -10.55989012756945300 ) ) ;
#17002 = CARTESIAN_POINT ( 'NONE',  ( 33.58253175000000113, 54.37500000273118417, -4.112674001490185761E-15 ) ) ;
#17003 = FILL_AREA_STYLE ('',( #21652 ) ) ;
#17004 = CARTESIAN_POINT ( 'NONE',  ( 10.04305231718579705, 36.60000000000000853, 30.90933677959248982 ) ) ;
#17005 = CARTESIAN_POINT ( 'NONE',  ( -2.092463501923844636E-15, 31.49999999999999289, -34.17252228774368916 ) ) ;
#17006 = CARTESIAN_POINT ( 'NONE',  ( -23.41746825000000243, 11.52499999726880553, -7.608796670333730638 ) ) ;
#17007 = CARTESIAN_POINT ( 'NONE',  ( -10.37757302488623701, 73.52500000273121827, 31.93888565452638417 ) ) ;
#17008 = CARTESIAN_POINT ( 'NONE',  ( 0.000000000000000000, 80.00000000000001421, 0.000000000000000000 ) ) ;
#17009 = CARTESIAN_POINT ( 'NONE',  ( -13.91746824999999532, 77.47500000273117848, 4.522059556121122093 ) ) ;
#17010 = CARTESIAN_POINT ( 'NONE',  ( -20.75514604977248112, 65.67500000273116711, 28.56700777964554661 ) ) ;
#17011 = CARTESIAN_POINT ( 'NONE',  ( 2.067204126564591252E-14, 4.249999994537631665, -24.50000000000000000 ) ) ;
#17012 = CARTESIAN_POINT ( 'NONE',  ( -19.82091636218621034, 2.549999994537616388, -14.40073868116559552 ) ) ;
#17013 = CARTESIAN_POINT ( 'NONE',  ( -19.06425588902591173, 13.43788166759064140, -19.11951029504763611 ) ) ;
#17014 = EDGE_CURVE ( 'NONE', #14163, #29502, #2568, .T. ) ;
#17015 = CARTESIAN_POINT ( 'NONE',  ( 5.779280353836490358E-15, 11.00000000546238077, 32.49999999999999289 ) ) ;
#17016 = CARTESIAN_POINT ( 'NONE',  ( -2.162160676586881955E-15, 48.62500000273118417, -35.31076352940723240 ) ) ;
#17017 = CARTESIAN_POINT ( 'NONE',  ( 6.486482029760649416E-15, 1.875000002731192383, 35.31076352940723240 ) ) ;
#17018 = CARTESIAN_POINT ( 'NONE',  ( 10.37757302488624056, 60.77500000273118275, -31.93888565452638417 ) ) ;
#17019 = CARTESIAN_POINT ( 'NONE',  ( 24.20753774853756113, 47.95052083333332149, 13.97622843553589789 ) ) ;
#17020 = CARTESIAN_POINT ( 'NONE',  ( 25.98046417659858420, 42.51340250092398065, 15.04653450569292872 ) ) ;
#17021 = ADVANCED_FACE ( 'NONE', ( #7689 ), #2013, .T. ) ;
#17022 = CARTESIAN_POINT ( 'NONE',  ( -28.00173670424535644, 30.61420166574267654, 7.543491769121936308 ) ) ;
#17023 = CARTESIAN_POINT ( 'NONE',  ( 6.277390505771533514E-15, 69.00000000546239676, 34.17252228774368916 ) ) ;
#17024 = CARTESIAN_POINT ( 'NONE',  ( -8.960552108402742093E-16, 76.37500000273114154, -14.63369212191046387 ) ) ;
#17025 = CARTESIAN_POINT ( 'NONE',  ( -19.06425588902558133, 57.82774333240935505, 19.11951029504797006 ) ) ;
#17026 = CARTESIAN_POINT ( 'NONE',  ( -20.08610463437157989, 57.70000000000000995, -27.64615127144129758 ) ) ;
#17027 = CARTESIAN_POINT ( 'NONE',  ( -15.14183272437242067, 4.449999994537617631, -20.84094480462497856 ) ) ;
#17028 = ORIENTED_EDGE ( 'NONE', *, *, #1791, .F. ) ;
#17029 = CARTESIAN_POINT ( 'NONE',  ( -33.58253175000000113, 41.27500000273117564, -10.91162601494193218 ) ) ;
#17030 = CARTESIAN_POINT ( 'NONE',  ( -4.523095164977117273E-15, 2.624999997268825602, 24.62258325217400312 ) ) ;
#17031 = CARTESIAN_POINT ( 'NONE',  ( -26.29305231718579350, 32.30000000546238681, -19.10302069950537884 ) ) ;
#17032 = VERTEX_POINT ( 'NONE', #20915 ) ;
#17033 = CARTESIAN_POINT ( 'NONE',  ( 2.740863092043355209E-13, 31.33593749999999289, 30.02300923189239512 ) ) ;
#17034 = EDGE_LOOP ( 'NONE', ( #31836, #8630, #25037, #7140 ) ) ;
#17035 = ORIENTED_EDGE ( 'NONE', *, *, #11313, .T. ) ;
#17036 = CARTESIAN_POINT ( 'NONE',  ( -1.778240108872766143E-15, 55.49999999999999289, -32.49999999999999289 ) ) ;
#17037 = CARTESIAN_POINT ( 'NONE',  ( 33.58253175000000113, 50.12500000273117706, -4.112674001490185761E-15 ) ) ;
#17038 = CARTESIAN_POINT ( 'NONE',  ( -15.01150461594642138, 53.39322916666665009, -26.00068869287340334 ) ) ;
#17039 = CARTESIAN_POINT ( 'NONE',  ( 32.50000000000000000, 11.50000000546236301, -3.980102097228898626E-15 ) ) ;
#17040 = CARTESIAN_POINT ( 'NONE',  ( -10.04305231718578462, 8.400000000000018119, 30.90933677959249337 ) ) ;
#17041 = CARTESIAN_POINT ( 'NONE',  ( -7.236395654485763274, 14.52499999726880553, 22.27133577429736633 ) ) ;
#17042 = CARTESIAN_POINT ( 'NONE',  ( 20.08610463437158344, 52.69999999999998863, 27.64615127144129403 ) ) ;
#17043 = CARTESIAN_POINT ( 'NONE',  ( 27.16883889988624290, 26.17500000273118133, 19.73931689729373673 ) ) ;
#17044 = LINE ( 'NONE', #27340, #4707 ) ;
#17045 = CARTESIAN_POINT ( 'NONE',  ( 30.02300923189239867, 66.85118083240935505, -0.04044903255044467877 ) ) ;
#17046 = CARTESIAN_POINT ( 'NONE',  ( -11.25946833292375793, 75.07500000273120122, 8.180482586598737171 ) ) ;
#17047 = CARTESIAN_POINT ( 'NONE',  ( 0.000000000000000000, 80.00000000000001421, -32.50000000000000000 ) ) ;
#17048 = CARTESIAN_POINT ( 'NONE',  ( 30.16025403784430736, -21.99999999999999289, 3.693565856891707127E-15 ) ) ;
#17049 = CARTESIAN_POINT ( 'NONE',  ( 32.50000000000000000, 3.099999999999989875, -10.55989012756945833 ) ) ;
#17050 = VERTEX_POINT ( 'NONE', #31365 ) ;
#17051 = CARTESIAN_POINT ( 'NONE',  ( -23.41746824999999887, 8.124999997268817609, -2.867812753649727150E-15 ) ) ;
#17052 = DIRECTION ( 'NONE',  ( 0.000000000000000000, 0.000000000000000000, -1.000000000000000000 ) ) ;
#17053 = AXIS2_PLACEMENT_3D ( 'NONE', #31370, #18010, #4948 ) ;
#17054 = CARTESIAN_POINT ( 'NONE',  ( 24.20753774853731244, 43.94010416666665719, -13.97622843553632599 ) ) ;
#17055 = CARTESIAN_POINT ( 'NONE',  ( 10.37757302488624056, 66.52500000273118985, -31.93888565452638417 ) ) ;
#17056 = CARTESIAN_POINT ( 'NONE',  ( -2.162160676586881955E-15, 20.87500000273119127, -35.31076352940723240 ) ) ;
#17057 = CARTESIAN_POINT ( 'NONE',  ( -10.37757302488624411, 18.97500000273118204, -31.93888565452638417 ) ) ;
#17058 = CARTESIAN_POINT ( 'NONE',  ( 20.75514604977249178, 8.075000002731185234, 28.56700777964553950 ) ) ;
#17059 = CARTESIAN_POINT ( 'NONE',  ( 28.02196122052045268, 11.14621500092397532, -7.468012846824774620 ) ) ;
#17060 = ADVANCED_FACE ( 'NONE', ( #26055 ), #2716, .T. ) ;
#17061 = CARTESIAN_POINT ( 'NONE',  ( -20.50609665441004736, 56.68749999999998579, -20.50609665440969565 ) ) ;
#17062 = CARTESIAN_POINT ( 'NONE',  ( -4.300734207923755825, 77.77500000273118985, 13.23629886949340673 ) ) ;
#17063 = CARTESIAN_POINT ( 'NONE',  ( 32.50000000000000000, 47.00000000000000000, -3.980102097228898626E-15 ) ) ;
#17064 = AXIS2_PLACEMENT_3D ( 'NONE', #31684, #15922, #2702 ) ;
#17065 = AXIS2_PLACEMENT_3D ( 'NONE', #5430, #13326, #23799 ) ;
#17066 = CARTESIAN_POINT ( 'NONE',  ( -10.37757302488623701, 49.52500000273118985, 31.93888565452638417 ) ) ;
#17067 = CARTESIAN_POINT ( 'NONE',  ( 14.47279130897151589, 18.82499999726881157, 19.92008829642072953 ) ) ;
#17068 = ORIENTED_EDGE ( 'NONE', *, *, #25075, .F. ) ;
#17069 = CARTESIAN_POINT ( 'NONE',  ( -33.58253175000000113, 63.37500000273120548, 0.000000000000000000 ) ) ;
#17070 = CARTESIAN_POINT ( 'NONE',  ( 10.04305231718578817, 43.39999999999999147, -30.90933677959249337 ) ) ;
#17071 = CARTESIAN_POINT ( 'NONE',  ( -4.523095164977116484E-15, 14.12499999726881050, 24.62258325217400312 ) ) ;
#17072 = CARTESIAN_POINT ( 'NONE',  ( 6.950374756619721595, 29.19309000092397000, 26.09010956794232428 ) ) ;
#17073 = ORIENTED_EDGE ( 'NONE', *, *, #4845, .T. ) ;
#17074 = CARTESIAN_POINT ( 'NONE',  ( -20.75514604977248823, 32.82500000273118701, -28.56700777964554305 ) ) ;
#17075 = DIRECTION ( 'NONE',  ( 0.000000000000000000, 1.000000000000000000, 0.000000000000000000 ) ) ;
#17076 = EDGE_CURVE ( 'NONE', #31503, #10494, #27816, .T. ) ;
#17077 = ORIENTED_EDGE ( 'NONE', *, *, #27400, .T. ) ;
#17078 = CARTESIAN_POINT ( 'NONE',  ( 28.01184896238290278, 61.27083333333332860, -7.505752307973347470 ) ) ;
#17079 = CARTESIAN_POINT ( 'NONE',  ( 10.37757302488624056, 58.77500000273119696, -31.93888565452638417 ) ) ;
#17080 = CARTESIAN_POINT ( 'NONE',  ( -8.891200544363830713E-16, 75.50000000000001421, -15.00000000000000000 ) ) ;
#17081 = CARTESIAN_POINT ( 'NONE',  ( -20.75514604977248823, 64.82500000273120122, -28.56700777964554305 ) ) ;
#17082 = CARTESIAN_POINT ( 'NONE',  ( 2.740863092043355209E-13, 27.89843750000000000, 30.02300923189239512 ) ) ;
#17083 = CARTESIAN_POINT ( 'NONE',  ( -7.570916362186210335, 8.599999999999996092, -23.30088464923126779 ) ) ;
#17084 = CARTESIAN_POINT ( 'NONE',  ( 27.16883889988623935, 2.575000002731198112, -19.73931689729374384 ) ) ;
#17085 = CARTESIAN_POINT ( 'NONE',  ( 33.58253175000000823, 14.02500000273117209, 10.91162601494192863 ) ) ;
#17086 = CARTESIAN_POINT ( 'NONE',  ( -4.300734207923759378, 72.47500000273119269, -13.23629886949340495 ) ) ;
#17087 = CARTESIAN_POINT ( 'NONE',  ( -7.543491769121917656, 45.22357666574267654, -28.00173670424536354 ) ) ;
#17088 = STYLED_ITEM ( 'NONE', ( #13122 ), #9552 ) ;
#17089 = CARTESIAN_POINT ( 'NONE',  ( -11.25946833292375793, 71.57500000273120122, 8.180482586598737171 ) ) ;
#17090 = CARTESIAN_POINT ( 'NONE',  ( -20.50609665441004736, 60.12500000000000000, -20.50609665440969565 ) ) ;
#17091 = CARTESIAN_POINT ( 'NONE',  ( -12.13525491562421088, 74.05000000546237970, -8.816778784387096835 ) ) ;
#17092 = CARTESIAN_POINT ( 'NONE',  ( 19.82091636218621389, 7.949999994537631842, -14.40073868116559197 ) ) ;
#17093 = CARTESIAN_POINT ( 'NONE',  ( -12.13525491562421088, 78.05000000546239391, -8.816778784387096835 ) ) ;
#17094 = CARTESIAN_POINT ( 'NONE',  ( 26.07999730980477437, 13.14583333333332860, -6.988114217768290004 ) ) ;
#17095 =( BOUNDED_CURVE ( )  B_SPLINE_CURVE ( 2, ( #4091, #7172, #15078, #22622, #17653, #24853, #28114, #2026, #17312, #12327, #1334, #33074, #1673 ),
 .UNSPECIFIED., .F., .T. ) 
 B_SPLINE_CURVE_WITH_KNOTS ( ( 3, 2, 2, 2, 2, 2, 3 ),
 ( 0.1388888888888888951, 0.1444444444444444309, 0.1555555555555555580, 0.1666666666666666574, 0.1777777777777777846, 0.1888888888888888840, 0.1944444444444444475 ),
 .UNSPECIFIED. ) 
 CURVE ( )  GEOMETRIC_REPRESENTATION_ITEM ( )  RATIONAL_B_SPLINE_CURVE ( ( 0.9755282581475768211, 0.9755282581475768211, 1.000000000000000000, 0.9510565162951535312, 1.000000000000000000, 0.9510565162951535312, 1.000000000000000000, 0.9510565162951535312, 1.000000000000000000, 0.9510565162951535312, 1.000000000000000000, 0.9755282581475768211, 0.9755282581475768211 ) ) 
 REPRESENTATION_ITEM ( '' )  );
#17096 = CARTESIAN_POINT ( 'NONE',  ( 10.37757302488624056, 40.52500000273118275, -31.93888565452638417 ) ) ;
#17097 = CARTESIAN_POINT ( 'NONE',  ( -11.25946833292375793, 76.67500000273119554, -8.180482586598733619 ) ) ;
#17098 = CARTESIAN_POINT ( 'NONE',  ( -20.75514604977248823, 49.07500000273117280, -28.56700777964554305 ) ) ;
#17099 = CARTESIAN_POINT ( 'NONE',  ( -33.58253175000000113, 29.27500000273118630, -10.91162601494193041 ) ) ;
#17100 = CARTESIAN_POINT ( 'NONE',  ( 10.04305231718578817, 41.39999999999999147, -30.90933677959249337 ) ) ;
#17101 = CARTESIAN_POINT ( 'NONE',  ( 19.09188309203694800, 30.90624999999999645, 19.09188309203660694 ) ) ;
#17102 = DIRECTION ( 'NONE',  ( 0.000000000000000000, 0.000000000000000000, -1.000000000000000000 ) ) ;
#17103 = CARTESIAN_POINT ( 'NONE',  ( 0.000000000000000000, 16.99999999999998579, -24.50000000000000000 ) ) ;
#17104 = CARTESIAN_POINT ( 'NONE',  ( -26.29305231718578995, 68.20000000000000284, 19.10302069950538595 ) ) ;
#17105 = CARTESIAN_POINT ( 'NONE',  ( -4.523095164977117273E-15, 14.12499999726881050, 24.62258325217400312 ) ) ;
#17106 = CARTESIAN_POINT ( 'NONE',  ( 26.02091320914876960, 25.88763916574269075, 14.97647472619900455 ) ) ;
#17107 = CARTESIAN_POINT ( 'NONE',  ( -14.47279130897152122, 4.424999997268826313, 19.92008829642072243 ) ) ;
#17108 = CARTESIAN_POINT ( 'NONE',  ( 19.11951029504797006, 36.34336833240934794, 19.06425588902558133 ) ) ;
#17109 = CARTESIAN_POINT ( 'NONE',  ( 10.37757302488624056, 76.77500000273117564, -31.93888565452638417 ) ) ;
#17110 = CARTESIAN_POINT ( 'NONE',  ( -20.75514604977248823, 10.82500000273118701, -28.56700777964554305 ) ) ;
#17111 = CARTESIAN_POINT ( 'NONE',  ( -18.94512977948576093, 14.32499999726882756, 13.76444248337722698 ) ) ;
#17112 = CARTESIAN_POINT ( 'NONE',  ( 13.97622843553633665, 58.54947916666665009, 24.20753774853730889 ) ) ;
#17113 = ADVANCED_FACE ( 'NONE', ( #2192 ), #33602, .F. ) ;
#17114 = ORIENTED_EDGE ( 'NONE', *, *, #33702, .T. ) ;
#17115 = CARTESIAN_POINT ( 'NONE',  ( -33.58253175000000113, 49.22500000273119269, 10.91162601494193929 ) ) ;
#17116 = CARTESIAN_POINT ( 'NONE',  ( -10.37757302488624411, 20.97500000273118559, -31.93888565452638417 ) ) ;
#17117 = EDGE_LOOP ( 'NONE', ( #310, #3441, #13493, #3436 ) ) ;
#17118 = CARTESIAN_POINT ( 'NONE',  ( -20.50609665441004736, 22.31250000000000000, -20.50609665440969565 ) ) ;
#17119 = CARTESIAN_POINT ( 'NONE',  ( -14.97647472619946285, 20.45611083425730925, -26.02091320914851025 ) ) ;
#17120 = CARTESIAN_POINT ( 'NONE',  ( 32.50000000000000711, 38.89999999999999147, 10.55989012756945122 ) ) ;
#17121 = CARTESIAN_POINT ( 'NONE',  ( 24.50000000000000355, 15.84999999453763664, -7.960532557706203605 ) ) ;
#17122 = EDGE_CURVE ( 'NONE', #6224, #29257, #6398, .T. ) ;
#17123 = CARTESIAN_POINT ( 'NONE',  ( -18.94512977948576093, 5.824999997268820451, 13.76444248337722698 ) ) ;
#17124 = CARTESIAN_POINT ( 'NONE',  ( 33.58253175000000823, 24.27500000273120051, 10.91162601494192863 ) ) ;
#17125 = CARTESIAN_POINT ( 'NONE',  ( -32.50000000000000000, 26.40000000546236336, -10.55989012756945478 ) ) ;
#17126 = VECTOR ( 'NONE', #4265, 1000.000000000000000 ) ;
#17127 = CARTESIAN_POINT ( 'NONE',  ( 32.50000000000000000, 75.09999999999999432, -10.55989012756945833 ) ) ;
#17128 = DIRECTION ( 'NONE',  ( -1.000000000000000000, -1.309225264888156377E-16, 0.000000000000000000 ) ) ;
#17129 = CARTESIAN_POINT ( 'NONE',  ( -11.79757697019589457, 74.00000000000001421, 8.763667255710268833 ) ) ;
#17130 = CARTESIAN_POINT ( 'NONE',  ( 26.02091320914851025, 55.69048583425730925, -14.97647472619946463 ) ) ;
#17131 = CARTESIAN_POINT ( 'NONE',  ( -27.16883889988623935, 39.57500000273117280, 19.73931689729374739 ) ) ;
#17132 = CARTESIAN_POINT ( 'NONE',  ( -27.16883889988623935, 57.32500000273120833, 19.73931689729374739 ) ) ;
#17133 = CARTESIAN_POINT ( 'NONE',  ( 15.01150461594596486, 33.34114583333332860, -26.00068869287367690 ) ) ;
#17134 = DIRECTION ( 'NONE',  ( 0.000000000000000000, -1.000000000000000000, 0.000000000000000000 ) ) ;
#17135 = EDGE_CURVE ( 'NONE', #7428, #29891, #5269, .T. ) ;
#17136 = TOROIDAL_SURFACE ( 'NONE', #19340, 11.45223628611452860, 2.000000000000014211 ) ;
#17137 = CARTESIAN_POINT ( 'NONE',  ( 14.47279130897151589, 12.82499999726882400, 19.92008829642072953 ) ) ;
#17138 = CARTESIAN_POINT ( 'NONE',  ( -32.50000000000000000, 15.89999999999999147, -10.55989012756945478 ) ) ;
#17139 = CARTESIAN_POINT ( 'NONE',  ( 15.14183272437242245, 16.30000000000001137, -20.84094480462497856 ) ) ;
#17140 = CARTESIAN_POINT ( 'NONE',  ( 26.09010956794244507, 42.93190999907601935, 6.950374756619249084 ) ) ;
#17141 = CARTESIAN_POINT ( 'NONE',  ( 33.58253175000000113, 56.12500000273118417, -4.112674001490185761E-15 ) ) ;
#17142 = CARTESIAN_POINT ( 'NONE',  ( 6.486482029760648627E-15, 47.87500000273117706, 35.31076352940722529 ) ) ;
#17143 = CARTESIAN_POINT ( 'NONE',  ( -18.94512977948575738, 13.42499999726881654, -13.76444248337723231 ) ) ;
#17144 = CARTESIAN_POINT ( 'NONE',  ( 26.29305231718579350, 67.30000000546237970, 19.10302069950537529 ) ) ;
#17145 = CARTESIAN_POINT ( 'NONE',  ( -10.04305231718578462, 50.39999999999999858, 30.90933677959249337 ) ) ;
#17146 = CARTESIAN_POINT ( 'NONE',  ( 26.06988505166735592, 52.68267333425730214, 7.025853678916393896 ) ) ;
#17147 = CARTESIAN_POINT ( 'NONE',  ( -23.09300878900790366, 16.99999999999999289, -7.697900481730200362 ) ) ;
#17148 = CARTESIAN_POINT ( 'NONE',  ( 33.58253175000000113, 20.22500000273117848, -10.91162601494193751 ) ) ;
#17149 = DIRECTION ( 'NONE',  ( -1.000000000000000000, 0.000000000000000000, 0.000000000000000000 ) ) ;
#17150 = CARTESIAN_POINT ( 'NONE',  ( 5.147494310547327423, 52.55125428154686062, 32.50000000000003553 ) ) ;
#17151 = CARTESIAN_POINT ( 'NONE',  ( 2.667360163309149608E-15, 78.00000000546238255, -32.50000000000000000 ) ) ;
#17152 = CARTESIAN_POINT ( 'NONE',  ( -26.02091320914878025, 65.41888916574268364, -14.97647472619899389 ) ) ;
#17153 = CARTESIAN_POINT ( 'NONE',  ( 26.29305231718578995, 39.70000000546237828, -19.10302069950538240 ) ) ;
#17154 = CARTESIAN_POINT ( 'NONE',  ( 5.147494310547426899, 35.44874571845313227, -32.50000000000000000 ) ) ;
#17156 = CARTESIAN_POINT ( 'NONE',  ( 33.58253175000000113, 32.12500000273119127, -4.112674001490185761E-15 ) ) ;
#17155 = VECTOR ( 'NONE', #14737, 1000.000000000000000 ) ;
#17157 = CARTESIAN_POINT ( 'NONE',  ( -33.58253175000000113, 65.47500000273117848, 10.91162601494193929 ) ) ;
#17158 = CARTESIAN_POINT ( 'NONE',  ( 24.20753774853756113, 37.63802083333331439, 13.97622843553589789 ) ) ;
#17159 = ORIENTED_EDGE ( 'NONE', *, *, #17836, .T. ) ;
#17160 = VECTOR ( 'NONE', #21201, 1000.000000000000000 ) ;
#17161 = CARTESIAN_POINT ( 'NONE',  ( 20.75514604977249178, 73.82500000273121543, 28.56700777964553950 ) ) ;
#17162 = CARTESIAN_POINT ( 'NONE',  ( 26.00068869287340334, 37.06510416666666430, -15.01150461594642316 ) ) ;
#17163 = CARTESIAN_POINT ( 'NONE',  ( 0.000000000000000000, 74.00000000000001421, 15.00000000000000000 ) ) ;
#17164 = VERTEX_POINT ( 'NONE', #24159 ) ;
#17165 = CARTESIAN_POINT ( 'NONE',  ( 7.543491769121427382, 48.38579833425730925, -28.00173670424548433 ) ) ;
#17166 = CARTESIAN_POINT ( 'NONE',  ( 32.50000000000000000, 13.50000000546237899, -3.980102097228898626E-15 ) ) ;
#17168 = CARTESIAN_POINT ( 'NONE',  ( 20.50609665441005092, 65.28125000000000000, 20.50609665440969209 ) ) ;
#17167 = VECTOR ( 'NONE', #15597, 1000.000000000000000 ) ;
#17169 = CARTESIAN_POINT ( 'NONE',  ( -33.58253175000000113, 41.47500000273117138, 10.91162601494193929 ) ) ;
#17170 = CARTESIAN_POINT ( 'NONE',  ( -20.08610463437156923, 44.80000000546235839, 27.64615127144130113 ) ) ;
#17171 = CARTESIAN_POINT ( 'NONE',  ( 8.601468415847520532, 72.07500000273117280, 11.83890561707634781 ) ) ;
#17172 = CARTESIAN_POINT ( 'NONE',  ( 20.75514604977249178, 29.82500000273119767, 28.56700777964553950 ) ) ;
#17173 = CARTESIAN_POINT ( 'NONE',  ( 15.14183272437242067, 13.44999999453762385, 20.84094480462498211 ) ) ;
#17174 = CARTESIAN_POINT ( 'NONE',  ( 10.37757302488624056, 52.77500000273118985, -31.93888565452638417 ) ) ;
#17175 = CARTESIAN_POINT ( 'NONE',  ( 32.50000000000000000, 37.09999999999999432, -10.55989012756945833 ) ) ;
#17176 = CARTESIAN_POINT ( 'NONE',  ( 26.29305231718578995, 31.20000000000000639, -19.10302069950538240 ) ) ;
#17177 = CARTESIAN_POINT ( 'NONE',  ( 23.41746825000000243, 12.52499999726880375, 7.608796670333735079 ) ) ;
#17178 = CARTESIAN_POINT ( 'NONE',  ( 10.37757302488624767, 77.72500000273119269, 31.93888565452638417 ) ) ;
#17179 = CARTESIAN_POINT ( 'NONE',  ( 0.000000000000000000, 74.00000000000001421, 0.000000000000000000 ) ) ;
#17180 = CARTESIAN_POINT ( 'NONE',  ( -4.300734207923759378, 76.97500000273122112, -13.23629886949340495 ) ) ;
#17181 = CARTESIAN_POINT ( 'NONE',  ( -27.16883889988623935, 63.57500000273119412, 19.73931689729374739 ) ) ;
#17182 = CARTESIAN_POINT ( 'NONE',  ( 4.635254915624209993, 75.65000000546234560, -14.26584774442730463 ) ) ;
#17183 = AXIS2_PLACEMENT_3D ( 'NONE', #2593, #12714, #10316 ) ;
#17184 = ORIENTED_EDGE ( 'NONE', *, *, #14259, .F. ) ;
#17185 = CARTESIAN_POINT ( 'NONE',  ( 24.50000000000000355, 3.649999994537613812, 7.960532557706212486 ) ) ;
#17186 = CARTESIAN_POINT ( 'NONE',  ( 14.01125832528286352, 17.59152750092397355, -24.18731323226246843 ) ) ;
#17187 = CARTESIAN_POINT ( 'NONE',  ( 12.86449124955741041, 74.00000000000001421, -5.310441354522136947 ) ) ;
#17188 = CARTESIAN_POINT ( 'NONE',  ( -10.37757302488624411, 42.72500000273119980, -31.93888565452638417 ) ) ;
#17189 = CARTESIAN_POINT ( 'NONE',  ( 10.37757302488624056, 6.775000002731193405, -31.93888565452638417 ) ) ;
#17190 = CARTESIAN_POINT ( 'NONE',  ( -20.75514604977248823, 59.07500000273120122, -28.56700777964554305 ) ) ;
#17191 = CARTESIAN_POINT ( 'NONE',  ( -24.20753774853730889, 55.97135416666665719, 13.97622843553634020 ) ) ;
#17192 = CARTESIAN_POINT ( 'NONE',  ( -15.04653450569291984, 36.49777750092397355, 25.98046417659859486 ) ) ;
#17193 = CARTESIAN_POINT ( 'NONE',  ( -30.02300923189239867, 34.19493083240935505, 0.04044903255044988294 ) ) ;
#17194 = CARTESIAN_POINT ( 'NONE',  ( -32.50000000000000000, 64.40000000546238823, -10.55989012756945478 ) ) ;
#17195 = CARTESIAN_POINT ( 'NONE',  ( -13.91746824999999887, 72.87500000273122680, 0.000000000000000000 ) ) ;
#17196 = CARTESIAN_POINT ( 'NONE',  ( -24.22776226481266448, 55.10638916574269786, -13.94119854578892514 ) ) ;
#17197 =( BOUNDED_CURVE ( )  B_SPLINE_CURVE ( 2, ( #10668, #31757, #21147, #5688, #31589, #18575, #29016, #5852, #15997, #26621, #16331, #3117, #26787 ),
 .UNSPECIFIED., .F., .T. ) 
 B_SPLINE_CURVE_WITH_KNOTS ( ( 3, 2, 2, 2, 2, 2, 3 ),
 ( 0.05769230769230769551, 0.05897435897435897301, 0.06153846153846154188, 0.06410256410256409687, 0.06666666666666666574, 0.06923076923076923461, 0.07051282051282051211 ),
 .UNSPECIFIED. ) 
 CURVE ( )  GEOMETRIC_REPRESENTATION_ITEM ( )  RATIONAL_B_SPLINE_CURVE ( ( 0.9755282581475768211, 0.9755282581475768211, 1.000000000000000000, 0.9510565162951535312, 1.000000000000000000, 0.9510565162951535312, 1.000000000000000000, 0.9510565162951535312, 1.000000000000000000, 0.9510565162951535312, 1.000000000000000000, 0.9755282581475768211, 0.9755282581475768211 ) ) 
 REPRESENTATION_ITEM ( '' )  );
#17198 = CARTESIAN_POINT ( 'NONE',  ( -26.29305231718578995, 58.20000000000000284, 19.10302069950538595 ) ) ;
#17199 = CARTESIAN_POINT ( 'NONE',  ( 9.270509831248421762, 79.29999999999999716, -12.75976212528059861 ) ) ;
#17200 = CARTESIAN_POINT ( 'NONE',  ( -2.162160676586881955E-15, 40.87500000273119838, -35.31076352940723240 ) ) ;
#17201 = CARTESIAN_POINT ( 'NONE',  ( 7.890940483122900408E-14, 16.49999999999999645, -24.50000000000000000 ) ) ;
#17202 = CARTESIAN_POINT ( 'NONE',  ( -10.04305231718578462, 32.90000000546238113, 30.90933677959249337 ) ) ;
#17203 = EDGE_LOOP ( 'NONE', ( #32497, #3684, #14969, #14449, #27444, #7062, #29804, #5302, #28391, #2303, #18737, #14079, #16821, #16614, #29049, #2793, #26328, #9832, #29842, #33491, #26161, #29629, #14490, #16162, #13870, #5048, #16186, #26493, #8168, #18943, #18901, #31719, #16246, #25061, #20728, #26941, #21022, #6302, #20309, #14118, #13434, #3848, #6553, #21732, #30472, #20997, #14750, #20071, #561, #3324, #14576, #11718, #11618, #22060, #13709, #24623, #15096, #26304, #13953, #9506, #24419, #19520, #17719, #16388, #27238, #22008, #7995, #32218, #11407, #3500, #21358, #26537, #398, #6591, #10184, #27409, #27194, #15011, #17372, #16693, #7579, #31383 ) ) ;
#17204 = CARTESIAN_POINT ( 'NONE',  ( 15.01150461594643204, 34.48697916666667140, 26.00068869287340334 ) ) ;
#17206 = ORIENTED_EDGE ( 'NONE', *, *, #2377, .F. ) ;
#17205 = EDGE_CURVE ( 'NONE', #11228, #19151, #23994, .T. ) ;
#17207 = CARTESIAN_POINT ( 'NONE',  ( -2.162160676586881955E-15, 50.62500000273118417, -35.31076352940723240 ) ) ;
#17208 = CARTESIAN_POINT ( 'NONE',  ( 26.29305231718578995, 55.70000000546237828, -19.10302069950538240 ) ) ;
#17209 = DIRECTION ( 'NONE',  ( -0.000000000000000000, 0.000000000000000000, -1.000000000000000000 ) ) ;
#17210 = EDGE_CURVE ( 'NONE', #8282, #22733, #29803, .T. ) ;
#17211 = CARTESIAN_POINT ( 'NONE',  ( -10.04305231718578462, 12.90000000546237580, 30.90933677959249337 ) ) ;
#17212 = CARTESIAN_POINT ( 'NONE',  ( -31.04172217648553556, 66.99999999999998579, -12.81397374188210136 ) ) ;
#17213 = CARTESIAN_POINT ( 'NONE',  ( 23.41746824999999887, 15.12499999726882294, 0.000000000000000000 ) ) ;
#17214 = CARTESIAN_POINT ( 'NONE',  ( 26.29305231718578995, 51.19999999999999574, -19.10302069950538240 ) ) ;
#17215 = CARTESIAN_POINT ( 'NONE',  ( 12.13525491562420910, 77.45000000546237118, -8.816778784387098611 ) ) ;
#17216 = CARTESIAN_POINT ( 'NONE',  ( -27.16883889988624290, 17.17500000273119909, -19.73931689729374028 ) ) ;
#17217 = FILL_AREA_STYLE_COLOUR ( '', #20050 ) ;
#17218 = CARTESIAN_POINT ( 'NONE',  ( 24.22776226481265383, 25.88763916574269075, 13.94119854578893580 ) ) ;
#17219 = CARTESIAN_POINT ( 'NONE',  ( -13.91746824999999532, 76.97500000273119269, 4.522059556121122093 ) ) ;
#17220 = CARTESIAN_POINT ( 'NONE',  ( 3.880418787951121828, 8.448745718453148257, -24.50000000000000355 ) ) ;
#17221 = CARTESIAN_POINT ( 'NONE',  ( 20.08610463437157279, 53.80000000546237970, -27.64615127144129758 ) ) ;
#17222 = CARTESIAN_POINT ( 'NONE',  ( -20.08610463437156923, 2.299999999999999822, 27.64615127144130113 ) ) ;
#17223 = ORIENTED_EDGE ( 'NONE', *, *, #21026, .T. ) ;
#17224 = CARTESIAN_POINT ( 'NONE',  ( -7.236395654485763274, 4.524999997268825069, 22.27133577429736633 ) ) ;
#17225 = CARTESIAN_POINT ( 'NONE',  ( 26.07999730980477437, 40.64583333333332860, -6.988114217768290004 ) ) ;
#17226 = CARTESIAN_POINT ( 'NONE',  ( -33.58253175000000113, 67.12500000273118417, 0.000000000000000000 ) ) ;
#17227 = CARTESIAN_POINT ( 'NONE',  ( -20.75514604977248112, 25.67500000273118488, 28.56700777964554661 ) ) ;
#17228 = CARTESIAN_POINT ( 'NONE',  ( -33.58253175000000113, 7.375000002731183280, 0.000000000000000000 ) ) ;
#17229 = CARTESIAN_POINT ( 'NONE',  ( 10.37757302488624767, 11.97500000273118914, 31.93888565452638417 ) ) ;
#17230 = CARTESIAN_POINT ( 'NONE',  ( 20.47846945139902530, 15.15663166759064495, 20.53372385742071771 ) ) ;
#17231 = CARTESIAN_POINT ( 'NONE',  ( -20.50609665440969209, 52.39062499999999289, 20.50609665441005092 ) ) ;
#17232 = CARTESIAN_POINT ( 'NONE',  ( 20.08610463437158344, 2.700000000000001954, 27.64615127144129403 ) ) ;
#17233 = CARTESIAN_POINT ( 'NONE',  ( 26.29305231718579350, 46.79999999999999716, 19.10302069950537529 ) ) ;
#17234 = CARTESIAN_POINT ( 'NONE',  ( 5.779280353836490358E-15, 57.00000000546238965, 32.49999999999999289 ) ) ;
#17235 = CARTESIAN_POINT ( 'NONE',  ( 33.58253175000000113, 50.12500000273117706, -4.112674001490185761E-15 ) ) ;
#17236 = CARTESIAN_POINT ( 'NONE',  ( -7.236395654485763274, 2.024999997268822405, 22.27133577429736633 ) ) ;
#17237 = PRODUCT_DEFINITION_SHAPE ( 'NONE', 'NONE',  #33998 ) ;
#17238 = ORIENTED_EDGE ( 'NONE', *, *, #7688, .F. ) ;
#17239 = CARTESIAN_POINT ( 'NONE',  ( -33.58253175000000113, 59.27500000273119696, -10.91162601494193218 ) ) ;
#17240 = CARTESIAN_POINT ( 'NONE',  ( 5.779280353836490358E-15, 58.49999999999999289, 32.49999999999999289 ) ) ;
#17241 = CARTESIAN_POINT ( 'NONE',  ( -23.41746825000000598, 11.72499999726882614, 7.608796670333726198 ) ) ;
#17242 = CARTESIAN_POINT ( 'NONE',  ( 7.025853678916403666, 31.19829833425730570, -26.06988505166735237 ) ) ;
#17243 = VERTEX_POINT ( 'NONE', #3226 ) ;
#17244 = CARTESIAN_POINT ( 'NONE',  ( 20.75514604977249178, 29.82500000273119767, 28.56700777964553950 ) ) ;
#17245 = CARTESIAN_POINT ( 'NONE',  ( -15.00000000000000000, 74.00000000000001421, 0.000000000000000000 ) ) ;
#17246 = COLOUR_RGB ( '', 0.08235294, 0.09019608, 0.10196078) ;
#17247 = VERTEX_POINT ( 'NONE', #629 ) ;
#17248 = CARTESIAN_POINT ( 'NONE',  ( 15.01150461594643204, 61.98697916666665009, 26.00068869287340334 ) ) ;
#17249 = CARTESIAN_POINT ( 'NONE',  ( -2.162160676586881955E-15, 60.87500000273116996, -35.31076352940723240 ) ) ;
#17250 = FACE_OUTER_BOUND ( 'NONE', #12579, .T. ) ;
#17251 = CARTESIAN_POINT ( 'NONE',  ( 10.37757302488624767, 67.72500000273117848, 31.93888565452638417 ) ) ;
#17252 = CARTESIAN_POINT ( 'NONE',  ( -26.00068869287368756, 32.48177083333332860, -15.01150461594595775 ) ) ;
#17253 = CARTESIAN_POINT ( 'NONE',  ( -7.570916362186210335, 12.59999999999999964, -23.30088464923126779 ) ) ;
#17254 = CARTESIAN_POINT ( 'NONE',  ( -33.58253175000000113, 5.475000002731181148, 10.91162601494193929 ) ) ;
#17255 = CARTESIAN_POINT ( 'NONE',  ( -27.16883889988624290, 12.92500000273116889, -19.73931689729374028 ) ) ;
#17256 = CARTESIAN_POINT ( 'NONE',  ( 13.91746824999999532, 71.97500000273120691, -4.522059556121118540 ) ) ;
#17257 = CARTESIAN_POINT ( 'NONE',  ( -15.04653450569338524, 45.08034749907603356, -25.98046417659831775 ) ) ;
#17258 = CARTESIAN_POINT ( 'NONE',  ( -28.01184896238290278, 59.55208333333332149, 7.505752307973363457 ) ) ;
#17259 = CARTESIAN_POINT ( 'NONE',  ( 20.08610463437158344, 22.70000000000000995, 27.64615127144129403 ) ) ;
#17260 = CARTESIAN_POINT ( 'NONE',  ( -7.570916362186210335, 8.349999994537615322, -23.30088464923126779 ) ) ;
#17261 = CARTESIAN_POINT ( 'NONE',  ( 15.00000000000000000, 77.35000000546237686, -4.873795443493596835 ) ) ;
#17262 = CARTESIAN_POINT ( 'NONE',  ( -6.988114217767819270, 17.72916666666666430, 26.07999730980490583 ) ) ;
#17263 = CARTESIAN_POINT ( 'NONE',  ( 33.58253175000000113, 38.22500000273119269, -10.91162601494193751 ) ) ;
#17264 = CARTESIAN_POINT ( 'NONE',  ( -11.25946833292375793, 75.07500000273120122, 8.180482586598737171 ) ) ;
#17265 = CARTESIAN_POINT ( 'NONE',  ( -20.75514604977248112, 43.67500000273119554, 28.56700777964554661 ) ) ;
#17266 = CARTESIAN_POINT ( 'NONE',  ( 10.37757302488624056, 28.77500000273120051, -31.93888565452638417 ) ) ;
#17267 = CARTESIAN_POINT ( 'NONE',  ( 0.000000000000000000, 16.99999999999998579, -24.50000000000000000 ) ) ;
#17268 = CARTESIAN_POINT ( 'NONE',  ( 24.50000000000000000, 2.099999999999991651, -7.960532557706203605 ) ) ;
#17269 = VECTOR ( 'NONE', #12288, 1000.000000000000000 ) ;
#17270 = CARTESIAN_POINT ( 'NONE',  ( 5.147494310547428675, 78.55125428154684641, 32.50000000000000000 ) ) ;
#17271 = CARTESIAN_POINT ( 'NONE',  ( -32.50000000000000000, 69.90000000000000568, -10.55989012756945478 ) ) ;
#17272 = CARTESIAN_POINT ( 'NONE',  ( -23.41746825000000243, 9.724999997268803043, 7.608796670333725309 ) ) ;
#17273 = CARTESIAN_POINT ( 'NONE',  ( 25.98046417659831775, 21.87722249907602290, -15.04653450569338879 ) ) ;
#17274 = CARTESIAN_POINT ( 'NONE',  ( -15.00000000000000000, 77.89999999999997726, -4.873795443493594171 ) ) ;
#17275 = CARTESIAN_POINT ( 'NONE',  ( 13.94119854578893580, 38.77826416574269075, -24.22776226481265383 ) ) ;
#17276 = SURFACE_SIDE_STYLE ('',( #12113 ) ) ;
#17277 = CARTESIAN_POINT ( 'NONE',  ( -10.37757302488623701, 15.52500000273118808, 31.93888565452638417 ) ) ;
#17278 = CARTESIAN_POINT ( 'NONE',  ( 7.236395654485755280, 10.72499999726880837, 22.27133577429736988 ) ) ;
#17279 = CARTESIAN_POINT ( 'NONE',  ( -26.07999730980477437, 62.98958333333332149, 6.988114217768305103 ) ) ;
#17280 = ORIENTED_EDGE ( 'NONE', *, *, #31175, .T. ) ;
#17281 = CARTESIAN_POINT ( 'NONE',  ( -20.75514604977248112, 51.42500000273118133, 28.56700777964554661 ) ) ;
#17282 = CARTESIAN_POINT ( 'NONE',  ( 33.58253175000000113, 20.37500000273119483, -4.112674001490185761E-15 ) ) ;
#17283 = ORIENTED_EDGE ( 'NONE', *, *, #13886, .T. ) ;
#17284 = CARTESIAN_POINT ( 'NONE',  ( 28.01184896238304134, 30.61979166666666075, 7.505752307972846538 ) ) ;
#17285 = CARTESIAN_POINT ( 'NONE',  ( 14.97647472619947351, 32.48736083425731636, 26.02091320914850314 ) ) ;
#17286 = CARTESIAN_POINT ( 'NONE',  ( -15.14183272437242778, 3.300000000000012257, 20.84094480462497856 ) ) ;
#17287 = CARTESIAN_POINT ( 'NONE',  ( -15.14183272437241889, 14.44999999453762207, -20.84094480462497856 ) ) ;
#17288 = CARTESIAN_POINT ( 'NONE',  ( 1.507698388325705758E-15, 13.12499999726881228, -24.62258325217400312 ) ) ;
#17289 = CARTESIAN_POINT ( 'NONE',  ( 10.37757302488624767, 21.97500000273119980, 31.93888565452638417 ) ) ;
#17290 = VECTOR ( 'NONE', #11134, 1000.000000000000000 ) ;
#17291 = CARTESIAN_POINT ( 'NONE',  ( 20.08610463437158344, 27.20000000546237118, 27.64615127144129403 ) ) ;
#17292 =( BOUNDED_CURVE ( )  B_SPLINE_CURVE ( 2, ( #24759, #17389, #17562, #1412, #1237, #30582, #22198, #7078, #11715, #22874, #33332, #32976, #27854 ),
 .UNSPECIFIED., .F., .T. ) 
 B_SPLINE_CURVE_WITH_KNOTS ( ( 3, 2, 2, 2, 2, 2, 3 ),
 ( 0.3012820512820512664, 0.3025641025641025439, 0.3051282051282051544, 0.3076923076923077094, 0.3102564102564102644, 0.3128205128205128194, 0.3141025641025640969 ),
 .UNSPECIFIED. ) 
 CURVE ( )  GEOMETRIC_REPRESENTATION_ITEM ( )  RATIONAL_B_SPLINE_CURVE ( ( 0.9755282581475768211, 0.9755282581475768211, 1.000000000000000000, 0.9510565162951535312, 1.000000000000000000, 0.9510565162951535312, 1.000000000000000000, 0.9510565162951535312, 1.000000000000000000, 0.9510565162951535312, 1.000000000000000000, 0.9755282581475768211, 0.9755282581475768211 ) ) 
 REPRESENTATION_ITEM ( '' )  );
#17293 = CARTESIAN_POINT ( 'NONE',  ( -32.50000000000000000, 70.10000000000000853, 10.55989012756946366 ) ) ;
#17294 = CARTESIAN_POINT ( 'NONE',  ( -10.04305231718579172, 6.100000005462375086, -30.90933677959248982 ) ) ;
#17295 = CARTESIAN_POINT ( 'NONE',  ( 5.147494310547434893, 66.55125428154683220, 32.49999999999999289 ) ) ;
#17296 = CARTESIAN_POINT ( 'NONE',  ( -15.04653450569291984, 53.68527750092398065, 25.98046417659859486 ) ) ;
#17297 = CARTESIAN_POINT ( 'NONE',  ( -33.58253175000000113, 37.27500000273119696, -10.91162601494193218 ) ) ;
#17298 = CARTESIAN_POINT ( 'NONE',  ( -27.16883889988624290, 54.92500000273118843, -19.73931689729374028 ) ) ;
#17299 = CARTESIAN_POINT ( 'NONE',  ( -7.505752307973343918, 32.91145833333332860, -28.01184896238290989 ) ) ;
#17300 = DIRECTION ( 'NONE',  ( 0.000000000000000000, 0.000000000000000000, 1.000000000000000000 ) ) ;
#17301 = CARTESIAN_POINT ( 'NONE',  ( -23.41746824999999887, 8.124999997268817609, -2.867812753649727150E-15 ) ) ;
#17302 = CARTESIAN_POINT ( 'NONE',  ( 10.04305231718578817, 17.39999999999999858, -30.90933677959249337 ) ) ;
#17303 = CARTESIAN_POINT ( 'NONE',  ( 32.50000000000000000, 9.500000005462361230, -3.980102097228898626E-15 ) ) ;
#17304 = CARTESIAN_POINT ( 'NONE',  ( 13.94119854578893580, 45.65326416574269786, -24.22776226481265383 ) ) ;
#17305 = CARTESIAN_POINT ( 'NONE',  ( 10.37757302488624767, 55.72500000273117138, 31.93888565452638417 ) ) ;
#17306 = AXIS2_PLACEMENT_3D ( 'NONE', #24553, #8599, #32101 ) ;
#17307 = CARTESIAN_POINT ( 'NONE',  ( -20.75514604977248112, 47.67500000273118843, 28.56700777964554661 ) ) ;
#17308 = CARTESIAN_POINT ( 'NONE',  ( 0.000000000000000000, 80.00000000000001421, 0.000000000000000000 ) ) ;
#17309 = CARTESIAN_POINT ( 'NONE',  ( 24.50000000000000000, 9.900000000000007461, 7.960532557706212486 ) ) ;
#17310 = CARTESIAN_POINT ( 'NONE',  ( 27.16883889988624290, 1.925000002731186433, 19.73931689729373673 ) ) ;
#17311 = CARTESIAN_POINT ( 'NONE',  ( 7.025853678916403666, 48.38579833425730925, -26.06988505166735237 ) ) ;
#17312 = CARTESIAN_POINT ( 'NONE',  ( -19.82091636218621389, 4.949999994537629178, 14.40073868116558842 ) ) ;
#17313 = CARTESIAN_POINT ( 'NONE',  ( 10.17814985357209245, -45.51763809020504681, 0.000000000000000000 ) ) ;
#17314 = CARTESIAN_POINT ( 'NONE',  ( 6.486482029760649416E-15, 23.62500000273119127, 35.31076352940723240 ) ) ;
#17315 = DIRECTION ( 'NONE',  ( 0.000000000000000000, 1.000000000000000000, 0.000000000000000000 ) ) ;
#17316 = CARTESIAN_POINT ( 'NONE',  ( 3.445340210940985210E-14, 9.249999994537636994, 24.50000000000000000 ) ) ;
#17317 = CARTESIAN_POINT ( 'NONE',  ( 20.08610463437158344, 41.20000000546236407, 27.64615127144129403 ) ) ;
#17318 = CARTESIAN_POINT ( 'NONE',  ( -7.025853678916861966, 14.28607666574268720, -26.06988505166722803 ) ) ;
#17319 = CARTESIAN_POINT ( 'NONE',  ( 20.08610463437157279, 43.80000000546237970, -27.64615127144129758 ) ) ;
#17320 = CARTESIAN_POINT ( 'NONE',  ( -33.58253175000000113, 33.22500000273117138, 10.91162601494193929 ) ) ;
#17321 = CARTESIAN_POINT ( 'NONE',  ( 33.58253175000000823, 64.27500000273118985, 10.91162601494192863 ) ) ;
#17322 = CARTESIAN_POINT ( 'NONE',  ( -6.988114217768288228, 32.91145833333332860, -26.07999730980477437 ) ) ;
#17323 = ORIENTED_EDGE ( 'NONE', *, *, #19726, .F. ) ;
#17324 = CARTESIAN_POINT ( 'NONE',  ( 10.37757302488624056, 70.52500000273118985, -31.93888565452638417 ) ) ;
#17325 = CARTESIAN_POINT ( 'NONE',  ( -7.505752307973343918, 43.22395833333332860, -28.01184896238290989 ) ) ;
#17326 = CARTESIAN_POINT ( 'NONE',  ( 40.00000000000000000, 52.00000000000000711, 23.09401076758503990 ) ) ;
#17327 = ORIENTED_EDGE ( 'NONE', *, *, #29070, .F. ) ;
#17328 = CARTESIAN_POINT ( 'NONE',  ( 7.468012846824777284, 63.56809000092398065, 28.02196122052045268 ) ) ;
#17329 = CARTESIAN_POINT ( 'NONE',  ( 0.04044903254993986036, 58.55506916759063785, -27.95245687107223986 ) ) ;
#17330 = CIRCLE ( 'NONE', #6780, 26.50000000000000000 ) ;
#17331 = CARTESIAN_POINT ( 'NONE',  ( 27.16883889988623935, 8.325000002731188786, -19.73931689729374384 ) ) ;
#17332 = CARTESIAN_POINT ( 'NONE',  ( 20.50609665441005092, 61.84374999999998579, 20.50609665440969209 ) ) ;
#17333 = CARTESIAN_POINT ( 'NONE',  ( 5.779280353836490358E-15, 56.49999999999998579, 32.49999999999999289 ) ) ;
#17334 = CARTESIAN_POINT ( 'NONE',  ( 10.37757302488624767, 41.97500000273118559, 31.93888565452638417 ) ) ;
#17335 = CARTESIAN_POINT ( 'NONE',  ( -2.092463501923844636E-15, 44.00000000546238965, -34.17252228774368916 ) ) ;
#17336 = EDGE_CURVE ( 'NONE', #11703, #26987, #13860, .T. ) ;
#17337 = CARTESIAN_POINT ( 'NONE',  ( -11.25946833292375793, 75.57500000273120122, 8.180482586598737171 ) ) ;
#17338 = CARTESIAN_POINT ( 'NONE',  ( -27.16883889988624290, 30.92500000273118488, -19.73931689729374028 ) ) ;
#17339 = CARTESIAN_POINT ( 'NONE',  ( 7.570916362186207671, 13.34999999453762065, 23.30088464923126779 ) ) ;
#17340 = CARTESIAN_POINT ( 'NONE',  ( 27.16883889988623935, 54.57500000273118701, -19.73931689729374384 ) ) ;
#17341 = CARTESIAN_POINT ( 'NONE',  ( 32.50000000000000000, 38.99999999999999289, -3.980102097228898626E-15 ) ) ;
#17342 = CARTESIAN_POINT ( 'NONE',  ( 32.50000000000000000, 31.10000000000000497, -10.55989012756945833 ) ) ;
#17343 = CARTESIAN_POINT ( 'NONE',  ( 24.50000000000000355, 2.099999999999991651, -7.960532557706203605 ) ) ;
#17344 = CARTESIAN_POINT ( 'NONE',  ( 33.58253175000000823, 78.02500000273118985, 10.91162601494192863 ) ) ;
#17345 = CARTESIAN_POINT ( 'NONE',  ( -5.393181536354430428, 66.99999999999997158, 32.17179393301731949 ) ) ;
#17346 = CARTESIAN_POINT ( 'NONE',  ( 4.300734207923761154, 75.97500000273122112, 13.23629886949340495 ) ) ;
#17347 = CARTESIAN_POINT ( 'NONE',  ( -2.162160676586882350E-15, 66.87500000273119838, -35.31076352940722529 ) ) ;
#17348 = CARTESIAN_POINT ( 'NONE',  ( -15.00000000000000000, 78.15000000546238823, -4.873795443493594171 ) ) ;
#17349 = EDGE_CURVE ( 'NONE', #4016, #21770, #23921, .T. ) ;
#17350 = FACE_BOUND ( 'NONE', #7828, .T. ) ;
#17351 = CARTESIAN_POINT ( 'NONE',  ( 7.570916362186213000, 12.14999999453764090, -23.30088464923126423 ) ) ;
#17352 = CARTESIAN_POINT ( 'NONE',  ( -19.06425588902591173, 23.75038166759064140, -19.11951029504763611 ) ) ;
#17353 = CARTESIAN_POINT ( 'NONE',  ( -9.270509831248419985, 74.55000000546237970, 12.75976212528060039 ) ) ;
#17354 = CARTESIAN_POINT ( 'NONE',  ( 33.58253175000000113, 42.22500000273118559, -10.91162601494193751 ) ) ;
#17355 = CARTESIAN_POINT ( 'NONE',  ( 20.75514604977249178, 2.075000002731186122, 28.56700777964553950 ) ) ;
#17356 = CARTESIAN_POINT ( 'NONE',  ( -10.37757302488624411, 52.97500000273118559, -31.93888565452638417 ) ) ;
#17357 = CARTESIAN_POINT ( 'NONE',  ( 0.04044903254992426173, 48.24256916759064495, -30.02300923189239867 ) ) ;
#17358 = AXIS2_PLACEMENT_3D ( 'NONE', #14512, #9344, #19827 ) ;
#17359 = CARTESIAN_POINT ( 'NONE',  ( -30.02300923189239867, 37.63243083240935505, 0.04044903255044988294 ) ) ;
#17360 = CARTESIAN_POINT ( 'NONE',  ( -20.08610463437156923, 60.80000000546239391, 27.64615127144130113 ) ) ;
#17361 = CARTESIAN_POINT ( 'NONE',  ( -4.300734207923755825, 75.27500000273118985, 13.23629886949340673 ) ) ;
#17362 = CARTESIAN_POINT ( 'NONE',  ( -19.11951029504797006, 68.99961833240934084, -19.06425588902558133 ) ) ;
#17363 = CARTESIAN_POINT ( 'NONE',  ( -10.04305231718579172, 53.60000000000002274, -30.90933677959248982 ) ) ;
#17364 = AXIS2_PLACEMENT_3D ( 'NONE', #6593, #11910, #27529 ) ;
#17365 = CARTESIAN_POINT ( 'NONE',  ( -10.04305231718578462, 72.90000000546237402, 30.90933677959249337 ) ) ;
#17366 = CARTESIAN_POINT ( 'NONE',  ( 20.50609665440969565, 16.29687499999999645, -20.50609665441004736 ) ) ;
#17367 = CARTESIAN_POINT ( 'NONE',  ( -27.16883889988624290, 39.17500000273120264, -19.73931689729374028 ) ) ;
#17368 = LINE ( 'NONE', #30051, #11891 ) ;
#17369 = EDGE_LOOP ( 'NONE', ( #2732, #18965, #30821, #15442 ) ) ;
#17370 = CARTESIAN_POINT ( 'NONE',  ( 33.58253175000000113, 72.47500000273119269, -10.91162601494193751 ) ) ;
#17371 = CARTESIAN_POINT ( 'NONE',  ( 10.04305231718578817, 29.90000000546237757, -30.90933677959249337 ) ) ;
#17372 = ORIENTED_EDGE ( 'NONE', *, *, #25226, .F. ) ;
#17373 = CARTESIAN_POINT ( 'NONE',  ( 20.50609665440969565, 36.92187499999999289, -20.50609665441004736 ) ) ;
#17374 = CARTESIAN_POINT ( 'NONE',  ( -2.092463501923844636E-15, 60.00000000546238255, -34.17252228774368916 ) ) ;
#17375 = VERTEX_POINT ( 'NONE', #3390 ) ;
#17376 = CARTESIAN_POINT ( 'NONE',  ( -15.14183272437242067, 12.44999999453762918, -20.84094480462497856 ) ) ;
#17377 = CARTESIAN_POINT ( 'NONE',  ( -27.16883889988624290, 50.92500000273120264, -19.73931689729374028 ) ) ;
#17378 = CARTESIAN_POINT ( 'NONE',  ( 7.236395654485755280, 16.22499999726881370, 22.27133577429736988 ) ) ;
#17379 = CARTESIAN_POINT ( 'NONE',  ( -1.778240108872766143E-15, 17.50000000000000000, -32.49999999999999289 ) ) ;
#17380 = CARTESIAN_POINT ( 'NONE',  ( -20.08610463437156923, 2.800000005462385477, 27.64615127144130113 ) ) ;
#17381 = CARTESIAN_POINT ( 'NONE',  ( -33.58253175000000113, 65.12500000273118417, 0.000000000000000000 ) ) ;
#17382 = CARTESIAN_POINT ( 'NONE',  ( -7.236395654485757944, 13.72499999726881015, -22.27133577429736988 ) ) ;
#17383 = CARTESIAN_POINT ( 'NONE',  ( -10.04305231718578462, 52.40000000000000568, 30.90933677959249337 ) ) ;
#17384 = CARTESIAN_POINT ( 'NONE',  ( -23.41746825000000598, 1.724999997268824581, 7.608796670333726198 ) ) ;
#17385 = CARTESIAN_POINT ( 'NONE',  ( -10.37757302488623701, 15.77500000273118808, 31.93888565452638417 ) ) ;
#17386 = CARTESIAN_POINT ( 'NONE',  ( -15.14183272437242778, 7.300000000000001599, 20.84094480462497856 ) ) ;
#17387 = CARTESIAN_POINT ( 'NONE',  ( -19.11951029504797006, 20.87461833240935505, -19.06425588902558133 ) ) ;
#17388 = CARTESIAN_POINT ( 'NONE',  ( -11.25946833292375793, 73.07500000273120122, 8.180482586598737171 ) ) ;
#17389 = CARTESIAN_POINT ( 'NONE',  ( -5.147494310547423346, 56.44874571845313938, 32.50000000000000000 ) ) ;
#17390 = PLANE ( 'NONE',  #21598 ) ;
#17391 = AXIS2_PLACEMENT_3D ( 'NONE', #23339, #33801, #7541 ) ;
#17392 = CARTESIAN_POINT ( 'NONE',  ( 33.58253175000000113, 78.37500000273118417, -4.112674001490185761E-15 ) ) ;
#17393 = VERTEX_POINT ( 'NONE', #29125 ) ;
#17394 = CARTESIAN_POINT ( 'NONE',  ( 1.507698388325705758E-15, 7.624999997268814056, -24.62258325217400312 ) ) ;
#17395 = DIRECTION ( 'NONE',  ( -0.8660254037844385966, 0.000000000000000000, 0.5000000000000003331 ) ) ;
#17396 = CARTESIAN_POINT ( 'NONE',  ( -27.95245687107222921, 52.82031249999997868, 2.498001805406602216E-13 ) ) ;
#17397 = CARTESIAN_POINT ( 'NONE',  ( -10.37757302488623701, 59.52500000273118275, 31.93888565452638417 ) ) ;
#17398 = CARTESIAN_POINT ( 'NONE',  ( -33.58253175000000113, 23.47500000273119269, 10.91162601494193929 ) ) ;
#17399 = CARTESIAN_POINT ( 'NONE',  ( 20.75514604977249178, 8.075000002731185234, 28.56700777964553950 ) ) ;
#17400 = CARTESIAN_POINT ( 'NONE',  ( -10.04305231718578462, 20.40000000000000213, 30.90933677959249337 ) ) ;
#17401 = CARTESIAN_POINT ( 'NONE',  ( -20.47846945139902175, 20.31288166759063785, -20.53372385742072481 ) ) ;
#17402 = CARTESIAN_POINT ( 'NONE',  ( 28.01184896238304134, 64.99479166666665719, 7.505752307972846538 ) ) ;
#17403 = CARTESIAN_POINT ( 'NONE',  ( 10.37757302488624767, 1.725000002731180704, 31.93888565452638417 ) ) ;
#17404 = EDGE_CURVE ( 'NONE', #16018, #25987, #27408, .T. ) ;
#17405 = CARTESIAN_POINT ( 'NONE',  ( -13.91746824999999887, 71.37500000273119838, 0.000000000000000000 ) ) ;
#17406 = CARTESIAN_POINT ( 'NONE',  ( 6.277390505771533514E-15, 42.50000000000000000, 34.17252228774368916 ) ) ;
#17407 = CARTESIAN_POINT ( 'NONE',  ( 27.16883889988624290, 49.92500000273120264, 19.73931689729373673 ) ) ;
#17408 = ADVANCED_FACE ( 'NONE', ( #24982 ), #32696, .F. ) ;
#17409 = CARTESIAN_POINT ( 'NONE',  ( 14.47279130897151767, 0.9249999972688209837, -19.92008829642072598 ) ) ;
#17410 = CARTESIAN_POINT ( 'NONE',  ( -1.778240108872766143E-15, 22.00000000546237899, -32.49999999999999289 ) ) ;
#17411 = VERTEX_POINT ( 'NONE', #28072 ) ;
#17412 = CARTESIAN_POINT ( 'NONE',  ( 10.37757302488624767, 57.97500000273118559, 31.93888565452638417 ) ) ;
#17413 = DIRECTION ( 'NONE',  ( -0.000000000000000000, -1.000000000000000000, -0.000000000000000000 ) ) ;
#17414 = CARTESIAN_POINT ( 'NONE',  ( -18.94512977948576093, 9.824999997268824004, 13.76444248337722698 ) ) ;
#17415 = CARTESIAN_POINT ( 'NONE',  ( -24.22776226481240514, 29.90923583425730925, 13.94119854578937812 ) ) ;
#17416 = ORIENTED_EDGE ( 'NONE', *, *, #3887, .F. ) ;
#17417 = AXIS2_PLACEMENT_3D ( 'NONE', #3492, #5737, #19120 ) ;
#17418 = CARTESIAN_POINT ( 'NONE',  ( -2.162160676586881955E-15, 30.62500000273119838, -35.31076352940723240 ) ) ;
#17419 = CARTESIAN_POINT ( 'NONE',  ( 7.570916362186213000, 6.399999999999988809, -23.30088464923126423 ) ) ;
#17420 = ORIENTED_EDGE ( 'NONE', *, *, #17983, .T. ) ;
#17421 = CARTESIAN_POINT ( 'NONE',  ( -15.01150461594642138, 60.26822916666665009, -26.00068869287340334 ) ) ;
#17422 = FACE_OUTER_BOUND ( 'NONE', #9105, .T. ) ;
#17423 = CARTESIAN_POINT ( 'NONE',  ( -27.16883889988623935, 67.32500000273117280, 19.73931689729374739 ) ) ;
#17424 = CARTESIAN_POINT ( 'NONE',  ( -15.01150461594595775, 41.93489583333333570, 26.00068869287368756 ) ) ;
#17425 = CARTESIAN_POINT ( 'NONE',  ( 15.14183272437241889, 15.69999999999999929, 20.84094480462498211 ) ) ;
#17426 = CARTESIAN_POINT ( 'NONE',  ( -27.16883889988623935, 3.575000002731199000, 19.73931689729374739 ) ) ;
#17427 = CARTESIAN_POINT ( 'NONE',  ( 33.58253175000000113, 10.12500000273119838, -4.112674001490185761E-15 ) ) ;
#17428 = CARTESIAN_POINT ( 'NONE',  ( 4.300734207923757602, 74.27500000273118985, -13.23629886949340673 ) ) ;
#17429 = CARTESIAN_POINT ( 'NONE',  ( 26.02091320914876960, 49.95013916574269786, 14.97647472619900455 ) ) ;
#17430 = CARTESIAN_POINT ( 'NONE',  ( -9.657523855033125146E-16, 73.50000000000001421, -15.77193336357400710 ) ) ;
#17431 = CARTESIAN_POINT ( 'NONE',  ( -28.01184896238304134, 59.83854166666666430, -7.505752307972844761 ) ) ;
#17432 = CARTESIAN_POINT ( 'NONE',  ( 20.08610463437157279, 19.80000000546237615, -27.64615127144129758 ) ) ;
#17433 = CARTESIAN_POINT ( 'NONE',  ( -2.165007332552593587E-13, 52.50000000000000711, 32.50000000000000000 ) ) ;
#17434 = CARTESIAN_POINT ( 'NONE',  ( -24.50000000000000000, 6.749999994537625447, -3.000384657911015469E-15 ) ) ;
#17435 = CARTESIAN_POINT ( 'NONE',  ( -9.270509831248425314, 77.95000000546237118, -12.75976212528059861 ) ) ;
#17436 = CARTESIAN_POINT ( 'NONE',  ( -2.428612866367529427E-13, 26.17968750000000000, -27.95245687107222921 ) ) ;
#17437 = CARTESIAN_POINT ( 'NONE',  ( -33.58253175000000113, 35.22500000273119980, 10.91162601494193929 ) ) ;
#17438 = DIRECTION ( 'NONE',  ( 0.000000000000000000, 0.000000000000000000, -1.000000000000000000 ) ) ;
#17439 = CARTESIAN_POINT ( 'NONE',  ( 10.37757302488624767, 45.97500000273117848, 31.93888565452638417 ) ) ;
#17440 = CARTESIAN_POINT ( 'NONE',  ( -33.58253175000000113, 19.27500000273117919, -10.91162601494193041 ) ) ;
#17441 = CARTESIAN_POINT ( 'NONE',  ( 3.980102097228898626E-15, 80.00000000000001421, 32.50000000000000000 ) ) ;
#17442 = CARTESIAN_POINT ( 'NONE',  ( 3.880418787951139592, 1.551254281546846192, 24.50000000000000000 ) ) ;
#17443 = CIRCLE ( 'NONE', #33882, 27.00000000000000000 ) ;
#17444 = EDGE_CURVE ( 'NONE', #19766, #14943, #30918, .T. ) ;
#17445 = CARTESIAN_POINT ( 'NONE',  ( 2.667360163309149608E-15, 79.50000000000001421, -32.50000000000000000 ) ) ;
#17446 = CARTESIAN_POINT ( 'NONE',  ( 26.29305231718579350, 64.80000000000001137, 19.10302069950537529 ) ) ;
#17447 = CARTESIAN_POINT ( 'NONE',  ( 14.47279130897151944, 10.92499999726882365, -19.92008829642072598 ) ) ;
#17448 = CARTESIAN_POINT ( 'NONE',  ( -14.97647472619899389, 23.30951416574269075, 26.02091320914878025 ) ) ;
#17449 = EDGE_CURVE ( 'NONE', #21971, #31380, #19675, .T. ) ;
#17450 = FACE_OUTER_BOUND ( 'NONE', #11369, .T. ) ;
#17451 = CARTESIAN_POINT ( 'NONE',  ( -6.950374756619247307, 40.35378499907601935, 26.09010956794245217 ) ) ;
#17452 = CARTESIAN_POINT ( 'NONE',  ( 33.58253175000000113, 78.37500000273118417, -4.112674001490185761E-15 ) ) ;
#17453 = CARTESIAN_POINT ( 'NONE',  ( -2.162160676586882350E-15, 12.62500000273118772, -35.31076352940722529 ) ) ;
#17454 = CARTESIAN_POINT ( 'NONE',  ( -23.41746825000000598, 10.22499999726881903, 7.608796670333726198 ) ) ;
#17455 = CARTESIAN_POINT ( 'NONE',  ( 27.95245687107222921, 61.41406250000000711, -2.463307335887066074E-13 ) ) ;
#17456 = ORIENTED_EDGE ( 'NONE', *, *, #33247, .F. ) ;
#17457 = CARTESIAN_POINT ( 'NONE',  ( -20.75514604977248823, 50.82500000273116569, -28.56700777964554305 ) ) ;
#17458 = CARTESIAN_POINT ( 'NONE',  ( -10.37757302488624411, 22.97500000273118559, -31.93888565452638417 ) ) ;
#17459 = VERTEX_POINT ( 'NONE', #33205 ) ;
#17460 = CARTESIAN_POINT ( 'NONE',  ( 30.02300923189239512, 30.47656250000000355, -2.619432448724977703E-13 ) ) ;
#17461 = CARTESIAN_POINT ( 'NONE',  ( 28.02196122052045268, 31.77121500092397000, -7.468012846824774620 ) ) ;
#17462 = CARTESIAN_POINT ( 'NONE',  ( -5.147494310547403806, 72.05125428700921475, -32.50000000000000711 ) ) ;
#17463 = CARTESIAN_POINT ( 'NONE',  ( 23.41746824999999887, 5.124999997268814056, 0.000000000000000000 ) ) ;
#17464 = CARTESIAN_POINT ( 'NONE',  ( 18.94512977948576093, 10.82499999726882578, -13.76444248337722875 ) ) ;
#17465 = CARTESIAN_POINT ( 'NONE',  ( 6.486482029760649416E-15, 23.87500000273117706, 35.31076352940723240 ) ) ;
#17466 = CARTESIAN_POINT ( 'NONE',  ( -20.08610463437157989, 22.20000000546238184, -27.64615127144129758 ) ) ;
#17467 = CARTESIAN_POINT ( 'NONE',  ( 32.50000000000000000, 69.09999999999998010, -10.55989012756945833 ) ) ;
#17468 = CARTESIAN_POINT ( 'NONE',  ( 5.779280353836490358E-15, 47.00000000546238255, 32.49999999999999289 ) ) ;
#17469 = CARTESIAN_POINT ( 'NONE',  ( -14.73595198987283972, 73.99999999999997158, 2.369153449599709305 ) ) ;
#17470 = CARTESIAN_POINT ( 'NONE',  ( -26.00068869287368756, 15.29427083333332504, -15.01150461594595775 ) ) ;
#17471 = CARTESIAN_POINT ( 'NONE',  ( 6.486482029760649416E-15, 35.87500000273118417, 35.31076352940723240 ) ) ;
#17472 = CARTESIAN_POINT ( 'NONE',  ( -26.29305231718578995, 32.70000000546238539, 19.10302069950538595 ) ) ;
#17473 = CARTESIAN_POINT ( 'NONE',  ( 28.01184896238290278, 33.77083333333333570, -7.505752307973347470 ) ) ;
#17474 = CARTESIAN_POINT ( 'NONE',  ( 23.41746825000000243, 15.02499999726881086, 7.608796670333735079 ) ) ;
#17475 = CARTESIAN_POINT ( 'NONE',  ( -26.29305231718579350, 15.79999999999998117, -19.10302069950537884 ) ) ;
#17476 = CARTESIAN_POINT ( 'NONE',  ( -32.50000000000000000, 52.10000000000001563, 10.55989012756946366 ) ) ;
#17477 = CARTESIAN_POINT ( 'NONE',  ( -7.025853678916861966, 45.22357666574267654, -26.06988505166722803 ) ) ;
#17478 = CARTESIAN_POINT ( 'NONE',  ( -33.58253175000000113, 59.02500000273120406, -10.91162601494193218 ) ) ;
#17479 = CARTESIAN_POINT ( 'NONE',  ( -33.58253175000000113, 59.37500000273119838, 0.000000000000000000 ) ) ;
#17480 = CARTESIAN_POINT ( 'NONE',  ( -33.58253175000000113, 49.27500000273118985, -10.91162601494193041 ) ) ;
#17481 = CARTESIAN_POINT ( 'NONE',  ( -23.41746825000000243, 15.72499999726882081, 7.608796670333725309 ) ) ;
#17482 = CARTESIAN_POINT ( 'NONE',  ( 5.779280353836490358E-15, 37.00000000546237544, 32.49999999999999289 ) ) ;
#17483 = CARTESIAN_POINT ( 'NONE',  ( -32.50000000000000000, 6.000000000000005329, 0.000000000000000000 ) ) ;
#17484 = CARTESIAN_POINT ( 'NONE',  ( 19.11951029504763611, 45.23475666759063785, -19.06425588902591173 ) ) ;
#17485 = CARTESIAN_POINT ( 'NONE',  ( -23.40419987650453848, 16.99999999999998579, -6.773127805312867622 ) ) ;
#17486 = CARTESIAN_POINT ( 'NONE',  ( 7.570916362186207671, 3.599999999999992095, 23.30088464923126779 ) ) ;
#17487 = CARTESIAN_POINT ( 'NONE',  ( 20.75514604977248467, 22.42500000273119909, -28.56700777964554305 ) ) ;
#17488 = CARTESIAN_POINT ( 'NONE',  ( 5.779280353836490358E-15, 66.49999999999998579, 32.49999999999999289 ) ) ;
#17489 = CARTESIAN_POINT ( 'NONE',  ( 5.147494310547434893, 55.05125428700922896, 32.49999999999999289 ) ) ;
#17490 = CARTESIAN_POINT ( 'NONE',  ( -26.29305231718579350, 78.30000000546239391, -19.10302069950537884 ) ) ;
#17491 = CARTESIAN_POINT ( 'NONE',  ( -28.00173670424535644, 61.55170166574269786, 7.543491769121936308 ) ) ;
#17492 = CARTESIAN_POINT ( 'NONE',  ( 32.50000000000000000, 41.50000000546237544, -3.980102097228898626E-15 ) ) ;
#17493 = CARTESIAN_POINT ( 'NONE',  ( -32.50000000000000000, 60.60000000546239107, 10.55989012756946366 ) ) ;
#17494 = CARTESIAN_POINT ( 'NONE',  ( -27.16883889988624290, 34.92500000273118843, -19.73931689729374028 ) ) ;
#17495 = CARTESIAN_POINT ( 'NONE',  ( -19.09188309203694445, 39.49999999999999289, -19.09188309203661049 ) ) ;
#17496 = VERTEX_POINT ( 'NONE', #14356 ) ;
#17497 = CARTESIAN_POINT ( 'NONE',  ( 20.75514604977249178, 71.82500000273118701, 28.56700777964553950 ) ) ;
#17498 = CARTESIAN_POINT ( 'NONE',  ( -28.01184896238290278, 35.48958333333332860, 7.505752307973363457 ) ) ;
#17499 = CARTESIAN_POINT ( 'NONE',  ( -20.08610463437157989, 16.20000000546236762, -27.64615127144129758 ) ) ;
#17500 = ORIENTED_EDGE ( 'NONE', *, *, #9880, .T. ) ;
#17501 = CARTESIAN_POINT ( 'NONE',  ( 14.97647472619947351, 56.54986083425731636, 26.02091320914850314 ) ) ;
#17502 = CARTESIAN_POINT ( 'NONE',  ( 6.950374756619721595, 63.56809000092398065, 26.09010956794232428 ) ) ;
#17503 = CARTESIAN_POINT ( 'NONE',  ( 20.75514604977248467, 14.42500000273119021, -28.56700777964554305 ) ) ;
#17504 = CARTESIAN_POINT ( 'NONE',  ( 25.98046417659831775, 18.43972249907602290, -15.04653450569338879 ) ) ;
#17505 = CARTESIAN_POINT ( 'NONE',  ( -20.08610463437156923, 46.29999999999999716, 27.64615127144130113 ) ) ;
#17506 = CARTESIAN_POINT ( 'NONE',  ( 27.16883889988623935, 38.57500000273117280, -19.73931689729374384 ) ) ;
#17507 = CARTESIAN_POINT ( 'NONE',  ( -32.50000000000000000, 46.60000000546237686, 10.55989012756946366 ) ) ;
#17508 = EDGE_CURVE ( 'NONE', #31882, #684, #7870, .T. ) ;
#17509 = CARTESIAN_POINT ( 'NONE',  ( -15.00000000000000000, 73.90000000000000568, -4.873795443493594171 ) ) ;
#17510 = CARTESIAN_POINT ( 'NONE',  ( 10.37757302488624767, 29.72500000273120691, 31.93888565452638417 ) ) ;
#17511 = CARTESIAN_POINT ( 'NONE',  ( 3.880418787951172011, 13.30125427608447097, 24.49999999999998579 ) ) ;
#17512 = CARTESIAN_POINT ( 'NONE',  ( -27.16883889988624290, 57.17500000273118133, -19.73931689729374028 ) ) ;
#17513 = CARTESIAN_POINT ( 'NONE',  ( 26.29305231718579350, 30.80000000000000782, 19.10302069950537529 ) ) ;
#17514 = CARTESIAN_POINT ( 'NONE',  ( -10.04305231718578462, 34.39999999999998437, 30.90933677959249337 ) ) ;
#17515 = CARTESIAN_POINT ( 'NONE',  ( -4.523095164977116484E-15, 16.12499999726880873, 24.62258325217400312 ) ) ;
#17516 = CARTESIAN_POINT ( 'NONE',  ( 6.486482029760649416E-15, 77.62500000273121259, 35.31076352940723240 ) ) ;
#17517 = CARTESIAN_POINT ( 'NONE',  ( -16.81447360525995194, 66.99999999999995737, 28.18961368868553663 ) ) ;
#17518 = CARTESIAN_POINT ( 'NONE',  ( 8.959971004064378519, 74.08848768517671601, 11.34546913621253950 ) ) ;
#17519 = CARTESIAN_POINT ( 'NONE',  ( 20.75514604977249178, 66.07500000273118701, 28.56700777964553950 ) ) ;
#17520 = CARTESIAN_POINT ( 'NONE',  ( 15.00000000000000000, 77.25000000546239676, -1.836970198721029589E-15 ) ) ;
#17521 = ORIENTED_EDGE ( 'NONE', *, *, #32906, .T. ) ;
#17522 = CARTESIAN_POINT ( 'NONE',  ( -20.75514604977248823, 20.82500000273119412, -28.56700777964554305 ) ) ;
#17523 = PRODUCT_DEFINITION_SHAPE ( 'NONE', 'NONE',  #33996 ) ;
#17524 = CARTESIAN_POINT ( 'NONE',  ( -15.14183272437242600, 11.04999999453761284, 20.84094480462497856 ) ) ;
#17525 = CARTESIAN_POINT ( 'NONE',  ( -26.09010956794232428, 19.73996500092397355, 6.950374756619732253 ) ) ;
#17526 = CARTESIAN_POINT ( 'NONE',  ( 33.58253175000000823, 42.02500000273118985, 10.91162601494192863 ) ) ;
#17527 = CARTESIAN_POINT ( 'NONE',  ( -20.75514604977248823, 5.075000002731193227, -28.56700777964554305 ) ) ;
#17528 = CARTESIAN_POINT ( 'NONE',  ( 27.16883889988624290, 58.17500000273119554, 19.73931689729373673 ) ) ;
#17529 = CARTESIAN_POINT ( 'NONE',  ( -0.04044903254990864921, 46.52381916759065206, 30.02300923189239867 ) ) ;
#17530 = CARTESIAN_POINT ( 'NONE',  ( -4.300734207923759378, 80.47500000273116427, -13.23629886949340495 ) ) ;
#17531 = CARTESIAN_POINT ( 'NONE',  ( -20.47846945139866648, 37.20274333240935505, 20.53372385742108008 ) ) ;
#17532 = CARTESIAN_POINT ( 'NONE',  ( -10.04305231718579172, 62.10000000546238397, -30.90933677959248982 ) ) ;
#17533 = CARTESIAN_POINT ( 'NONE',  ( 11.25946833292375793, 74.07500000273120122, -8.180482586598735395 ) ) ;
#17534 = CARTESIAN_POINT ( 'NONE',  ( -26.09010956794245217, 65.27565999907601224, -6.950374756619243755 ) ) ;
#17535 = CARTESIAN_POINT ( 'NONE',  ( -5.147494310547322094, 57.55125428154683931, -32.50000000000003553 ) ) ;
#17536 = EDGE_CURVE ( 'NONE', #13996, #24889, #3883, .T. ) ;
#17537 = CARTESIAN_POINT ( 'NONE',  ( 6.277390505771533514E-15, 73.00000000546239676, 34.17252228774368916 ) ) ;
#17538 = CARTESIAN_POINT ( 'NONE',  ( -23.09401076758502924, 96.00000000000002842, 5.354274672883389237E-15 ) ) ;
#17539 = CARTESIAN_POINT ( 'NONE',  ( 33.58253175000000113, 40.37500000273118417, -4.112674001490185761E-15 ) ) ;
#17540 = CARTESIAN_POINT ( 'NONE',  ( 7.236395654485755280, 10.72499999726880837, 22.27133577429736988 ) ) ;
#17541 = ORIENTED_EDGE ( 'NONE', *, *, #17881, .T. ) ;
#17542 = CARTESIAN_POINT ( 'NONE',  ( 33.58253175000000823, 76.27500000273118985, 10.91162601494192863 ) ) ;
#17543 = CARTESIAN_POINT ( 'NONE',  ( 32.50000000000000711, 25.40000000546236691, 10.55989012756945122 ) ) ;
#17544 = ORIENTED_EDGE ( 'NONE', *, *, #30831, .F. ) ;
#17545 = EDGE_CURVE ( 'NONE', #28806, #8605, #30121, .T. ) ;
#17546 = CARTESIAN_POINT ( 'NONE',  ( 15.01150461594596308, 43.65364583333332860, -26.00068869287367335 ) ) ;
#17547 = CARTESIAN_POINT ( 'NONE',  ( 26.29305231718579350, 63.30000000546237260, 19.10302069950537529 ) ) ;
#17548 = ORIENTED_EDGE ( 'NONE', *, *, #31693, .T. ) ;
#17549 = CARTESIAN_POINT ( 'NONE',  ( 5.779280353836490358E-15, 56.49999999999998579, 32.49999999999999289 ) ) ;
#17550 = CARTESIAN_POINT ( 'NONE',  ( 10.37757302488624056, 50.52500000273118985, -31.93888565452638417 ) ) ;
#17551 = CARTESIAN_POINT ( 'NONE',  ( 20.08610463437157279, 55.80000000546236549, -27.64615127144129758 ) ) ;
#17552 = CARTESIAN_POINT ( 'NONE',  ( 20.08610463437157279, 7.800000005462373487, -27.64615127144129758 ) ) ;
#17553 = EDGE_CURVE ( 'NONE', #15317, #24251, #14887, .T. ) ;
#17554 = CARTESIAN_POINT ( 'NONE',  ( -12.13525491562421088, 77.80000000000001137, -8.816778784387096835 ) ) ;
#17555 = CYLINDRICAL_SURFACE ( 'NONE', #3460, 32.50000000000000000 ) ;
#17556 = CARTESIAN_POINT ( 'NONE',  ( -2.092463501923844636E-15, 51.50000000000000711, -34.17252228774368916 ) ) ;
#17557 = FACE_OUTER_BOUND ( 'NONE', #8004, .T. ) ;
#17558 = CARTESIAN_POINT ( 'NONE',  ( 20.75514604977248467, 18.67500000273120264, -28.56700777964554305 ) ) ;
#17559 = CARTESIAN_POINT ( 'NONE',  ( -32.50000000000000000, 73.90000000000001990, -10.55989012756945300 ) ) ;
#17560 = CARTESIAN_POINT ( 'NONE',  ( -7.025853678916861966, 28.03607666574268364, -26.06988505166722803 ) ) ;
#17561 = CARTESIAN_POINT ( 'NONE',  ( 8.601468415847520532, 78.07500000273117280, 11.83890561707634781 ) ) ;
#17562 = CARTESIAN_POINT ( 'NONE',  ( -10.04305231718578462, 56.39999999999999147, 30.90933677959249337 ) ) ;
#17563 = CARTESIAN_POINT ( 'NONE',  ( 16.87750156402159618, 52.00000000000001421, 29.11635311643962964 ) ) ;
#17564 = CARTESIAN_POINT ( 'NONE',  ( -33.58253175000000113, 79.27500000273118985, -10.91162601494193218 ) ) ;
#17565 = VERTEX_POINT ( 'NONE', #1291 ) ;
#17566 = CARTESIAN_POINT ( 'NONE',  ( -18.94512977948576093, 16.32499999726880091, 13.76444248337722698 ) ) ;
#17567 = CARTESIAN_POINT ( 'NONE',  ( 20.08610463437157279, 71.80000000546239391, -27.64615127144129758 ) ) ;
#17568 = CARTESIAN_POINT ( 'NONE',  ( 24.20753774853756113, 54.82552083333331439, 13.97622843553589789 ) ) ;
#17569 = CARTESIAN_POINT ( 'NONE',  ( 27.16883889988624290, 57.92500000273119554, 19.73931689729373673 ) ) ;
#17570 = CARTESIAN_POINT ( 'NONE',  ( -33.58253175000000113, 23.37500000273119838, 0.000000000000000000 ) ) ;
#17571 = CARTESIAN_POINT ( 'NONE',  ( 20.75514604977248467, 8.675000002731195536, -28.56700777964554305 ) ) ;
#17572 = CARTESIAN_POINT ( 'NONE',  ( -33.58253175000000113, 3.275000002731191628, -10.91162601494193041 ) ) ;
#17573 = CARTESIAN_POINT ( 'NONE',  ( 28.02196122052045268, 21.45871500092397355, -7.468012846824774620 ) ) ;
#17574 = CARTESIAN_POINT ( 'NONE',  ( 2.740863092043355209E-13, 62.27343749999999289, 30.02300923189239512 ) ) ;
#17575 = CARTESIAN_POINT ( 'NONE',  ( -33.58253175000000113, 5.125000002731180615, 0.000000000000000000 ) ) ;
#17576 = CARTESIAN_POINT ( 'NONE',  ( 10.04305231718578817, 3.400000000000014122, -30.90933677959249337 ) ) ;
#17577 = CARTESIAN_POINT ( 'NONE',  ( 10.04305231718578817, 43.40000000000000568, -30.90933677959249337 ) ) ;
#17578 = CARTESIAN_POINT ( 'NONE',  ( -10.37757302488624411, 42.72500000273119269, -31.93888565452638417 ) ) ;
#17579 = CARTESIAN_POINT ( 'NONE',  ( -14.47279130897151589, 3.324999997268803131, -19.92008829642072598 ) ) ;
#17580 = CARTESIAN_POINT ( 'NONE',  ( 13.97622843553633842, 65.42447916666665719, 24.20753774853730889 ) ) ;
#17581 = EDGE_LOOP ( 'NONE', ( #29584, #3237, #20412, #3134, #20460, #26961, #20327, #29409 ) ) ;
#17582 = CARTESIAN_POINT ( 'NONE',  ( 27.16883889988623935, 60.57500000273117990, -19.73931689729374384 ) ) ;
#17583 = CARTESIAN_POINT ( 'NONE',  ( 32.50000000000000000, 42.99999999999998579, -3.980102097228898626E-15 ) ) ;
#17584 = CARTESIAN_POINT ( 'NONE',  ( -18.94512977948575738, 13.42499999726881654, -13.76444248337723231 ) ) ;
#17585 = CARTESIAN_POINT ( 'NONE',  ( -26.06988505166735237, 37.21392333425730214, -7.025853678916388567 ) ) ;
#17586 = ORIENTED_EDGE ( 'NONE', *, *, #6380, .T. ) ;
#17587 = CARTESIAN_POINT ( 'NONE',  ( 10.37757302488624056, 30.52500000273118630, -31.93888565452638417 ) ) ;
#17588 = ORIENTED_EDGE ( 'NONE', *, *, #9209, .T. ) ;
#17589 = DIRECTION ( 'NONE',  ( -1.000000000000000000, -1.416100796715760863E-16, 0.000000000000000000 ) ) ;
#17590 = CARTESIAN_POINT ( 'NONE',  ( 33.58253175000000113, 66.12500000273119838, -4.112674001490185761E-15 ) ) ;
#17591 = CARTESIAN_POINT ( 'NONE',  ( 30.02300923189239512, 40.78906249999998579, -2.619432448724977703E-13 ) ) ;
#17592 = CARTESIAN_POINT ( 'NONE',  ( -24.50000000000000000, 13.00000000000001066, -3.000384657911015469E-15 ) ) ;
#17593 = CARTESIAN_POINT ( 'NONE',  ( 23.41746824999999887, 3.224999997268806151, -7.608796670333727974 ) ) ;
#17594 = CARTESIAN_POINT ( 'NONE',  ( -27.16883889988623935, 9.325000002731176352, 19.73931689729374739 ) ) ;
#17595 = CARTESIAN_POINT ( 'NONE',  ( -15.14183272437242067, 6.449999994537612302, -20.84094480462497856 ) ) ;
#17596 = CARTESIAN_POINT ( 'NONE',  ( -15.04653450569338524, 48.51784749907601935, -25.98046417659831775 ) ) ;
#17597 = CARTESIAN_POINT ( 'NONE',  ( -4.635254915624211769, 73.59999999999999432, -14.26584774442730286 ) ) ;
#17598 = CARTESIAN_POINT ( 'NONE',  ( 28.01184896238304134, 61.55729166666666430, 7.505752307972846538 ) ) ;
#17599 = CARTESIAN_POINT ( 'NONE',  ( 32.50000000000000000, 19.50000000546236834, -3.980102097228898626E-15 ) ) ;
#17600 = CARTESIAN_POINT ( 'NONE',  ( -9.270509831248423538, 73.95000000546238539, -12.75976212528059861 ) ) ;
#17601 = CARTESIAN_POINT ( 'NONE',  ( 19.82091636218621034, 13.54999999453762527, 14.40073868116559730 ) ) ;
#17602 = CARTESIAN_POINT ( 'NONE',  ( -12.13525491562420910, 76.45000000546237118, 8.816778784387098611 ) ) ;
#17603 = CARTESIAN_POINT ( 'NONE',  ( -2.428612866367529427E-13, 22.74218749999999645, -27.95245687107222921 ) ) ;
#17604 = CARTESIAN_POINT ( 'NONE',  ( 20.75514604977249178, 31.82500000273119056, 28.56700777964553950 ) ) ;
#17605 = AXIS2_PLACEMENT_3D ( 'NONE', #5947, #23977, #29106 ) ;
#17606 = CARTESIAN_POINT ( 'NONE',  ( 20.75514604977249178, 46.07500000273117280, 28.56700777964553950 ) ) ;
#17607 = CARTESIAN_POINT ( 'NONE',  ( 33.58253175000000113, 20.37500000273118062, -4.112674001490185761E-15 ) ) ;
#17608 = LINE ( 'NONE', #17267, #2411 ) ;
#17609 = CARTESIAN_POINT ( 'NONE',  ( -1.778240108872766143E-15, 8.000000005462370112, -32.49999999999999289 ) ) ;
#17610 = CARTESIAN_POINT ( 'NONE',  ( 12.13525491562421088, 80.79999999999998295, 8.816778784387095058 ) ) ;
#17611 = CARTESIAN_POINT ( 'NONE',  ( 20.08610463437157279, 61.30000000000001847, -27.64615127144129758 ) ) ;
#17612 = CARTESIAN_POINT ( 'NONE',  ( -23.41746824999999887, 9.624999997268817609, -2.867812753649727150E-15 ) ) ;
#17613 = CARTESIAN_POINT ( 'NONE',  ( 6.486482029760648627E-15, 67.62500000273119838, 35.31076352940722529 ) ) ;
#17614 = CARTESIAN_POINT ( 'NONE',  ( -1.089172066684569321E-14, 78.49999999999998579, 15.00000000000000000 ) ) ;
#17615 = CARTESIAN_POINT ( 'NONE',  ( 6.950374756619257965, 35.19753499907601935, -26.09010956794244507 ) ) ;
#17616 = VECTOR ( 'NONE', #7068, 1000.000000000000000 ) ;
#17617 = CARTESIAN_POINT ( 'NONE',  ( -27.16883889988624290, 79.17500000273118133, -19.73931689729374028 ) ) ;
#17618 = CARTESIAN_POINT ( 'NONE',  ( 33.58253175000000113, 12.12500000273120193, -4.112674001490185761E-15 ) ) ;
#17619 = CARTESIAN_POINT ( 'NONE',  ( 23.41746825000000243, 13.02499999726881619, 7.608796670333735079 ) ) ;
#17620 = CARTESIAN_POINT ( 'NONE',  ( -13.97622843553588901, 65.99739583333334281, 24.20753774853756823 ) ) ;
#17621 = VERTEX_POINT ( 'NONE', #1466 ) ;
#17622 = CARTESIAN_POINT ( 'NONE',  ( 10.37757302488624767, 51.72500000273121401, 31.93888565452638417 ) ) ;
#17623 = CARTESIAN_POINT ( 'NONE',  ( -20.75514604977248823, 25.07500000273120122, -28.56700777964554305 ) ) ;
#17624 = ORIENTED_EDGE ( 'NONE', *, *, #29971, .F. ) ;
#17625 = CARTESIAN_POINT ( 'NONE',  ( 15.01150461594643204, 34.48697916666667140, 26.00068869287340334 ) ) ;
#17626 = CARTESIAN_POINT ( 'NONE',  ( 28.00173670424549499, 35.49517333425730214, 7.543491769121417612 ) ) ;
#17627 = CARTESIAN_POINT ( 'NONE',  ( 7.313012447739250820E-14, 15.50000000000000178, 24.50000000000000000 ) ) ;
#17628 = VECTOR ( 'NONE', #315, 1000.000000000000000 ) ;
#17629 = CARTESIAN_POINT ( 'NONE',  ( 12.11000150615021909, -45.00000000000000000, 1.483047458217648827E-15 ) ) ;
#17630 = CARTESIAN_POINT ( 'NONE',  ( 18.94512977948575738, 2.924999997268806773, 13.76444248337723408 ) ) ;
#17631 = CARTESIAN_POINT ( 'NONE',  ( -23.41746825000000243, 9.524999997268810858, -7.608796670333730638 ) ) ;
#17632 = CARTESIAN_POINT ( 'NONE',  ( -20.75514604977248823, 15.07500000273116747, -28.56700777964554305 ) ) ;
#17633 = CARTESIAN_POINT ( 'NONE',  ( 10.04305231718578817, 21.90000000546238468, -30.90933677959249337 ) ) ;
#17634 = EDGE_CURVE ( 'NONE', #20831, #7065, #18418, .T. ) ;
#17635 = CARTESIAN_POINT ( 'NONE',  ( -26.29305231718578995, 68.19999999999998863, 19.10302069950538595 ) ) ;
#17636 = PLANE ( 'NONE',  #27490 ) ;
#17637 = CARTESIAN_POINT ( 'NONE',  ( -14.28731510817884498, 73.99999999999998579, 4.080734695941037771 ) ) ;
#17638 = CARTESIAN_POINT ( 'NONE',  ( 28.00173670424549499, 62.99517333425730214, 7.543491769121417612 ) ) ;
#17639 = CARTESIAN_POINT ( 'NONE',  ( -33.58253175000000113, 31.27500000273118275, -10.91162601494193218 ) ) ;
#17640 = CARTESIAN_POINT ( 'NONE',  ( 11.25946833292375793, 80.17500000273119554, 8.180482586598731842 ) ) ;
#17641 = CARTESIAN_POINT ( 'NONE',  ( -20.50609665440969209, 28.32812499999999645, 20.50609665441005092 ) ) ;
#17642 = ADVANCED_FACE ( 'NONE', ( #15560 ), #26013, .F. ) ;
#17643 = CARTESIAN_POINT ( 'NONE',  ( -15.14183272437242067, 0.7000000000000070610, -20.84094480462497856 ) ) ;
#17644 = CARTESIAN_POINT ( 'NONE',  ( -10.04305231718579172, 7.599999999999996092, -30.90933677959248982 ) ) ;
#17645 = CARTESIAN_POINT ( 'NONE',  ( -19.82091636218621034, 16.80000000000000782, -14.40073868116559552 ) ) ;
#17646 = CARTESIAN_POINT ( 'NONE',  ( 0.04044903255044120238, 50.52305583240934794, 27.95245687107223276 ) ) ;
#17647 = CARTESIAN_POINT ( 'NONE',  ( 20.75514604977248467, 56.42500000273120264, -28.56700777964554305 ) ) ;
#17648 = CARTESIAN_POINT ( 'NONE',  ( -2.162160676586881955E-15, 64.87500000273119838, -35.31076352940723240 ) ) ;
#17649 = CARTESIAN_POINT ( 'NONE',  ( 27.16883889988623935, 38.57500000273117280, -19.73931689729374384 ) ) ;
#17650 = CARTESIAN_POINT ( 'NONE',  ( -4.523095164977117273E-15, 14.12499999726881050, 24.62258325217400312 ) ) ;
#17651 = CARTESIAN_POINT ( 'NONE',  ( 15.14183272437242067, 9.700000000000013500, 20.84094480462498211 ) ) ;
#17652 = CARTESIAN_POINT ( 'NONE',  ( 40.00000000000000000, 52.00000000000000711, -23.09401076758505766 ) ) ;
#17653 = CARTESIAN_POINT ( 'NONE',  ( -19.82091636218621034, 4.549999994537618164, -14.40073868116559552 ) ) ;
#17654 = CARTESIAN_POINT ( 'NONE',  ( 4.159479030958464888E-15, -56.96472381958990638, 0.000000000000000000 ) ) ;
#17655 = CARTESIAN_POINT ( 'NONE',  ( -20.75514604977248112, 21.42500000273120264, 28.56700777964554661 ) ) ;
#17656 = DIRECTION ( 'NONE',  ( 0.000000000000000000, -0.000000000000000000, 1.000000000000000000 ) ) ;
#17657 = PLANE ( 'NONE',  #5696 ) ;
#17658 = LINE ( 'NONE', #25030, #17126 ) ;
#17659 = CARTESIAN_POINT ( 'NONE',  ( -28.00173670424535644, 64.98920166574268364, 7.543491769121936308 ) ) ;
#17660 = CARTESIAN_POINT ( 'NONE',  ( 20.08610463437157279, 41.80000000546237260, -27.64615127144129758 ) ) ;
#17661 = CARTESIAN_POINT ( 'NONE',  ( -1.778240108872766143E-15, 35.49999999999998579, -32.49999999999999289 ) ) ;
#17662 = CARTESIAN_POINT ( 'NONE',  ( 10.37757302488624767, 29.72500000273120691, 31.93888565452638417 ) ) ;
#17663 = CARTESIAN_POINT ( 'NONE',  ( -27.95245687107222921, 32.19531250000000000, 2.498001805406602216E-13 ) ) ;
#17664 = ORIENTED_EDGE ( 'NONE', *, *, #10417, .T. ) ;
#17665 = EDGE_LOOP ( 'NONE', ( #18859, #23929, #1477, #2988 ) ) ;
#17666 = CARTESIAN_POINT ( 'NONE',  ( -10.37757302488623701, 69.52500000273118985, 31.93888565452638417 ) ) ;
#17667 = CARTESIAN_POINT ( 'NONE',  ( -7.505752307972844761, 41.79166666666666430, 28.01184896238304134 ) ) ;
#17668 = CARTESIAN_POINT ( 'NONE',  ( -5.147494310547430452, 16.05125428700922541, -32.49999999999999289 ) ) ;
#17669 = ORIENTED_EDGE ( 'NONE', *, *, #33593, .F. ) ;
#17670 = CARTESIAN_POINT ( 'NONE',  ( -20.53372385742071771, 57.26600666759063785, 20.47846945139902530 ) ) ;
#17671 = CARTESIAN_POINT ( 'NONE',  ( 24.18731323226247554, 63.13840250092397355, 14.01125832528285997 ) ) ;
#17672 = CIRCLE ( 'NONE', #9442, 13.32050807568876927 ) ;
#17673 = CARTESIAN_POINT ( 'NONE',  ( 20.75514604977249178, 11.82500000273118346, 28.56700777964553950 ) ) ;
#17674 = CARTESIAN_POINT ( 'NONE',  ( -30.02300923189239867, 17.00743083240935860, 0.04044903255044988294 ) ) ;
#17675 = LINE ( 'NONE', #4793, #15768 ) ;
#17676 = CARTESIAN_POINT ( 'NONE',  ( 27.16883889988624290, 42.17500000273119554, 19.73931689729373673 ) ) ;
#17677 = CARTESIAN_POINT ( 'NONE',  ( -26.29305231718579350, 44.30000000546238681, -19.10302069950537884 ) ) ;
#17678 = CARTESIAN_POINT ( 'NONE',  ( 4.635254915624209993, 77.39999999999996305, -14.26584774442730463 ) ) ;
#17679 = CARTESIAN_POINT ( 'NONE',  ( 20.75514604977249178, 19.82500000273119412, 28.56700777964553950 ) ) ;
#17680 = CARTESIAN_POINT ( 'NONE',  ( 24.50000000000000000, 13.74999999453763166, 0.000000000000000000 ) ) ;
#17681 = CARTESIAN_POINT ( 'NONE',  ( 10.37757302488624767, 53.97500000273119980, 31.93888565452638417 ) ) ;
#17682 =( LENGTH_UNIT ( ) NAMED_UNIT ( * ) SI_UNIT ( .MILLI., .METRE. ) );
#17683 = ADVANCED_FACE ( 'NONE', ( #15898 ), #18135, .T. ) ;
#17684 = CARTESIAN_POINT ( 'NONE',  ( 20.08610463437158344, 30.69999999999999218, 27.64615127144129403 ) ) ;
#17685 = ADVANCED_FACE ( 'NONE', ( #12973 ), #2843, .T. ) ;
#17686 = CARTESIAN_POINT ( 'NONE',  ( -10.04305231718578462, 28.40000000000000924, 30.90933677959249337 ) ) ;
#17687 = CARTESIAN_POINT ( 'NONE',  ( -23.41746825000000598, 17.72499999726881725, 7.608796670333726198 ) ) ;
#17688 = CARTESIAN_POINT ( 'NONE',  ( -2.162160676586881955E-15, 76.62500000273118417, -35.31076352940723240 ) ) ;
#17689 = CARTESIAN_POINT ( 'NONE',  ( -8.761981113183991350E-16, -15.84529946162075298, 0.000000000000000000 ) ) ;
#17690 = CARTESIAN_POINT ( 'NONE',  ( 5.779280353836490358E-15, 21.00000000546237544, 32.49999999999999289 ) ) ;
#17691 = CARTESIAN_POINT ( 'NONE',  ( 33.58253175000000823, 60.27500000273116143, 10.91162601494192685 ) ) ;
#17692 = CARTESIAN_POINT ( 'NONE',  ( -12.13525491562420910, 76.45000000546237118, 8.816778784387098611 ) ) ;
#17693 = ORIENTED_EDGE ( 'NONE', *, *, #33051, .F. ) ;
#17694 = CARTESIAN_POINT ( 'NONE',  ( -20.75514604977248112, 21.42500000273120264, 28.56700777964554661 ) ) ;
#17695 = CARTESIAN_POINT ( 'NONE',  ( -7.570916362186210335, 8.349999994537615322, -23.30088464923126779 ) ) ;
#17696 = CARTESIAN_POINT ( 'NONE',  ( 24.18731323226247554, 18.45090250092397355, 14.01125832528285997 ) ) ;
#17697 = AXIS2_PLACEMENT_3D ( 'NONE', #16977, #119, #10275 ) ;
#17698 = CARTESIAN_POINT ( 'NONE',  ( -33.58253175000000113, 39.02500000273118985, -10.91162601494193218 ) ) ;
#17699 = CARTESIAN_POINT ( 'NONE',  ( -27.16883889988624290, 5.175000002731189319, -19.73931689729374028 ) ) ;
#17700 = CARTESIAN_POINT ( 'NONE',  ( 20.75514604977248467, 54.67500000273119554, -28.56700777964554305 ) ) ;
#17701 = CARTESIAN_POINT ( 'NONE',  ( 14.97647472619947351, 46.23736083425730925, 26.02091320914850314 ) ) ;
#17702 = EDGE_CURVE ( 'NONE', #24433, #31338, #25413, .T. ) ;
#17703 = CARTESIAN_POINT ( 'NONE',  ( 3.880418787951140036, 6.448745718453147369, -24.49999999999999645 ) ) ;
#17704 = CARTESIAN_POINT ( 'NONE',  ( -25.98046417659831420, 40.78347249907601935, 15.04653450569339945 ) ) ;
#17705 = CARTESIAN_POINT ( 'NONE',  ( 26.29305231718578995, 59.70000000546237118, -19.10302069950538240 ) ) ;
#17706 = CARTESIAN_POINT ( 'NONE',  ( 13.91746825000000065, 73.77500000273116143, 4.522059556121114987 ) ) ;
#17707 =( BOUNDED_CURVE ( )  B_SPLINE_CURVE ( 2, ( #23496, #13362, #5124, #10109, #15611, #31206, #2556, #23325, #23836, #33954, #12675, #10447, #23664 ),
 .UNSPECIFIED., .F., .T. ) 
 B_SPLINE_CURVE_WITH_KNOTS ( ( 3, 2, 2, 2, 2, 2, 3 ),
 ( 0.4722222222222222099, 0.4777777777777778012, 0.4888888888888888729, 0.5000000000000000000, 0.5111111111111110716, 0.5222222222222222543, 0.5277777777777777901 ),
 .UNSPECIFIED. ) 
 CURVE ( )  GEOMETRIC_REPRESENTATION_ITEM ( )  RATIONAL_B_SPLINE_CURVE ( ( 0.9755282581475765991, 0.9755282581475765991, 1.000000000000000000, 0.9510565162951535312, 1.000000000000000000, 0.9510565162951535312, 1.000000000000000000, 0.9510565162951535312, 1.000000000000000000, 0.9510565162951535312, 1.000000000000000000, 0.9755282581475768211, 0.9755282581475768211 ) ) 
 REPRESENTATION_ITEM ( '' )  );
#17708 = CARTESIAN_POINT ( 'NONE',  ( -24.22776226481266448, 65.41888916574268364, -13.94119854578892514 ) ) ;
#17709 = CARTESIAN_POINT ( 'NONE',  ( 26.29305231718578995, 63.70000000546238539, -19.10302069950538240 ) ) ;
#17710 = CARTESIAN_POINT ( 'NONE',  ( -20.08610463437157989, 74.20000000546238539, -27.64615127144129758 ) ) ;
#17711 = CARTESIAN_POINT ( 'NONE',  ( 15.01150461594596308, 16.15364583333333215, -26.00068869287367335 ) ) ;
#17712 = CARTESIAN_POINT ( 'NONE',  ( -2.162160676586881955E-15, 32.87500000273118417, -35.31076352940723240 ) ) ;
#17713 = CARTESIAN_POINT ( 'NONE',  ( 23.41746824999999887, 7.224999997268826135, -7.608796670333727974 ) ) ;
#17714 = EDGE_LOOP ( 'NONE', ( #30935, #216, #6175, #21060 ) ) ;
#17715 = CARTESIAN_POINT ( 'NONE',  ( -10.37757302488623701, 75.77500000273118985, 31.93888565452638417 ) ) ;
#17716 = CARTESIAN_POINT ( 'NONE',  ( 32.50000000000000000, 25.50000000546236123, -3.980102097228898626E-15 ) ) ;
#17717 = CARTESIAN_POINT ( 'NONE',  ( -15.01150461594642138, 39.64322916666667140, -26.00068869287340334 ) ) ;
#17718 = CARTESIAN_POINT ( 'NONE',  ( 20.08610463437157279, 61.80000000546237970, -27.64615127144129758 ) ) ;
#17719 = ORIENTED_EDGE ( 'NONE', *, *, #17836, .F. ) ;
#17720 = AXIS2_PLACEMENT_3D ( 'NONE', #5446, #18837, #20904 ) ;
#17721 = CARTESIAN_POINT ( 'NONE',  ( -5.147494310547423346, 10.94874572391553436, 32.50000000000000000 ) ) ;
#17722 = CARTESIAN_POINT ( 'NONE',  ( 27.16883889988623935, 46.32500000273117990, -19.73931689729374384 ) ) ;
#17723 = CARTESIAN_POINT ( 'NONE',  ( 23.41746825000000243, 18.52499999726881441, 7.608796670333735079 ) ) ;
#17724 = CARTESIAN_POINT ( 'NONE',  ( -20.08610463437157989, 8.200000005462390718, -27.64615127144129758 ) ) ;
#17725 = AXIS2_PLACEMENT_3D ( 'NONE', #15575, #18149, #15223 ) ;
#17726 = CARTESIAN_POINT ( 'NONE',  ( -20.08610463437157989, 7.699999999999988631, -27.64615127144129758 ) ) ;
#17727 = CARTESIAN_POINT ( 'NONE',  ( 26.00068869287341045, 16.44010416666666430, -15.01150461594642493 ) ) ;
#17728 = CARTESIAN_POINT ( 'NONE',  ( -32.50000000000000000, 54.10000000000000853, 10.55989012756946366 ) ) ;
#17729 = CARTESIAN_POINT ( 'NONE',  ( 12.11607355459420710, -70.99969134886156041, 1.483791069686768383E-15 ) ) ;
#17730 = CARTESIAN_POINT ( 'NONE',  ( -33.58253175000000113, 19.47500000273117493, 10.91162601494193929 ) ) ;
#17731 = CARTESIAN_POINT ( 'NONE',  ( -26.29305231718579350, 24.30000000546236905, -19.10302069950537884 ) ) ;
#17732 = CARTESIAN_POINT ( 'NONE',  ( -14.01125832528328985, 21.01784749907601579, -24.18731323226223040 ) ) ;
#17733 = CARTESIAN_POINT ( 'NONE',  ( 13.91746825000000065, 76.27500000273118985, 4.522059556121114987 ) ) ;
#17734 = CARTESIAN_POINT ( 'NONE',  ( 24.50000000000000000, 7.900000000000012790, 7.960532557706212486 ) ) ;
#17735 = CARTESIAN_POINT ( 'NONE',  ( 26.29305231718579350, 2.799999999999997158, 19.10302069950537529 ) ) ;
#17736 = ORIENTED_EDGE ( 'NONE', *, *, #31186, .F. ) ;
#17737 = CARTESIAN_POINT ( 'NONE',  ( -18.94512977948575738, 13.92499999726881654, -13.76444248337723231 ) ) ;
#17738 = CARTESIAN_POINT ( 'NONE',  ( 23.41746824999999887, 4.524999997268823293, 7.608796670333735079 ) ) ;
#17739 = CARTESIAN_POINT ( 'NONE',  ( -27.95245687107222921, 49.38281249999997868, 2.498001805406602216E-13 ) ) ;
#17740 = CARTESIAN_POINT ( 'NONE',  ( 27.16883889988623935, 60.32500000273120833, -19.73931689729374384 ) ) ;
#17741 = CARTESIAN_POINT ( 'NONE',  ( 20.75514604977248467, 22.67500000273119198, -28.56700777964554305 ) ) ;
#17742 = CARTESIAN_POINT ( 'NONE',  ( 10.37757302488624056, 8.775000002731166759, -31.93888565452638417 ) ) ;
#17743 = CARTESIAN_POINT ( 'NONE',  ( -27.95245687107223276, 28.75781249999999645, 2.498001805406602216E-13 ) ) ;
#17744 = CARTESIAN_POINT ( 'NONE',  ( -15.04653450569291984, 22.74777750092397355, 25.98046417659859486 ) ) ;
#17745 = CARTESIAN_POINT ( 'NONE',  ( 2.740863092043355209E-13, 58.83593750000000000, 30.02300923189239512 ) ) ;
#17746 = CARTESIAN_POINT ( 'NONE',  ( 6.277390505771533514E-15, 77.00000000546235412, 34.17252228774368916 ) ) ;
#17747 = CARTESIAN_POINT ( 'NONE',  ( -8.601468415847515203, 73.67500000273120975, 11.83890561707634959 ) ) ;
#17748 = CARTESIAN_POINT ( 'NONE',  ( -10.04305231718578462, 42.40000000000000568, 30.90933677959249337 ) ) ;
#17749 = CARTESIAN_POINT ( 'NONE',  ( 20.75514604977248467, 46.42500000273119554, -28.56700777964554305 ) ) ;
#17750 = AXIS2_PLACEMENT_3D ( 'NONE', #31029, #2374, #18009 ) ;
#17751 = CARTESIAN_POINT ( 'NONE',  ( -7.236395654485763274, 10.02499999726880198, 22.27133577429736633 ) ) ;
#17752 = CARTESIAN_POINT ( 'NONE',  ( 2.375766604868040144, 78.55125428154686062, 15.00000000000000178 ) ) ;
#17753 = ORIENTED_EDGE ( 'NONE', *, *, #4310, .F. ) ;
#17754 = CARTESIAN_POINT ( 'NONE',  ( 33.58253175000000823, 56.27500000273116854, 10.91162601494192863 ) ) ;
#17755 = CARTESIAN_POINT ( 'NONE',  ( 3.673940397442059178E-15, -10.99999999999999645, -30.00000000000000000 ) ) ;
#17756 = CARTESIAN_POINT ( 'NONE',  ( 0.04044903254993986036, 44.80506916759064495, -27.95245687107223986 ) ) ;
#17757 = CARTESIAN_POINT ( 'NONE',  ( 33.58253175000000823, 74.27500000273117564, 10.91162601494192863 ) ) ;
#17758 = VERTEX_POINT ( 'NONE', #12803 ) ;
#17759 = CARTESIAN_POINT ( 'NONE',  ( -27.16883889988624290, 28.92500000273119554, -19.73931689729374028 ) ) ;
#17760 = CARTESIAN_POINT ( 'NONE',  ( 15.01150461594643204, 17.29947916666666430, 26.00068869287340334 ) ) ;
#17761 = EDGE_LOOP ( 'NONE', ( #33796, #24378, #15145, #13500 ) ) ;
#17762 = CARTESIAN_POINT ( 'NONE',  ( 5.779280353836490358E-15, 58.49999999999999289, 32.49999999999999289 ) ) ;
#17763 = CARTESIAN_POINT ( 'NONE',  ( 10.37757302488624056, 70.52500000273120406, -31.93888565452638417 ) ) ;
#17764 = CARTESIAN_POINT ( 'NONE',  ( -26.00068869287340334, 35.34635416666666430, 15.01150461594643382 ) ) ;
#17765 = CARTESIAN_POINT ( 'NONE',  ( -24.50000000000000355, 10.90000000000000568, -7.960532557706207157 ) ) ;
#17766 = LINE ( 'NONE', #20520, #27021 ) ;
#17767 = EDGE_CURVE ( 'NONE', #28004, #24994, #20624, .T. ) ;
#17768 = CARTESIAN_POINT ( 'NONE',  ( -27.16883889988624290, 10.92500000273119376, -19.73931689729374028 ) ) ;
#17769 = CYLINDRICAL_SURFACE ( 'NONE', #3928, 27.00000000000000000 ) ;
#17770 = CARTESIAN_POINT ( 'NONE',  ( -28.00173670424535644, 51.23920166574269786, 7.543491769121936308 ) ) ;
#17771 = CARTESIAN_POINT ( 'NONE',  ( -12.13525491562420910, 76.19999999999998863, 8.816778784387098611 ) ) ;
#17772 = CLOSED_SHELL ( 'NONE', ( #7266, #19921, #24193, #23538, #10282, #29290, #12010, #11872, #27145, #3797, #22009, #31313, #21860, #16593, #20054, #3152, #26158, #6428, #18140, #14405, #29262, #15249, #18702, #22670, #15471, #32262, #6886, #1158, #15462, #33398, #11539, #17113, #7989, #19443, #13029, #5991, #20601, #13466, #21637, #5942, #22163, #33036, #12930, #26004, #14604, #10470, #10846, #20204, #23008, #28752, #16787, #27609, #31463, #12505, #1650, #28756, #25081, #15182, #19029, #20494, #10743, #27085, #19163, #10622, #31750, #19344, #19021, #32679, #23774, #33147, #28516, #14988, #319, #2241, #4129, #14075, #21961, #2957, #11460, #4115, #4220, #26624, #30637, #30300, #11864, #24062, #2443, #20158, #26568, #6630, #13881, #17685, #28797, #26010, #8825, #28940, #17982, #17683, #12406, #2964, #6740, #23919, #26148, #11453, #23163, #21633, #5960, #12655, #10836, #19222, #6928, #26286, #14817, #22621, #5944, #15015, #4328, #28330, #33862, #25951, #25812, #31074, #24156, #8365, #4182, #29168, #23624, #13980, #10427, #1585, #886, #31166, #3198, #20358, #11735 ) ) ;
#17773 = CARTESIAN_POINT ( 'NONE',  ( 15.00000000000000355, 80.90000000000000568, 4.873795443493592394 ) ) ;
#17774 = DIRECTION ( 'NONE',  ( -1.000000000000000000, -1.309225264888156377E-16, 0.000000000000000000 ) ) ;
#17775 = CARTESIAN_POINT ( 'NONE',  ( 5.147494310547434893, 61.05125428700922896, 32.49999999999999289 ) ) ;
#17776 = CARTESIAN_POINT ( 'NONE',  ( 24.50000000000000355, 15.84999999453763664, -7.960532557706203605 ) ) ;
#17777 = CARTESIAN_POINT ( 'NONE',  ( -4.635254915624211769, 79.85000000546239107, -14.26584774442730286 ) ) ;
#17778 = CARTESIAN_POINT ( 'NONE',  ( -6.988114217768288228, 22.59895833333332860, -26.07999730980477437 ) ) ;
#17779 = CARTESIAN_POINT ( 'NONE',  ( -27.16883889988624290, 32.92500000273118843, -19.73931689729374028 ) ) ;
#17780 = CARTESIAN_POINT ( 'NONE',  ( 15.00000000000000000, 75.00000000000001421, -1.836970198721029589E-15 ) ) ;
#17781 = CARTESIAN_POINT ( 'NONE',  ( -27.16883889988624290, 43.17500000273118133, -19.73931689729374028 ) ) ;
#17782 = CARTESIAN_POINT ( 'NONE',  ( 33.58253175000000823, 24.27500000273119696, 10.91162601494192685 ) ) ;
#17783 = CARTESIAN_POINT ( 'NONE',  ( -20.08610463437156923, 12.80000000546236016, 27.64615127144130113 ) ) ;
#17784 = CARTESIAN_POINT ( 'NONE',  ( 33.58253175000000113, 74.22500000273119269, -10.91162601494193574 ) ) ;
#17785 = CARTESIAN_POINT ( 'NONE',  ( 3.445340210940985210E-14, 7.499999999999994671, 24.50000000000000000 ) ) ;
#17786 = CARTESIAN_POINT ( 'NONE',  ( 26.29305231718578995, 63.20000000000001705, -19.10302069950538240 ) ) ;
#17787 = CARTESIAN_POINT ( 'NONE',  ( -18.94512977948575738, 15.42499999726881832, -13.76444248337723231 ) ) ;
#17788 = CARTESIAN_POINT ( 'NONE',  ( -20.75514604977248823, 66.82500000273118701, -28.56700777964554305 ) ) ;
#17789 = CARTESIAN_POINT ( 'NONE',  ( -18.94512977948576093, 4.324999997268818674, 13.76444248337722698 ) ) ;
#17790 = CARTESIAN_POINT ( 'NONE',  ( -24.18731323226221974, 47.65847249907603356, 14.01125832528330406 ) ) ;
#17791 = MECHANICAL_DESIGN_GEOMETRIC_PRESENTATION_REPRESENTATION (  '', ( #31478 ), #29820 ) ;
#17792 = CARTESIAN_POINT ( 'NONE',  ( 27.16883889988623935, 70.57500000273118701, -19.73931689729374384 ) ) ;
#17793 = CARTESIAN_POINT ( 'NONE',  ( -10.37757302488624411, 8.725000002731187365, -31.93888565452638417 ) ) ;
#17794 = CARTESIAN_POINT ( 'NONE',  ( -7.236395654485757944, 13.72499999726881015, -22.27133577429736988 ) ) ;
#17795 = CARTESIAN_POINT ( 'NONE',  ( 6.988114217768294445, 65.56770833333332860, 26.07999730980477437 ) ) ;
#17796 = VERTEX_POINT ( 'NONE', #28917 ) ;
#17797 = CARTESIAN_POINT ( 'NONE',  ( -10.37757302488624411, 50.72500000273118559, -31.93888565452638417 ) ) ;
#17798 =( BOUNDED_CURVE ( )  B_SPLINE_CURVE ( 2, ( #27458, #18911, #32595, #3284, #11501, #6357, #21980, #1188, #29679, #19241, #1360, #32429, #29516 ),
 .UNSPECIFIED., .F., .T. ) 
 B_SPLINE_CURVE_WITH_KNOTS ( ( 3, 2, 2, 2, 2, 2, 3 ),
 ( 0.006410256410256410901, 0.007692307692307692735, 0.01025641025641025640, 0.01282051282051282007, 0.01538461538461538547, 0.01794871794871794740, 0.01923076923076923184 ),
 .UNSPECIFIED. ) 
 CURVE ( )  GEOMETRIC_REPRESENTATION_ITEM ( )  RATIONAL_B_SPLINE_CURVE ( ( 0.9755282581475768211, 0.9755282581475768211, 1.000000000000000000, 0.9510565162951535312, 1.000000000000000000, 0.9510565162951535312, 1.000000000000000000, 0.9510565162951535312, 1.000000000000000000, 0.9510565162951535312, 1.000000000000000000, 0.9755282581475767101, 0.9755282581475768211 ) ) 
 REPRESENTATION_ITEM ( '' )  );
#17799 = ORIENTED_EDGE ( 'NONE', *, *, #13656, .F. ) ;
#17800 = CARTESIAN_POINT ( 'NONE',  ( 7.505752307972854531, 36.63541666666666430, -28.01184896238303423 ) ) ;
#17801 = CARTESIAN_POINT ( 'NONE',  ( 28.02196122052045268, 35.20871500092396644, -7.468012846824774620 ) ) ;
#17802 = CARTESIAN_POINT ( 'NONE',  ( 0.000000000000000000, 102.0000000000000284, 14.00000000000000178 ) ) ;
#17803 = CARTESIAN_POINT ( 'NONE',  ( -2.092463501923844636E-15, 8.000000005462366559, -34.17252228774368916 ) ) ;
#17804 = CARTESIAN_POINT ( 'NONE',  ( 0.000000000000000000, 82.00000000000001421, -15.00000000000000000 ) ) ;
#17805 = CARTESIAN_POINT ( 'NONE',  ( 23.41746825000000243, 1.224999997268811480, -7.608796670333727974 ) ) ;
#17806 = CARTESIAN_POINT ( 'NONE',  ( 1.507698388325705758E-15, 9.124999997268822938, -24.62258325217400312 ) ) ;
#17807 = CARTESIAN_POINT ( 'NONE',  ( 33.58253175000000113, 14.37500000273117529, -4.112674001490185761E-15 ) ) ;
#17808 = CARTESIAN_POINT ( 'NONE',  ( -32.50000000000000000, 26.50000000546237544, 0.000000000000000000 ) ) ;
#17809 = CARTESIAN_POINT ( 'NONE',  ( -10.04305231718578462, 64.40000000000000568, 30.90933677959249337 ) ) ;
#17810 = CARTESIAN_POINT ( 'NONE',  ( -3.880418787951124493, 5.448745718453149145, 24.50000000000000355 ) ) ;
#17811 = CARTESIAN_POINT ( 'NONE',  ( 0.000000000000000000, 80.00000000000001421, -32.50000000000000000 ) ) ;
#17812 = CARTESIAN_POINT ( 'NONE',  ( -30.02300923189239867, 61.13319416759063785, -0.04044903254991731589 ) ) ;
#17813 = CARTESIAN_POINT ( 'NONE',  ( 27.16883889988623935, 30.57500000273119412, -19.73931689729374384 ) ) ;
#17814 = CARTESIAN_POINT ( 'NONE',  ( -1.550433958383848148E-15, 111.9999999999999858, -11.32050807568876749 ) ) ;
#17815 = CARTESIAN_POINT ( 'NONE',  ( 26.00068869287367690, 41.07552083333332149, 15.01150461594596486 ) ) ;
#17816 = DIRECTION ( 'NONE',  ( 0.000000000000000000, 0.000000000000000000, 1.000000000000000000 ) ) ;
#17817 = CARTESIAN_POINT ( 'NONE',  ( 7.236395654485755280, 18.72499999726881370, 22.27133577429736988 ) ) ;
#17818 = CARTESIAN_POINT ( 'NONE',  ( -2.092463501923844636E-15, 5.500000000000000888, -34.17252228774368916 ) ) ;
#17819 = COLOUR_RGB ( '', 0.08235294, 0.09019608, 0.10196078) ;
#17820 = CARTESIAN_POINT ( 'NONE',  ( -5.147494310547531704, 52.44874571845315359, 32.49999999999996447 ) ) ;
#17821 = CARTESIAN_POINT ( 'NONE',  ( 6.950374756619257965, 48.94753499907601935, -26.09010956794244507 ) ) ;
#17822 = CARTESIAN_POINT ( 'NONE',  ( -10.37757302488623701, 47.52500000273118985, 31.93888565452638417 ) ) ;
#17823 = CARTESIAN_POINT ( 'NONE',  ( 20.75514604977249178, 62.07500000273118701, 28.56700777964553950 ) ) ;
#17824 = CARTESIAN_POINT ( 'NONE',  ( 33.58253175000000113, 38.37500000273119838, -4.112674001490185761E-15 ) ) ;
#17825 = DIRECTION ( 'NONE',  ( 0.000000000000000000, 0.000000000000000000, -1.000000000000000000 ) ) ;
#17826 = CARTESIAN_POINT ( 'NONE',  ( -13.97622843553632777, 12.14322916666666430, -24.20753774853731599 ) ) ;
#17827 = CARTESIAN_POINT ( 'NONE',  ( 0.000000000000000000, 102.0000000000000284, 0.000000000000000000 ) ) ;
#17828 = CARTESIAN_POINT ( 'NONE',  ( -10.07379044330640028, 16.99999999999998579, -21.64901441059538101 ) ) ;
#17829 = CARTESIAN_POINT ( 'NONE',  ( -10.04305231718578462, 28.40000000000000924, 30.90933677959249337 ) ) ;
#17830 = CARTESIAN_POINT ( 'NONE',  ( -27.16883889988623935, 19.32500000273117280, 19.73931689729374739 ) ) ;
#17831 = CARTESIAN_POINT ( 'NONE',  ( 1.555960095263670572E-15, 16.24999999453762101, -24.50000000000000000 ) ) ;
#17832 = LINE ( 'NONE', #23139, #32517 ) ;
#17833 = LINE ( 'NONE', #25551, #30258 ) ;
#17834 = CARTESIAN_POINT ( 'NONE',  ( -20.53372385742107653, 68.99961833240934084, -20.47846945139867003 ) ) ;
#17835 = CARTESIAN_POINT ( 'NONE',  ( -20.08610463437156923, 44.80000000546235839, 27.64615127144130113 ) ) ;
#17836 = EDGE_CURVE ( 'NONE', #6801, #5893, #28918, .T. ) ;
#17837 = CARTESIAN_POINT ( 'NONE',  ( -32.50000000000000000, 60.40000000546236691, -10.55989012756945300 ) ) ;
#17838 = CARTESIAN_POINT ( 'NONE',  ( 27.16883889988623935, 28.32500000273119412, -19.73931689729374384 ) ) ;
#17839 = AXIS2_PLACEMENT_3D ( 'NONE', #17308, #32893, #17825 ) ;
#17840 = CARTESIAN_POINT ( 'NONE',  ( 24.20753774853731244, 33.62760416666665719, -13.97622843553632599 ) ) ;
#17841 = EDGE_CURVE ( 'NONE', #23226, #4399, #253, .T. ) ;
#17842 = VERTEX_POINT ( 'NONE', #24287 ) ;
#17843 = CARTESIAN_POINT ( 'NONE',  ( 10.37757302488624767, 71.72500000273117848, 31.93888565452638417 ) ) ;
#17844 = CARTESIAN_POINT ( 'NONE',  ( -26.00068869287368756, 42.79427083333331439, -15.01150461594595775 ) ) ;
#17845 = DIRECTION ( 'NONE',  ( 0.000000000000000000, 0.000000000000000000, 1.000000000000000000 ) ) ;
#17846 = ORIENTED_EDGE ( 'NONE', *, *, #32075, .F. ) ;
#17847 = CARTESIAN_POINT ( 'NONE',  ( 28.02196122052045268, 62.70871500092398065, -7.468012846824774620 ) ) ;
#17848 = CARTESIAN_POINT ( 'NONE',  ( -0.04044903254992426173, 63.71131916759064495, 27.95245687107223276 ) ) ;
#17849 = ORIENTED_EDGE ( 'NONE', *, *, #14557, .T. ) ;
#17850 = CARTESIAN_POINT ( 'NONE',  ( 33.58253175000000823, 12.02500000273117742, 10.91162601494192863 ) ) ;
#17851 = CARTESIAN_POINT ( 'NONE',  ( -25.98046417659831420, 16.72097249907602290, 15.04653450569339945 ) ) ;
#17852 = CARTESIAN_POINT ( 'NONE',  ( -2.165007332552593587E-13, 46.50000000000000711, 32.50000000000000000 ) ) ;
#17853 = CARTESIAN_POINT ( 'NONE',  ( 20.75514604977249178, 34.07500000273117990, 28.56700777964553950 ) ) ;
#17854 = CARTESIAN_POINT ( 'NONE',  ( -26.29305231718578995, 44.70000000546237118, 19.10302069950538595 ) ) ;
#17855 = AXIS2_PLACEMENT_3D ( 'NONE', #17008, #11845, #27637 ) ;
#17856 = CARTESIAN_POINT ( 'NONE',  ( 4.635254915624209993, 75.40000000000001990, -14.26584774442730463 ) ) ;
#17857 = CARTESIAN_POINT ( 'NONE',  ( 6.486482029760649416E-15, 25.62500000273118772, 35.31076352940723240 ) ) ;
#17858 = CARTESIAN_POINT ( 'NONE',  ( 3.880418787951172011, 13.30125427608447097, 24.49999999999998579 ) ) ;
#17859 = CARTESIAN_POINT ( 'NONE',  ( -2.162160676586881955E-15, 46.87500000273118417, -35.31076352940723240 ) ) ;
#17860 = PRESENTATION_STYLE_ASSIGNMENT (( #14934 ) ) ;
#17861 = CARTESIAN_POINT ( 'NONE',  ( -2.092463501923844636E-15, 27.50000000000000355, -34.17252228774368916 ) ) ;
#17862 = CARTESIAN_POINT ( 'NONE',  ( -32.50000000000000000, 30.00000000000000000, 0.000000000000000000 ) ) ;
#17863 = CARTESIAN_POINT ( 'NONE',  ( -7.236395654485757944, 15.22499999726881192, -22.27133577429736988 ) ) ;
#17864 = CARTESIAN_POINT ( 'NONE',  ( 33.58253175000000113, 68.22500000273116427, -10.91162601494193751 ) ) ;
#17865 = FACE_BOUND ( 'NONE', #22510, .T. ) ;
#17866 = CARTESIAN_POINT ( 'NONE',  ( -24.50000000000000000, 14.89999999999999503, -7.960532557706207157 ) ) ;
#17867 = CARTESIAN_POINT ( 'NONE',  ( -33.58253175000000113, 61.47500000273118559, 10.91162601494193929 ) ) ;
#17868 = CARTESIAN_POINT ( 'NONE',  ( -4.635254915624208216, 76.65000000546234560, 14.26584774442730463 ) ) ;
#17869 = CARTESIAN_POINT ( 'NONE',  ( 26.29305231718579350, 72.79999999999999716, 19.10302069950537529 ) ) ;
#17870 = CARTESIAN_POINT ( 'NONE',  ( -20.75514604977248112, 19.42500000273117777, 28.56700777964554661 ) ) ;
#17871 = CARTESIAN_POINT ( 'NONE',  ( -24.50000000000001066, 10.84999999453761887, 7.960532557706201828 ) ) ;
#17872 = CARTESIAN_POINT ( 'NONE',  ( -24.18731323226248264, 23.60715250092398421, -14.01125832528284931 ) ) ;
#17873 = CARTESIAN_POINT ( 'NONE',  ( 26.29305231718579350, 46.80000000000001137, 19.10302069950537529 ) ) ;
#17874 = CARTESIAN_POINT ( 'NONE',  ( 33.58253175000000113, 40.12500000273118417, -4.112674001490185761E-15 ) ) ;
#17875 = DIRECTION ( 'NONE',  ( 0.000000000000000000, 0.000000000000000000, 1.000000000000000000 ) ) ;
#17876 = CARTESIAN_POINT ( 'NONE',  ( -27.16883889988623935, 55.57500000273117280, 19.73931689729374739 ) ) ;
#17877 = CARTESIAN_POINT ( 'NONE',  ( 7.468012846824777284, 49.81809000092397355, 28.02196122052045268 ) ) ;
#17878 = CARTESIAN_POINT ( 'NONE',  ( 3.445340210940985210E-14, 5.499999999999997335, 24.50000000000000000 ) ) ;
#17879 = CARTESIAN_POINT ( 'NONE',  ( 7.543491769121922985, 33.19232666574268364, 28.00173670424535644 ) ) ;
#17880 = CARTESIAN_POINT ( 'NONE',  ( 20.08610463437157279, 59.80000000546235839, -27.64615127144129758 ) ) ;
#17881 = EDGE_CURVE ( 'NONE', #17796, #12037, #3064, .T. ) ;
#17882 = CARTESIAN_POINT ( 'NONE',  ( 13.91746824999999887, 73.87500000273116996, -1.704398294459741270E-15 ) ) ;
#17883 = CARTESIAN_POINT ( 'NONE',  ( -24.50000000000000000, 2.649999994537616477, -7.960532557706207157 ) ) ;
#17884 = CONICAL_SURFACE ( 'NONE', #32620, 26.50000000000000000, 1.047197551196594523 ) ;
#17885 = CARTESIAN_POINT ( 'NONE',  ( -27.95245687107223986, 61.69493083240936926, 0.04044903255043252877 ) ) ;
#17886 = CARTESIAN_POINT ( 'NONE',  ( -4.523095164977116484E-15, 2.624999997268825158, 24.62258325217400312 ) ) ;
#17887 = CARTESIAN_POINT ( 'NONE',  ( -20.75514604977248112, 1.425000002731191984, 28.56700777964554661 ) ) ;
#17888 = CARTESIAN_POINT ( 'NONE',  ( 2.375766604868040144, 78.55125428154684641, 15.00000000000000178 ) ) ;
#17889 = CARTESIAN_POINT ( 'NONE',  ( -27.16883889988623935, 33.57500000273118701, 19.73931689729374739 ) ) ;
#17890 = CARTESIAN_POINT ( 'NONE',  ( 1.507698388325705758E-15, 9.624999997268808727, -24.62258325217400312 ) ) ;
#17891 = ORIENTED_EDGE ( 'NONE', *, *, #16553, .F. ) ;
#17892 = CARTESIAN_POINT ( 'NONE',  ( 27.16883889988623935, 72.57500000273120122, -19.73931689729374384 ) ) ;
#17893 = CARTESIAN_POINT ( 'NONE',  ( 6.277390505771533514E-15, 21.00000000546236478, 34.17252228774368916 ) ) ;
#17894 = CARTESIAN_POINT ( 'NONE',  ( 15.01150461594643204, 44.79947916666667140, 26.00068869287340334 ) ) ;
#17895 = CARTESIAN_POINT ( 'NONE',  ( -33.58253175000000113, 51.37500000273120548, 0.000000000000000000 ) ) ;
#17896 = CARTESIAN_POINT ( 'NONE',  ( -20.08610463437156923, 60.80000000546239391, 27.64615127144130113 ) ) ;
#17897 = ORIENTED_EDGE ( 'NONE', *, *, #21266, .F. ) ;
#17898 = CARTESIAN_POINT ( 'NONE',  ( 7.570916362186213000, 6.149999994537635573, -23.30088464923126423 ) ) ;
#17899 = CARTESIAN_POINT ( 'NONE',  ( -33.58253175000000113, 45.22500000273117848, 10.91162601494193929 ) ) ;
#17900 = CARTESIAN_POINT ( 'NONE',  ( -14.47279130897152122, 17.92499999726880588, 19.92008829642072243 ) ) ;
#17901 = CARTESIAN_POINT ( 'NONE',  ( -10.37757302488624411, 70.97500000273119269, -31.93888565452638417 ) ) ;
#17902 = CARTESIAN_POINT ( 'NONE',  ( -10.04305231718578462, 2.900000005462366470, 30.90933677959249337 ) ) ;
#17903 = CARTESIAN_POINT ( 'NONE',  ( 33.58253175000000113, 62.22500000273119269, -10.91162601494193574 ) ) ;
#17904 = CYLINDRICAL_SURFACE ( 'NONE', #12777, 32.50000000000000000 ) ;
#17905 = CARTESIAN_POINT ( 'NONE',  ( -20.08610463437157989, 45.69999999999998863, -27.64615127144129758 ) ) ;
#17906 = CARTESIAN_POINT ( 'NONE',  ( 12.11607355459420710, -70.99969134886156041, 1.483791069686768383E-15 ) ) ;
#17907 = CARTESIAN_POINT ( 'NONE',  ( 33.58253175000000113, 16.47500000273118204, -10.91162601494193751 ) ) ;
#17908 = CARTESIAN_POINT ( 'NONE',  ( 1.555960095263670572E-15, 6.499999999999994671, -24.50000000000000000 ) ) ;
#17909 = CARTESIAN_POINT ( 'NONE',  ( -7.025853678916861966, 24.59857666574268720, -26.06988505166722803 ) ) ;
#17910 = CARTESIAN_POINT ( 'NONE',  ( 13.91746824999999887, 80.37500000273118417, -1.704398294459741270E-15 ) ) ;
#17911 = DIRECTION ( 'NONE',  ( -0.000000000000000000, -1.000000000000000000, -0.000000000000000000 ) ) ;
#17912 = CARTESIAN_POINT ( 'NONE',  ( -10.04305231718578462, 44.39999999999999147, 30.90933677959249337 ) ) ;
#17913 =( BOUNDED_CURVE ( )  B_SPLINE_CURVE ( 2, ( #18457, #26336, #2825, #13294, #23767, #234, #14300, #9298, #8972, #11545, #22522, #22358, #32805 ),
 .UNSPECIFIED., .F., .F. ) 
 B_SPLINE_CURVE_WITH_KNOTS ( ( 3, 2, 2, 2, 2, 2, 3 ),
 ( 0.9294871794871795156, 0.9307692307692307931, 0.9333333333333333481, 0.9358974358974359031, 0.9384615384615384581, 0.9410256410256410131, 0.9423076923076922906 ),
 .UNSPECIFIED. ) 
 CURVE ( )  GEOMETRIC_REPRESENTATION_ITEM ( )  RATIONAL_B_SPLINE_CURVE ( ( 0.9755282581475768211, 0.9755282581475768211, 1.000000000000000000, 0.9510565162951535312, 1.000000000000000000, 0.9510565162951535312, 1.000000000000000000, 0.9510565162951535312, 1.000000000000000000, 0.9510565162951535312, 1.000000000000000000, 0.9755282581475768211, 0.9755282581475768211 ) ) 
 REPRESENTATION_ITEM ( '' )  );
#17914 = CARTESIAN_POINT ( 'NONE',  ( 33.58253175000000823, 72.27500000273118985, 10.91162601494192863 ) ) ;
#17915 = EDGE_LOOP ( 'NONE', ( #18442, #32869, #29141, #9941 ) ) ;
#17916 = CARTESIAN_POINT ( 'NONE',  ( 23.41746825000000243, 11.02499999726882152, 7.608796670333735079 ) ) ;
#17917 = CARTESIAN_POINT ( 'NONE',  ( 7.236395654485760609, 3.024999997268823293, -22.27133577429736633 ) ) ;
#17918 = CARTESIAN_POINT ( 'NONE',  ( 27.95245687107222921, 47.66406249999998579, -2.463307335887066074E-13 ) ) ;
#17919 =( BOUNDED_CURVE ( )  B_SPLINE_CURVE ( 2, ( #1618, #10224, #33726, #15372, #20004, #25662, #33017, #20703, #33546, #12268, #12096, #20346, #25827 ),
 .UNSPECIFIED., .F., .F. ) 
 B_SPLINE_CURVE_WITH_KNOTS ( ( 3, 2, 2, 2, 2, 2, 3 ),
 ( 0.6944444444444444198, 0.6999999999999999556, 0.7111111111111111382, 0.7222222222222222099, 0.7333333333333332815, 0.7444444444444444642, 0.7500000000000000000 ),
 .UNSPECIFIED. ) 
 CURVE ( )  GEOMETRIC_REPRESENTATION_ITEM ( )  RATIONAL_B_SPLINE_CURVE ( ( 0.9755282581475768211, 0.9755282581475768211, 1.000000000000000000, 0.9510565162951535312, 1.000000000000000000, 0.9510565162951535312, 1.000000000000000000, 0.9510565162951535312, 1.000000000000000000, 0.9510565162951535312, 1.000000000000000000, 0.9755282581475768211, 0.9755282581475768211 ) ) 
 REPRESENTATION_ITEM ( '' )  );
#17920 = CARTESIAN_POINT ( 'NONE',  ( -20.75514604977248112, 63.42500000273118133, 28.56700777964554661 ) ) ;
#17921 = CARTESIAN_POINT ( 'NONE',  ( -33.58253175000000113, 17.47500000273117848, 10.91162601494193929 ) ) ;
#17922 = CARTESIAN_POINT ( 'NONE',  ( -2.162160676586881955E-15, 10.87500000273118417, -35.31076352940723240 ) ) ;
#17923 = CARTESIAN_POINT ( 'NONE',  ( -2.428612866367529427E-13, 29.61718749999999645, -27.95245687107223276 ) ) ;
#17924 = CARTESIAN_POINT ( 'NONE',  ( 7.543491769121427382, 17.44829833425730925, -28.00173670424548433 ) ) ;
#17925 = CARTESIAN_POINT ( 'NONE',  ( 30.02300923189239512, 61.41406250000000711, -2.619432448724977703E-13 ) ) ;
#17926 = CARTESIAN_POINT ( 'NONE',  ( 20.75514604977249178, 1.825000002731179460, 28.56700777964553950 ) ) ;
#17927 = CARTESIAN_POINT ( 'NONE',  ( 26.29305231718578995, 3.199999999999980638, -19.10302069950538240 ) ) ;
#17928 = CARTESIAN_POINT ( 'NONE',  ( -26.29305231718578995, 44.20000000000000284, 19.10302069950538595 ) ) ;
#17929 = CARTESIAN_POINT ( 'NONE',  ( -33.58253175000000113, 47.22500000273117138, 10.91162601494193929 ) ) ;
#17930 = PRODUCT_RELATED_PRODUCT_CATEGORY ( 'part', '', ( #23326 ) ) ;
#17931 = CARTESIAN_POINT ( 'NONE',  ( 23.41746825000000243, 6.724999997268811924, -7.608796670333727974 ) ) ;
#17932 = CARTESIAN_POINT ( 'NONE',  ( 3.880418787951134707, 13.55125428154684997, 24.50000000000000000 ) ) ;
#17933 = ORIENTED_EDGE ( 'NONE', *, *, #23007, .T. ) ;
#17934 = CARTESIAN_POINT ( 'NONE',  ( -2.162160676586881955E-15, 54.87500000273119127, -35.31076352940723240 ) ) ;
#17935 = DIRECTION ( 'NONE',  ( 0.000000000000000000, 0.000000000000000000, 1.000000000000000000 ) ) ;
#17936 = CARTESIAN_POINT ( 'NONE',  ( -6.950374756619716266, 41.22434000092397355, -26.09010956794232428 ) ) ;
#17937 = CARTESIAN_POINT ( 'NONE',  ( -33.58253175000000113, 73.37500000273116996, 0.000000000000000000 ) ) ;
#17938 = ORIENTED_EDGE ( 'NONE', *, *, #30695, .T. ) ;
#17939 = CARTESIAN_POINT ( 'NONE',  ( -27.16883889988624290, 22.92500000273119198, -19.73931689729374028 ) ) ;
#17940 = CARTESIAN_POINT ( 'NONE',  ( 30.02300923189239512, 20.16406249999999645, -2.619432448724977703E-13 ) ) ;
#17941 = EDGE_LOOP ( 'NONE', ( #27028, #14660, #10712, #24294 ) ) ;
#17942 = CARTESIAN_POINT ( 'NONE',  ( -1.778240108872766143E-15, 24.00000000546237899, -32.49999999999999289 ) ) ;
#17943 = CARTESIAN_POINT ( 'NONE',  ( -10.37757302488623701, 59.52500000273119696, 31.93888565452638417 ) ) ;
#17944 = CARTESIAN_POINT ( 'NONE',  ( -7.505752307972844761, 41.79166666666666430, 28.01184896238304134 ) ) ;
#17945 = AXIS2_PLACEMENT_3D ( 'NONE', #11739, #27700, #9678 ) ;
#17946 = CARTESIAN_POINT ( 'NONE',  ( 19.82091636218621034, 11.80000000000000426, 14.40073868116559730 ) ) ;
#17947 = CARTESIAN_POINT ( 'NONE',  ( -23.41746824999999887, 4.124999997268813168, -2.867812753649727150E-15 ) ) ;
#17948 = CARTESIAN_POINT ( 'NONE',  ( -33.58253175000000113, 9.125000002731198379, 0.000000000000000000 ) ) ;
#17949 = CARTESIAN_POINT ( 'NONE',  ( 5.147494310547426899, 29.44874571845315714, -32.50000000000000000 ) ) ;
#17950 = CARTESIAN_POINT ( 'NONE',  ( 14.97647472619900455, 55.96576416574269786, -26.02091320914876960 ) ) ;
#17951 = CARTESIAN_POINT ( 'NONE',  ( 4.635254915624212657, 76.59999999999999432, 14.26584774442730286 ) ) ;
#17952 = FACE_OUTER_BOUND ( 'NONE', #705, .T. ) ;
#17953 = CARTESIAN_POINT ( 'NONE',  ( 26.29305231718579350, 19.30000000546239391, 19.10302069950537529 ) ) ;
#17954 = CARTESIAN_POINT ( 'NONE',  ( -20.08610463437157989, 17.69999999999999218, -27.64615127144129758 ) ) ;
#17955 = CARTESIAN_POINT ( 'NONE',  ( 19.82091636218621389, 11.94999999453763628, -14.40073868116559197 ) ) ;
#17956 = CARTESIAN_POINT ( 'NONE',  ( 8.601468415847520532, 79.57500000273120122, 11.83890561707634781 ) ) ;
#17957 = CARTESIAN_POINT ( 'NONE',  ( -13.97622843553588901, 24.74739583333332504, 24.20753774853756823 ) ) ;
#17958 = CARTESIAN_POINT ( 'NONE',  ( -33.58253175000000113, 29.22500000273118914, 10.91162601494193929 ) ) ;
#17959 = CARTESIAN_POINT ( 'NONE',  ( -27.16883889988624290, 76.92500000273120975, -19.73931689729374028 ) ) ;
#17960 = CARTESIAN_POINT ( 'NONE',  ( -27.16883889988624290, 41.17500000273118133, -19.73931689729374028 ) ) ;
#17961 = CARTESIAN_POINT ( 'NONE',  ( -27.16883889988624290, 21.17500000273120264, -19.73931689729374028 ) ) ;
#17962 = CARTESIAN_POINT ( 'NONE',  ( -15.14183272437242778, 7.300000000000001599, 20.84094480462497856 ) ) ;
#17963 = CARTESIAN_POINT ( 'NONE',  ( 20.75514604977249178, 75.82500000273118701, 28.56700777964553950 ) ) ;
#17964 = CARTESIAN_POINT ( 'NONE',  ( 5.779280353836490358E-15, 66.49999999999998579, 32.49999999999999289 ) ) ;
#17965 = CARTESIAN_POINT ( 'NONE',  ( -32.50000000000000000, 61.99999999999998579, 0.000000000000000000 ) ) ;
#17966 = CARTESIAN_POINT ( 'NONE',  ( -7.236395654485757944, 15.22499999726881192, -22.27133577429736988 ) ) ;
#17967 = CARTESIAN_POINT ( 'NONE',  ( -2.162160676586882350E-15, 62.62500000273117706, -35.31076352940722529 ) ) ;
#17968 = CARTESIAN_POINT ( 'NONE',  ( -14.47279130897151589, 9.824999997268802687, -19.92008829642072598 ) ) ;
#17969 = CARTESIAN_POINT ( 'NONE',  ( 20.75514604977248467, 72.67500000273118133, -28.56700777964554305 ) ) ;
#17970 = CARTESIAN_POINT ( 'NONE',  ( -33.58253175000000113, 5.025000002731194293, -10.91162601494193041 ) ) ;
#17971 = CARTESIAN_POINT ( 'NONE',  ( 14.47279130897151767, 2.924999997268815655, -19.92008829642072598 ) ) ;
#17972 = CARTESIAN_POINT ( 'NONE',  ( 14.01125832528286352, 10.71652750092397888, -24.18731323226246843 ) ) ;
#17973 = EDGE_CURVE ( 'NONE', #969, #22307, #21215, .T. ) ;
#17974 = VERTEX_POINT ( 'NONE', #11400 ) ;
#17975 = CARTESIAN_POINT ( 'NONE',  ( -33.58253175000000113, 43.12500000273118417, 0.000000000000000000 ) ) ;
#17976 = VERTEX_POINT ( 'NONE', #27186 ) ;
#17977 = CARTESIAN_POINT ( 'NONE',  ( -2.584737979205441561E-13, 46.80468750000000000, -30.02300923189239512 ) ) ;
#17978 = DIRECTION ( 'NONE',  ( 0.000000000000000000, 0.000000000000000000, -1.000000000000000000 ) ) ;
#17979 = CARTESIAN_POINT ( 'NONE',  ( 6.277390505771533514E-15, 7.000000005462369224, 34.17252228774368916 ) ) ;
#17980 = CARTESIAN_POINT ( 'NONE',  ( -3.880418787951146697, 2.551254281546845526, -24.49999999999999645 ) ) ;
#17981 = CARTESIAN_POINT ( 'NONE',  ( -7.236395654485757944, 1.724999997268800156, -22.27133577429736988 ) ) ;
#17982 = ADVANCED_FACE ( 'NONE', ( #16236 ), #16399, .T. ) ;
#17983 = EDGE_CURVE ( 'NONE', #21829, #22725, #587, .T. ) ;
#17984 = CARTESIAN_POINT ( 'NONE',  ( 18.94512977948575738, 10.42499999726881299, 13.76444248337723408 ) ) ;
#17985 = CARTESIAN_POINT ( 'NONE',  ( 27.16883889988623935, 18.57500000273118346, -19.73931689729374384 ) ) ;
#17986 = CARTESIAN_POINT ( 'NONE',  ( -10.04305231718578462, 16.90000000546237757, 30.90933677959249337 ) ) ;
#17987 = CARTESIAN_POINT ( 'NONE',  ( -32.50000000000000000, 66.00000000000000000, 0.000000000000000000 ) ) ;
#17988 = DIRECTION ( 'NONE',  ( -1.000000000000000000, -1.145572106777136737E-16, 0.000000000000000000 ) ) ;
#17989 = DIRECTION ( 'NONE',  ( -0.000000000000000000, 1.000000000000000000, -0.000000000000000000 ) ) ;
#17990 = CARTESIAN_POINT ( 'NONE',  ( 20.50609665441005092, 13.71874999999999467, 20.50609665440969209 ) ) ;
#17991 = CARTESIAN_POINT ( 'NONE',  ( -2.162160676586881955E-15, 28.87500000273119838, -35.31076352940723240 ) ) ;
#17992 = CARTESIAN_POINT ( 'NONE',  ( 5.779280353836490358E-15, 33.00000000546238965, 32.49999999999999289 ) ) ;
#17993 = CARTESIAN_POINT ( 'NONE',  ( 20.50609665440969565, 40.35937499999999289, -20.50609665441004736 ) ) ;
#17994 = EDGE_CURVE ( 'NONE', #9084, #29760, #19140, .T. ) ;
#17995 = CARTESIAN_POINT ( 'NONE',  ( 14.47279130897151589, 16.82499999726881512, 19.92008829642072953 ) ) ;
#17996 = CARTESIAN_POINT ( 'NONE',  ( -26.29305231718579350, 5.799999999999999822, -19.10302069950537884 ) ) ;
#17997 = AXIS2_PLACEMENT_3D ( 'NONE', #28450, #33781, #28789 ) ;
#17998 = CARTESIAN_POINT ( 'NONE',  ( -15.00000000000000000, 74.10000000000000853, 4.873795443493597723 ) ) ;
#17999 = CARTESIAN_POINT ( 'NONE',  ( -0.04044903255042732459, 52.24180583240936215, -27.95245687107223986 ) ) ;
#18000 = CARTESIAN_POINT ( 'NONE',  ( 33.58253175000000113, 52.22500000273117848, -10.91162601494193751 ) ) ;
#18001 = CARTESIAN_POINT ( 'NONE',  ( -10.37757302488624411, 60.97500000273119269, -31.93888565452638417 ) ) ;
#18002 = CARTESIAN_POINT ( 'NONE',  ( 6.486482029760648627E-15, 39.87500000273119127, 35.31076352940722529 ) ) ;
#18003 = CARTESIAN_POINT ( 'NONE',  ( -14.47279130897152299, 15.92499999726881121, 19.92008829642072243 ) ) ;
#18004 = DIRECTION ( 'NONE',  ( -1.000000000000000000, -1.063101997391471025E-16, 0.000000000000000000 ) ) ;
#18005 = CYLINDRICAL_SURFACE ( 'NONE', #17997, 32.50000000000000000 ) ;
#18006 = CARTESIAN_POINT ( 'NONE',  ( -2.165007332552593587E-13, 51.00000000546238255, 32.50000000000000000 ) ) ;
#18007 = CARTESIAN_POINT ( 'NONE',  ( 10.04305231718579705, 76.59999999999999432, 30.90933677959248982 ) ) ;
#18008 = CARTESIAN_POINT ( 'NONE',  ( -27.16883889988624290, 12.92500000273118310, -19.73931689729374028 ) ) ;
#18009 = DIRECTION ( 'NONE',  ( 0.000000000000000000, 0.000000000000000000, 1.000000000000000000 ) ) ;
#18010 = DIRECTION ( 'NONE',  ( -0.000000000000000000, -1.000000000000000000, -0.000000000000000000 ) ) ;
#18011 = CARTESIAN_POINT ( 'NONE',  ( 19.06425588902558133, 14.85899333240935505, -19.11951029504797006 ) ) ;
#18012 = CARTESIAN_POINT ( 'NONE',  ( 32.50000000000000711, 37.40000000546236691, 10.55989012756945122 ) ) ;
#18013 =( BOUNDED_CURVE ( )  B_SPLINE_CURVE ( 2, ( #16666, #27123, #24711, #29856, #3949, #3616, #8925, #17001, #14090, #24547, #1018, #14424, #24878 ),
 .UNSPECIFIED., .F., .T. ) 
 B_SPLINE_CURVE_WITH_KNOTS ( ( 3, 2, 2, 2, 2, 2, 3 ),
 ( 0.1987179487179487336, 0.2000000000000000111, 0.2025641025641025661, 0.2051282051282051211, 0.2076923076923077038, 0.2102564102564102588, 0.2115384615384615363 ),
 .UNSPECIFIED. ) 
 CURVE ( )  GEOMETRIC_REPRESENTATION_ITEM ( )  RATIONAL_B_SPLINE_CURVE ( ( 0.9755282581475768211, 0.9755282581475770431, 1.000000000000000000, 0.9510565162951535312, 1.000000000000000000, 0.9510565162951535312, 1.000000000000000000, 0.9510565162951535312, 1.000000000000000000, 0.9510565162951535312, 1.000000000000000000, 0.9755282581475768211, 0.9755282581475768211 ) ) 
 REPRESENTATION_ITEM ( '' )  );
#18014 = CARTESIAN_POINT ( 'NONE',  ( 26.29305231718579350, 10.80000000000000426, 19.10302069950537529 ) ) ;
#18015 = CARTESIAN_POINT ( 'NONE',  ( -10.37757302488623701, 27.52500000273119696, 31.93888565452638417 ) ) ;
#18016 = CARTESIAN_POINT ( 'NONE',  ( 19.09188309203661049, 40.35937499999999289, -19.09188309203694445 ) ) ;
#18017 = EDGE_LOOP ( 'NONE', ( #21394, #8748, #8160, #32290 ) ) ;
#18018 = CARTESIAN_POINT ( 'NONE',  ( 27.16883889988623935, 66.32500000273118701, -19.73931689729374384 ) ) ;
#18019 = CARTESIAN_POINT ( 'NONE',  ( 15.01150461594596308, 47.09114583333332860, -26.00068869287367335 ) ) ;
#18020 = ORIENTED_EDGE ( 'NONE', *, *, #13072, .F. ) ;
#18021 = CARTESIAN_POINT ( 'NONE',  ( 0.04044903254992426173, 58.55506916759063785, -30.02300923189239867 ) ) ;
#18022 = CARTESIAN_POINT ( 'NONE',  ( 19.06425588902592239, 59.84413166759065206, 19.11951029504763611 ) ) ;
#18023 = EDGE_LOOP ( 'NONE', ( #20249, #30867, #12728, #7700 ) ) ;
#18024 = CARTESIAN_POINT ( 'NONE',  ( 33.58253175000000113, 12.12500000273118772, -4.112674001490185761E-15 ) ) ;
#18025 = CARTESIAN_POINT ( 'NONE',  ( 30.02300923189239867, 18.72618083240936215, -0.04044903255044467877 ) ) ;
#18026 = CARTESIAN_POINT ( 'NONE',  ( 0.000000000000000000, 16.99999999999998579, 0.000000000000000000 ) ) ;
#18027 = CARTESIAN_POINT ( 'NONE',  ( -33.58253175000000113, 33.27500000273120406, -10.91162601494193218 ) ) ;
#18028 = CARTESIAN_POINT ( 'NONE',  ( -26.29305231718579350, 34.30000000546237970, -19.10302069950537884 ) ) ;
#18029 = CARTESIAN_POINT ( 'NONE',  ( 15.00000000000000355, 76.90000000000000568, 4.873795443493592394 ) ) ;
#18030 = CARTESIAN_POINT ( 'NONE',  ( 15.01150461594643204, 65.42447916666667140, 26.00068869287340334 ) ) ;
#18031 = CARTESIAN_POINT ( 'NONE',  ( -27.16883889988623935, 21.32500000273118701, 19.73931689729374739 ) ) ;
#18032 = CARTESIAN_POINT ( 'NONE',  ( 3.880418787951134707, 5.301254276084462980, 24.50000000000000000 ) ) ;
#18033 = CARTESIAN_POINT ( 'NONE',  ( 27.16883889988623935, 46.57500000273117990, -19.73931689729374384 ) ) ;
#18034 = CARTESIAN_POINT ( 'NONE',  ( 6.277390505771533514E-15, 32.49999999999999289, 34.17252228774368916 ) ) ;
#18035 = CARTESIAN_POINT ( 'NONE',  ( 10.04305231718578817, 29.40000000000000924, -30.90933677959249337 ) ) ;
#18036 = CARTESIAN_POINT ( 'NONE',  ( -7.570916362186215665, 1.400000000000012346, 23.30088464923126423 ) ) ;
#18037 = EDGE_CURVE ( 'NONE', #3193, #19899, #29420, .T. ) ;
#18038 = CARTESIAN_POINT ( 'NONE',  ( -33.58253175000000113, 71.02500000273118985, -10.91162601494193218 ) ) ;
#18039 = CARTESIAN_POINT ( 'NONE',  ( 32.50000000000000000, 63.10000000000001563, -10.55989012756945833 ) ) ;
#18040 = CARTESIAN_POINT ( 'NONE',  ( -13.91746824999999532, 75.47500000273116427, 4.522059556121122093 ) ) ;
#18041 = CARTESIAN_POINT ( 'NONE',  ( 27.16883889988623935, 62.57500000273119412, -19.73931689729374384 ) ) ;
#18042 = FACE_OUTER_BOUND ( 'NONE', #1397, .T. ) ;
#18043 = CARTESIAN_POINT ( 'NONE',  ( -20.75514604977248823, 8.825000002731190563, -28.56700777964554305 ) ) ;
#18044 = CARTESIAN_POINT ( 'NONE',  ( -0.04044903254992426173, 29.33631916759064850, 27.95245687107223276 ) ) ;
#18045 = CARTESIAN_POINT ( 'NONE',  ( 25.94559702212998076, 66.99999999999998579, -20.21712673764820423 ) ) ;
#18046 = CARTESIAN_POINT ( 'NONE',  ( 33.58253175000000113, 36.12500000273118417, -4.112674001490185761E-15 ) ) ;
#18047 = CARTESIAN_POINT ( 'NONE',  ( 26.29305231718578995, 57.20000000000001705, -19.10302069950538240 ) ) ;
#18048 = CARTESIAN_POINT ( 'NONE',  ( 20.08610463437158344, 18.69999999999999574, 27.64615127144129403 ) ) ;
#18049 = CARTESIAN_POINT ( 'NONE',  ( 3.880418787951172011, 15.55125428154684819, 24.49999999999998579 ) ) ;
#18050 = CARTESIAN_POINT ( 'NONE',  ( -28.00173670424535644, 44.36420166574269075, 7.543491769121936308 ) ) ;
#18051 = CARTESIAN_POINT ( 'NONE',  ( 26.29305231718579350, 61.30000000546238681, 19.10302069950537529 ) ) ;
#18052 = CARTESIAN_POINT ( 'NONE',  ( -8.601468415847515203, 73.67500000273118133, 11.83890561707634959 ) ) ;
#18053 = CARTESIAN_POINT ( 'NONE',  ( 19.11951029504797006, 63.84336833240935505, 19.06425588902558133 ) ) ;
#18054 = CARTESIAN_POINT ( 'NONE',  ( -20.08610463437157989, 76.20000000546235697, -27.64615127144129758 ) ) ;
#18055 = CARTESIAN_POINT ( 'NONE',  ( -7.505752307973343918, 19.16145833333332860, -28.01184896238290989 ) ) ;
#18056 = CARTESIAN_POINT ( 'NONE',  ( 33.58253175000000113, 32.47500000273117138, -10.91162601494193751 ) ) ;
#18057 = CARTESIAN_POINT ( 'NONE',  ( 23.41746824999999887, 5.024999997268808194, 7.608796670333735079 ) ) ;
#18058 = EDGE_LOOP ( 'NONE', ( #2390, #24823, #6197, #22548 ) ) ;
#18059 = CARTESIAN_POINT ( 'NONE',  ( -33.58253175000000113, 77.37500000273116996, 0.000000000000000000 ) ) ;
#18060 = CARTESIAN_POINT ( 'NONE',  ( -20.08610463437156923, 24.80000000546235839, 27.64615127144130113 ) ) ;
#18061 = CARTESIAN_POINT ( 'NONE',  ( -28.01184896238304134, 46.08854166666666430, -7.505752307972844761 ) ) ;
#18062 = CARTESIAN_POINT ( 'NONE',  ( 20.50609665441005092, 58.40625000000000711, 20.50609665440969209 ) ) ;
#18063 = CARTESIAN_POINT ( 'NONE',  ( -33.58253175000000113, 53.27500000273117564, -10.91162601494193218 ) ) ;
#18064 = CARTESIAN_POINT ( 'NONE',  ( -32.50000000000000000, 60.40000000546236691, -10.55989012756945478 ) ) ;
#18065 = CARTESIAN_POINT ( 'NONE',  ( 33.58253175000000823, 44.02500000273118275, 10.91162601494192863 ) ) ;
#18066 = CARTESIAN_POINT ( 'NONE',  ( -12.13525491562420910, 76.45000000546237118, 8.816778784387098611 ) ) ;
#18067 = CARTESIAN_POINT ( 'NONE',  ( -27.16883889988623935, 67.57500000273120122, 19.73931689729374739 ) ) ;
#18068 = CARTESIAN_POINT ( 'NONE',  ( 32.50000000000000711, 7.400000005462386454, 10.55989012756945122 ) ) ;
#18069 = CARTESIAN_POINT ( 'NONE',  ( -33.58253175000000113, 63.12500000273117706, 0.000000000000000000 ) ) ;
#18070 = CARTESIAN_POINT ( 'NONE',  ( 7.236395654485755280, 18.72499999726881370, 22.27133577429736988 ) ) ;
#18071 = CARTESIAN_POINT ( 'NONE',  ( 10.04305231718578817, 45.39999999999999858, -30.90933677959249337 ) ) ;
#18072 = CYLINDRICAL_SURFACE ( 'NONE', #613, 30.50000000000000000 ) ;
#18073 = CARTESIAN_POINT ( 'NONE',  ( -33.58253175000000113, 9.275000002731177418, -10.91162601494193218 ) ) ;
#18074 = CARTESIAN_POINT ( 'NONE',  ( -24.50000000000000711, 7.100000000000008527, 7.960532557706201828 ) ) ;
#18075 = CARTESIAN_POINT ( 'NONE',  ( -19.06425588902558133, 30.32774333240935150, 19.11951029504797006 ) ) ;
#18076 = CARTESIAN_POINT ( 'NONE',  ( 8.601468415847520532, 80.07500000273118701, 11.83890561707634781 ) ) ;
#18077 = CARTESIAN_POINT ( 'NONE',  ( -4.000000000000003553, 0.000000000000000000, 0.000000000000000000 ) ) ;
#18078 = CARTESIAN_POINT ( 'NONE',  ( 2.067204126564591252E-14, 4.499999999999996447, -24.50000000000000000 ) ) ;
#18079 = EDGE_CURVE ( 'NONE', #22980, #22878, #24445, .T. ) ;
#18080 = CARTESIAN_POINT ( 'NONE',  ( 33.58253175000000823, 74.27500000273117564, 10.91162601494192863 ) ) ;
#18081 = VERTEX_POINT ( 'NONE', #11240 ) ;
#18082 = CARTESIAN_POINT ( 'NONE',  ( -23.41746824999999887, 12.12499999726882116, -2.867812753649727150E-15 ) ) ;
#18083 = CARTESIAN_POINT ( 'NONE',  ( 7.236395654485760609, 1.024999997268821739, -22.27133577429736633 ) ) ;
#18084 = CARTESIAN_POINT ( 'NONE',  ( 27.95245687107222921, 51.10156249999998579, -2.463307335887066074E-13 ) ) ;
#18085 = CARTESIAN_POINT ( 'NONE',  ( -2.162160676586881955E-15, 58.62500000273118417, -35.31076352940723240 ) ) ;
#18086 = CARTESIAN_POINT ( 'NONE',  ( 6.486482029760649416E-15, 19.87500000273119483, 35.31076352940723240 ) ) ;
#18087 = CARTESIAN_POINT ( 'NONE',  ( 10.37757302488624767, 1.975000002731180926, 31.93888565452638417 ) ) ;
#18088 = CARTESIAN_POINT ( 'NONE',  ( -24.20753774853756823, 42.79427083333332149, -13.97622843553588723 ) ) ;
#18089 = UNCERTAINTY_MEASURE_WITH_UNIT (LENGTH_MEASURE( 1.000000000000000082E-05 ), #1877, 'distance_accuracy_value', 'NONE');
#18090 = CARTESIAN_POINT ( 'NONE',  ( -30.02300923189239867, 19.88319416759064495, -0.04044903254991731589 ) ) ;
#18091 = CARTESIAN_POINT ( 'NONE',  ( -30.02300923189239512, 66.57031250000000000, 2.654126918244515359E-13 ) ) ;
#18092 = CARTESIAN_POINT ( 'NONE',  ( 6.486482029760649416E-15, 3.625000002731194826, 35.31076352940723240 ) ) ;
#18093 = DIRECTION ( 'NONE',  ( -0.000000000000000000, -1.000000000000000000, -0.000000000000000000 ) ) ;
#18094 = CARTESIAN_POINT ( 'NONE',  ( -27.16883889988624290, 46.92500000273119554, -19.73931689729374028 ) ) ;
#18095 = CARTESIAN_POINT ( 'NONE',  ( 18.94512977948576093, 8.824999997268822227, -13.76444248337722875 ) ) ;
#18096 = CARTESIAN_POINT ( 'NONE',  ( 2.375766604868043252, 79.44874571845313938, -14.99999999999999822 ) ) ;
#18097 = ORIENTED_EDGE ( 'NONE', *, *, #6211, .F. ) ;
#18098 = CARTESIAN_POINT ( 'NONE',  ( 27.16883889988623935, 56.57500000273117990, -19.73931689729374384 ) ) ;
#18099 = CARTESIAN_POINT ( 'NONE',  ( -10.04305231718579172, 4.100000005462373309, -30.90933677959248982 ) ) ;
#18100 = CARTESIAN_POINT ( 'NONE',  ( 26.09010956794232428, 38.64621500092395934, -6.950374756619718042 ) ) ;
#18101 = CARTESIAN_POINT ( 'NONE',  ( 6.486482029760649416E-15, 77.87500000273118417, 35.31076352940723240 ) ) ;
#18102 = ORIENTED_EDGE ( 'NONE', *, *, #28135, .T. ) ;
#18103 = CARTESIAN_POINT ( 'NONE',  ( -27.16883889988623935, 27.32500000273117990, 19.73931689729374739 ) ) ;
#18104 = CARTESIAN_POINT ( 'NONE',  ( 26.00068869287340334, 16.44010416666666430, -15.01150461594642316 ) ) ;
#18105 = ORIENTED_EDGE ( 'NONE', *, *, #1363, .T. ) ;
#18106 = CARTESIAN_POINT ( 'NONE',  ( 0.000000000000000000, 66.99999999999998579, 0.000000000000000000 ) ) ;
#18107 = CARTESIAN_POINT ( 'NONE',  ( -20.75514604977248112, 59.42500000273118843, 28.56700777964554661 ) ) ;
#18108 = CARTESIAN_POINT ( 'NONE',  ( -28.01184896238290278, 35.48958333333332860, 7.505752307973363457 ) ) ;
#18109 =( BOUNDED_CURVE ( )  B_SPLINE_CURVE ( 2, ( #12263, #17949, #33190, #25313, #22913, #20523, #30792, #28398, #20699, #2137, #12956, #7466, #18114 ),
 .UNSPECIFIED., .F., .T. ) 
 B_SPLINE_CURVE_WITH_KNOTS ( ( 3, 2, 2, 2, 2, 2, 3 ),
 ( 0.6474358974358974672, 0.6487179487179487447, 0.6512820512820512997, 0.6538461538461538547, 0.6564102564102564097, 0.6589743589743589647, 0.6602564102564102422 ),
 .UNSPECIFIED. ) 
 CURVE ( )  GEOMETRIC_REPRESENTATION_ITEM ( )  RATIONAL_B_SPLINE_CURVE ( ( 0.9755282581475768211, 0.9755282581475768211, 1.000000000000000000, 0.9510565162951535312, 1.000000000000000000, 0.9510565162951535312, 1.000000000000000000, 0.9510565162951535312, 1.000000000000000000, 0.9510565162951535312, 1.000000000000000000, 0.9755282581475768211, 0.9755282581475768211 ) ) 
 REPRESENTATION_ITEM ( '' )  );
#18110 = CARTESIAN_POINT ( 'NONE',  ( 15.14183272437242245, 16.30000000000001137, -20.84094480462497856 ) ) ;
#18111 = DIRECTION ( 'NONE',  ( 0.000000000000000000, 0.000000000000000000, -1.000000000000000000 ) ) ;
#18112 = CARTESIAN_POINT ( 'NONE',  ( -33.58253175000000113, 3.225000002731193138, 10.91162601494193929 ) ) ;
#18113 =( BOUNDED_CURVE ( )  B_SPLINE_CURVE ( 2, ( #29659, #999, #6162, #21795, #13732, #32074, #3103, #670, #3428, #3593, #11158, #29495, #24202 ),
 .UNSPECIFIED., .F., .T. ) 
 B_SPLINE_CURVE_WITH_KNOTS ( ( 3, 2, 2, 2, 2, 2, 3 ),
 ( 0.2115384615384615363, 0.2128205128205128138, 0.2153846153846153966, 0.2179487179487179516, 0.2205128205128205066, 0.2230769230769230893, 0.2243589743589743668 ),
 .UNSPECIFIED. ) 
 CURVE ( )  GEOMETRIC_REPRESENTATION_ITEM ( )  RATIONAL_B_SPLINE_CURVE ( ( 0.9755282581475768211, 0.9755282581475768211, 1.000000000000000000, 0.9510565162951535312, 1.000000000000000000, 0.9510565162951535312, 1.000000000000000000, 0.9510565162951535312, 1.000000000000000000, 0.9510565162951535312, 1.000000000000000000, 0.9755282581475768211, 0.9755282581475768211 ) ) 
 REPRESENTATION_ITEM ( '' )  );
#18114 = CARTESIAN_POINT ( 'NONE',  ( 5.779280353836490358E-15, 28.50000000000000355, 32.49999999999999289 ) ) ;
#18115 = CARTESIAN_POINT ( 'NONE',  ( 20.47846945139867003, 62.98399333240935505, -20.53372385742107653 ) ) ;
#18116 = CARTESIAN_POINT ( 'NONE',  ( 7.313012447739250820E-14, 15.50000000000000178, 24.50000000000000000 ) ) ;
#18117 = CARTESIAN_POINT ( 'NONE',  ( -26.00068869287368756, 63.41927083333333570, -15.01150461594595775 ) ) ;
#18118 = CARTESIAN_POINT ( 'NONE',  ( 32.50000000000000000, 9.000000000000007105, -3.980102097228898626E-15 ) ) ;
#18119 = CARTESIAN_POINT ( 'NONE',  ( 26.29305231718578995, 19.20000000000000995, -19.10302069950538240 ) ) ;
#18120 = CARTESIAN_POINT ( 'NONE',  ( -2.428612866367529427E-13, 63.99218749999997868, -27.95245687107223276 ) ) ;
#18121 = EDGE_CURVE ( 'NONE', #10457, #25891, #33750, .T. ) ;
#18122 = EDGE_CURVE ( 'NONE', #16826, #726, #21877, .T. ) ;
#18123 = CARTESIAN_POINT ( 'NONE',  ( 15.14183272437241889, 13.44999999453762385, 20.84094480462498211 ) ) ;
#18124 = CARTESIAN_POINT ( 'NONE',  ( -9.657523855033125146E-16, 73.75000000546238255, -15.77193336357400710 ) ) ;
#18125 = CARTESIAN_POINT ( 'NONE',  ( 24.20753774853756113, 23.88802083333331794, 13.97622843553589789 ) ) ;
#18126 = CARTESIAN_POINT ( 'NONE',  ( -20.75514604977248823, 28.82500000273116569, -28.56700777964554305 ) ) ;
#18127 = PRODUCT ( 'BR-007', 'BR-007', '', ( #30705 ) ) ;
#18128 = CARTESIAN_POINT ( 'NONE',  ( 33.58253175000000823, 78.02500000273118985, 10.91162601494192863 ) ) ;
#18129 = ADVANCED_BREP_SHAPE_REPRESENTATION ( '', ( #9431, #1376 ), #23828 ) ;
#18130 = CARTESIAN_POINT ( 'NONE',  ( 20.75514604977248467, 34.67500000273118843, -28.56700777964554305 ) ) ;
#18131 = CARTESIAN_POINT ( 'NONE',  ( 10.37757302488624056, 20.77500000273119340, -31.93888565452638417 ) ) ;
#18132 = CARTESIAN_POINT ( 'NONE',  ( -20.08610463437157989, 63.69999999999999574, -27.64615127144129758 ) ) ;
#18133 = CARTESIAN_POINT ( 'NONE',  ( -7.025853678916393008, 50.10454833425731636, 26.06988505166735592 ) ) ;
#18134 = CARTESIAN_POINT ( 'NONE',  ( 10.37757302488624767, 73.72500000273119269, 31.93888565452638417 ) ) ;
#18135 = CYLINDRICAL_SURFACE ( 'NONE', #5797, 32.50000000000000000 ) ;
#18136 = CARTESIAN_POINT ( 'NONE',  ( 32.50000000000000711, 62.89999999999999147, 10.55989012756945122 ) ) ;
#18137 = CARTESIAN_POINT ( 'NONE',  ( -7.236395654485757944, 17.22499999726881370, -22.27133577429736988 ) ) ;
#18138 = CARTESIAN_POINT ( 'NONE',  ( 10.37757302488624767, 63.72500000273117848, 31.93888565452638417 ) ) ;
#18139 = CARTESIAN_POINT ( 'NONE',  ( 18.94512977948575738, 8.924999997268812990, 13.76444248337723408 ) ) ;
#18140 = ADVANCED_FACE ( 'NONE', ( #5922 ), #19301, .F. ) ;
#18141 = CARTESIAN_POINT ( 'NONE',  ( -10.37757302488624411, 70.97500000273120691, -31.93888565452638417 ) ) ;
#18142 = CARTESIAN_POINT ( 'NONE',  ( 27.16883889988623935, 8.325000002731176352, -19.73931689729374384 ) ) ;
#18143 = CARTESIAN_POINT ( 'NONE',  ( 7.236395654485755280, 18.72499999726881370, 22.27133577429736988 ) ) ;
#18144 = CARTESIAN_POINT ( 'NONE',  ( -27.95245687107223986, 13.00819416759064318, -0.04044903254993292840 ) ) ;
#18145 = ORIENTED_EDGE ( 'NONE', *, *, #24987, .T. ) ;
#18146 = CARTESIAN_POINT ( 'NONE',  ( -27.16883889988623935, 45.32500000273119412, 19.73931689729374739 ) ) ;
#18147 = ORIENTED_EDGE ( 'NONE', *, *, #6732, .T. ) ;
#18148 = CARTESIAN_POINT ( 'NONE',  ( 2.740863092043355209E-13, 38.21093750000000000, 30.02300923189239512 ) ) ;
#18149 = DIRECTION ( 'NONE',  ( -1.224646799147353454E-16, 1.000000000000000000, -0.000000000000000000 ) ) ;
#18150 = CARTESIAN_POINT ( 'NONE',  ( -10.04305231718578462, 6.900000005462383790, 30.90933677959249337 ) ) ;
#18151 = DIRECTION ( 'NONE',  ( -0.7069718413157914938, -0.01953538259431466736, 0.7069718413158002646 ) ) ;
#18152 = CARTESIAN_POINT ( 'NONE',  ( 19.82091636218621034, 19.54999999453763238, 14.40073868116559730 ) ) ;
#18153 = CARTESIAN_POINT ( 'NONE',  ( -18.94512977948576093, 17.82499999726880446, 13.76444248337722698 ) ) ;
#18154 = CARTESIAN_POINT ( 'NONE',  ( -10.37757302488623701, 13.77500000273118630, 31.93888565452638417 ) ) ;
#18155 = CARTESIAN_POINT ( 'NONE',  ( -32.50000000000000000, 16.60000000546238752, 10.55989012756946366 ) ) ;
#18156 = CARTESIAN_POINT ( 'NONE',  ( 32.50000000000000711, 68.90000000000001990, 10.55989012756945122 ) ) ;
#18157 = CARTESIAN_POINT ( 'NONE',  ( 15.00000000000000000, 77.25000000546239676, -1.836970198721029589E-15 ) ) ;
#18158 = CARTESIAN_POINT ( 'NONE',  ( 1.555960095263670572E-15, 12.50000000000000355, -24.50000000000000000 ) ) ;
#18159 = CARTESIAN_POINT ( 'NONE',  ( -20.50609665441004736, 11.99999999999999645, -20.50609665440969565 ) ) ;
#18160 = CARTESIAN_POINT ( 'NONE',  ( 8.601468415847516980, 80.67500000273116711, -11.83890561707634781 ) ) ;
#18161 = CARTESIAN_POINT ( 'NONE',  ( -15.01150461594642316, 36.20572916666665719, -26.00068869287341045 ) ) ;
#18162 = APPLICATION_PROTOCOL_DEFINITION ( 'draft international standard', 'automotive_design', 1998, #20187 ) ;
#18163 = CARTESIAN_POINT ( 'NONE',  ( 0.000000000000000000, 0.000000000000000000, 24.50000000000000000 ) ) ;
#18164 = CARTESIAN_POINT ( 'NONE',  ( 7.236395654485755280, 16.72499999726881370, 22.27133577429736988 ) ) ;
#18165 = CARTESIAN_POINT ( 'NONE',  ( 6.277390505771533514E-15, 8.499999999999992895, 34.17252228774368916 ) ) ;
#18166 = CARTESIAN_POINT ( 'NONE',  ( -12.13525491562420910, 74.19999999999998863, 8.816778784387098611 ) ) ;
#18167 = CARTESIAN_POINT ( 'NONE',  ( 26.06988505166722803, 49.52045166574269075, -7.025853678916862854 ) ) ;
#18168 = CARTESIAN_POINT ( 'NONE',  ( 33.58253175000000113, 50.12500000273117706, -4.112674001490185761E-15 ) ) ;
#18169 = CARTESIAN_POINT ( 'NONE',  ( 6.486482029760649416E-15, 55.87500000273118417, 35.31076352940723240 ) ) ;
#18170 = CARTESIAN_POINT ( 'NONE',  ( 27.16883889988624290, 38.17500000273118843, 19.73931689729373673 ) ) ;
#18171 = DIRECTION ( 'NONE',  ( 0.000000000000000000, 0.000000000000000000, -1.000000000000000000 ) ) ;
#18172 = DIRECTION ( 'NONE',  ( 0.000000000000000000, -1.000000000000000000, 0.000000000000000000 ) ) ;
#18173 = CARTESIAN_POINT ( 'NONE',  ( -13.91746824999999887, 81.12500000273121259, 0.000000000000000000 ) ) ;
#18174 = CARTESIAN_POINT ( 'NONE',  ( 5.204170427930421283E-15, -70.99969134886156041, 0.000000000000000000 ) ) ;
#18175 = CARTESIAN_POINT ( 'NONE',  ( 32.50000000000000000, 79.00000000000000000, -3.980102097228898626E-15 ) ) ;
#18176 = CARTESIAN_POINT ( 'NONE',  ( 33.58253175000000113, 18.12500000273119127, -4.112674001490185761E-15 ) ) ;
#18177 = CARTESIAN_POINT ( 'NONE',  ( 0.000000000000000000, 86.00000000000001421, 0.000000000000000000 ) ) ;
#18178 = CARTESIAN_POINT ( 'NONE',  ( -15.00000000000000000, 80.25000000546239676, 0.000000000000000000 ) ) ;
#18179 = EDGE_CURVE ( 'NONE', #30438, #14163, #16730, .T. ) ;
#18180 = CARTESIAN_POINT ( 'NONE',  ( 4.023268246324634798E-14, 10.24999999453763166, -24.50000000000000355 ) ) ;
#18181 = CARTESIAN_POINT ( 'NONE',  ( 6.950374756619257965, 21.44753499907601579, -26.09010956794244507 ) ) ;
#18182 = CARTESIAN_POINT ( 'NONE',  ( -32.50000000000000000, 36.60000000546239818, 10.55989012756946366 ) ) ;
#18183 = CARTESIAN_POINT ( 'NONE',  ( 24.50000000000000000, 17.74999999453763522, 0.000000000000000000 ) ) ;
#18184 = CARTESIAN_POINT ( 'NONE',  ( 20.75514604977248467, 28.42500000273118133, -28.56700777964554305 ) ) ;
#18185 = AXIS2_PLACEMENT_3D ( 'NONE', #28953, #10093, #13006 ) ;
#18186 = CARTESIAN_POINT ( 'NONE',  ( 24.20753774853756113, 41.07552083333331439, 13.97622843553589789 ) ) ;
#18187 = EDGE_CURVE ( 'NONE', #13703, #7411, #23786, .T. ) ;
#18188 = ORIENTED_EDGE ( 'NONE', *, *, #33695, .F. ) ;
#18189 = CARTESIAN_POINT ( 'NONE',  ( 6.486482029760649416E-15, 63.62500000273117706, 35.31076352940723240 ) ) ;
#18190 = CARTESIAN_POINT ( 'NONE',  ( -7.505752307972844761, 45.22916666666665719, 28.01184896238304134 ) ) ;
#18191 = EDGE_LOOP ( 'NONE', ( #8123, #13705, #22860, #14984, #24168, #2808, #25582, #15863, #17544, #33715 ) ) ;
#18192 = CARTESIAN_POINT ( 'NONE',  ( 28.01184896238290278, 13.14583333333332860, -7.505752307973347470 ) ) ;
#18193 = CARTESIAN_POINT ( 'NONE',  ( 20.47846945139902530, 18.59413166759064140, 20.53372385742071771 ) ) ;
#18194 = CARTESIAN_POINT ( 'NONE',  ( 10.37757302488624767, 5.725000002731183812, 31.93888565452638417 ) ) ;
#18195 = EDGE_CURVE ( 'NONE', #21689, #7536, #5471, .T. ) ;
#18196 = CARTESIAN_POINT ( 'NONE',  ( -1.778240108872766143E-15, 45.49999999999999289, -32.49999999999999289 ) ) ;
#18197 = CARTESIAN_POINT ( 'NONE',  ( 6.486482029760649416E-15, 37.87500000273117706, 35.31076352940723240 ) ) ;
#18198 = CARTESIAN_POINT ( 'NONE',  ( 20.08610463437157279, 37.80000000546239391, -27.64615127144129758 ) ) ;
#18199 = CARTESIAN_POINT ( 'NONE',  ( 12.13525491562420910, 75.19999999999998863, -8.816778784387098611 ) ) ;
#18200 = CARTESIAN_POINT ( 'NONE',  ( -32.50000000000000000, 47.99999999999998579, 0.000000000000000000 ) ) ;
#18201 = CARTESIAN_POINT ( 'NONE',  ( 20.75514604977249178, 21.82500000273119056, 28.56700777964553950 ) ) ;
#18202 = DIRECTION ( 'NONE',  ( -0.8660254037844387076, 0.000000000000000000, -0.4999999999999998335 ) ) ;
#18203 = CARTESIAN_POINT ( 'NONE',  ( 27.16883889988624290, 52.17500000273117422, 19.73931689729373673 ) ) ;
#18204 = FILL_AREA_STYLE_COLOUR ( '', #24355 ) ;
#18205 = CARTESIAN_POINT ( 'NONE',  ( 32.50000000000000000, 31.10000000000000497, -10.55989012756945833 ) ) ;
#18206 = CARTESIAN_POINT ( 'NONE',  ( 10.04305231718579705, 30.60000000000001563, 30.90933677959248982 ) ) ;
#18207 = CARTESIAN_POINT ( 'NONE',  ( -19.82091636218621389, 5.200000000000009948, 14.40073868116558842 ) ) ;
#18208 = CARTESIAN_POINT ( 'NONE',  ( -10.37757302488624411, 70.72500000273119269, -31.93888565452638417 ) ) ;
#18209 = CARTESIAN_POINT ( 'NONE',  ( -26.02353298184806007, 67.00000000000000000, 20.33883978280647398 ) ) ;
#18210 = MECHANICAL_DESIGN_GEOMETRIC_PRESENTATION_REPRESENTATION (  '', ( #17088 ), #22563 ) ;
#18211 = CARTESIAN_POINT ( 'NONE',  ( -26.29305231718578995, 38.20000000000000995, 19.10302069950538595 ) ) ;
#18212 = CARTESIAN_POINT ( 'NONE',  ( 33.58253175000000113, 62.37500000273119127, -4.112674001490185761E-15 ) ) ;
#18213 = CARTESIAN_POINT ( 'NONE',  ( 0.000000000000000000, 80.00000000000001421, 0.000000000000000000 ) ) ;
#18214 = CARTESIAN_POINT ( 'NONE',  ( 33.58253175000000113, 10.22500000273117671, -10.91162601494193751 ) ) ;
#18215 = CARTESIAN_POINT ( 'NONE',  ( 24.18731323226247554, 28.76340250092398065, 14.01125832528285997 ) ) ;
#18216 =( BOUNDED_CURVE ( )  B_SPLINE_CURVE ( 2, ( #9270, #30547, #12542, #33468, #33296, #28325, #9968, #22836, #14608, #27986, #30372, #4473, #15123 ),
 .UNSPECIFIED., .F., .T. ) 
 B_SPLINE_CURVE_WITH_KNOTS ( ( 3, 2, 2, 2, 2, 2, 3 ),
 ( 0.6858974358974359031, 0.6871794871794871806, 0.6897435897435897356, 0.6923076923076922906, 0.6948717948717948456, 0.6974358974358974006, 0.6987179487179486781 ),
 .UNSPECIFIED. ) 
 CURVE ( )  GEOMETRIC_REPRESENTATION_ITEM ( )  RATIONAL_B_SPLINE_CURVE ( ( 0.9755282581475768211, 0.9755282581475768211, 1.000000000000000000, 0.9510565162951535312, 1.000000000000000000, 0.9510565162951535312, 1.000000000000000000, 0.9510565162951535312, 1.000000000000000000, 0.9510565162951535312, 1.000000000000000000, 0.9755282581475768211, 0.9755282581475768211 ) ) 
 REPRESENTATION_ITEM ( '' )  );
#18217 = CARTESIAN_POINT ( 'NONE',  ( 24.50000000000000000, 1.749999994537621006, 0.000000000000000000 ) ) ;
#18218 = CARTESIAN_POINT ( 'NONE',  ( 20.75514604977249178, 2.075000002731171467, 28.56700777964553950 ) ) ;
#18219 = CARTESIAN_POINT ( 'NONE',  ( 27.16883889988623935, 32.32500000273117990, -19.73931689729374384 ) ) ;
#18220 = CARTESIAN_POINT ( 'NONE',  ( 32.50000000000000000, 45.60000000546236265, -10.55989012756945833 ) ) ;
#18221 = CARTESIAN_POINT ( 'NONE',  ( 5.147494310547426899, 19.44874571845315003, -32.50000000000000000 ) ) ;
#18222 = CARTESIAN_POINT ( 'NONE',  ( -8.601468415847518756, 78.57500000273120122, -11.83890561707634603 ) ) ;
#18223 = CARTESIAN_POINT ( 'NONE',  ( -7.468012846824272799, 50.66628499907601935, 28.02196122052058413 ) ) ;
#18224 = CARTESIAN_POINT ( 'NONE',  ( -26.29305231718579350, 56.30000000546238681, -19.10302069950537884 ) ) ;
#18225 = CARTESIAN_POINT ( 'NONE',  ( 4.300734207923761154, 79.97500000273122112, 13.23629886949340495 ) ) ;
#18226 = CARTESIAN_POINT ( 'NONE',  ( 6.988114217768294445, 14.00520833333333215, 26.07999730980477437 ) ) ;
#18227 = CARTESIAN_POINT ( 'NONE',  ( -20.08610463437156923, 54.30000000000000426, 27.64615127144130113 ) ) ;
#18228 = CARTESIAN_POINT ( 'NONE',  ( 26.29305231718579350, 71.30000000546237970, 19.10302069950537529 ) ) ;
#18229 = CARTESIAN_POINT ( 'NONE',  ( -26.00068869287368756, 22.16927083333332504, -15.01150461594595775 ) ) ;
#18230 = CARTESIAN_POINT ( 'NONE',  ( 6.486482029760649416E-15, 35.87500000273118417, 35.31076352940723240 ) ) ;
#18231 = CARTESIAN_POINT ( 'NONE',  ( 7.236395654485760609, 5.524999997268825958, -22.27133577429736633 ) ) ;
#18232 = ORIENTED_EDGE ( 'NONE', *, *, #30542, .F. ) ;
#18233 = CARTESIAN_POINT ( 'NONE',  ( -7.543491769121417612, 43.22954833425730925, 28.00173670424549499 ) ) ;
#18234 = CARTESIAN_POINT ( 'NONE',  ( -20.08610463437156923, 20.80000000546236549, 27.64615127144130113 ) ) ;
#18235 = CARTESIAN_POINT ( 'NONE',  ( -28.01184896238304134, 39.21354166666666430, -7.505752307972844761 ) ) ;
#18236 = CARTESIAN_POINT ( 'NONE',  ( -26.00068869287340334, 62.84635416666667851, 15.01150461594643382 ) ) ;
#18237 = CARTESIAN_POINT ( 'NONE',  ( -10.37757302488624411, 50.97500000273119980, -31.93888565452638417 ) ) ;
#18238 = CARTESIAN_POINT ( 'NONE',  ( -26.29305231718579350, 58.30000000546237260, -19.10302069950537884 ) ) ;
#18239 = DIRECTION ( 'NONE',  ( -1.224646799147353454E-16, 1.000000000000000000, -0.000000000000000000 ) ) ;
#18240 = CARTESIAN_POINT ( 'NONE',  ( 33.58253175000000113, 42.22500000273118559, -10.91162601494193751 ) ) ;
#18241 = CARTESIAN_POINT ( 'NONE',  ( 2.445080149700053643E-15, 72.50000000000001421, 15.00000000000000000 ) ) ;
#18242 = CARTESIAN_POINT ( 'NONE',  ( -33.58253175000000113, 65.37500000273119838, 0.000000000000000000 ) ) ;
#18243 = CARTESIAN_POINT ( 'NONE',  ( -1.778240108872766143E-15, 22.00000000546237899, -32.49999999999999289 ) ) ;
#18244 = CARTESIAN_POINT ( 'NONE',  ( -20.75514604977248112, 63.42500000273118843, 28.56700777964554661 ) ) ;
#18245 = CARTESIAN_POINT ( 'NONE',  ( -26.00068869287368756, 18.73177083333332504, -15.01150461594595775 ) ) ;
#18246 = CARTESIAN_POINT ( 'NONE',  ( -10.04305231718578462, 46.39999999999999858, 30.90933677959249337 ) ) ;
#18247 = CARTESIAN_POINT ( 'NONE',  ( 23.41746825000000243, 2.724999997268822138, -7.608796670333727974 ) ) ;
#18248 = CARTESIAN_POINT ( 'NONE',  ( 33.58253175000000113, 10.47500000273119802, -10.91162601494193751 ) ) ;
#18249 = CARTESIAN_POINT ( 'NONE',  ( 0.000000000000000000, 80.00000000000001421, 0.000000000000000000 ) ) ;
#18250 = CARTESIAN_POINT ( 'NONE',  ( 26.09010956794244507, 36.05690999907600514, 6.950374756619249084 ) ) ;
#18251 = CARTESIAN_POINT ( 'NONE',  ( -4.300734207923759378, 80.97500000273119269, -13.23629886949340495 ) ) ;
#18252 = CARTESIAN_POINT ( 'NONE',  ( -2.162160676586882350E-15, 78.87500000273118417, -35.31076352940722529 ) ) ;
#18253 = DIRECTION ( 'NONE',  ( -0.000000000000000000, -1.000000000000000000, -0.000000000000000000 ) ) ;
#18254 = VECTOR ( 'NONE', #26959, 1000.000000000000000 ) ;
#18255 = CARTESIAN_POINT ( 'NONE',  ( 10.37757302488624056, 76.77500000273117564, -31.93888565452638417 ) ) ;
#18256 = ORIENTED_EDGE ( 'NONE', *, *, #27274, .T. ) ;
#18257 = CARTESIAN_POINT ( 'NONE',  ( -23.41746825000000598, 16.22499999726880304, 7.608796670333726198 ) ) ;
#18258 = CARTESIAN_POINT ( 'NONE',  ( -13.97622843553588901, 59.12239583333333570, 24.20753774853756823 ) ) ;
#18259 = CARTESIAN_POINT ( 'NONE',  ( -20.75514604977248823, 54.82500000273118701, -28.56700777964554305 ) ) ;
#18260 = CARTESIAN_POINT ( 'NONE',  ( -2.162160676586881955E-15, 16.87500000273120193, -35.31076352940723240 ) ) ;
#18261 = CARTESIAN_POINT ( 'NONE',  ( -33.58253175000000113, 79.02500000273118985, -10.91162601494193218 ) ) ;
#18262 = CARTESIAN_POINT ( 'NONE',  ( 19.09188309203661049, 36.92187499999999289, -19.09188309203694445 ) ) ;
#18263 = CARTESIAN_POINT ( 'NONE',  ( 20.47846945139902530, 32.34413166759064495, 20.53372385742071771 ) ) ;
#18264 = CARTESIAN_POINT ( 'NONE',  ( 20.47846945139867003, 18.29649333240935150, -20.53372385742107653 ) ) ;
#18265 = CARTESIAN_POINT ( 'NONE',  ( 32.50000000000000000, 73.50000000546238255, -3.980102097228898626E-15 ) ) ;
#18266 = CARTESIAN_POINT ( 'NONE',  ( 31.53731130704408869, 52.00000000000002132, 11.55439184653631024 ) ) ;
#18267 = CARTESIAN_POINT ( 'NONE',  ( -20.75514604977248112, 43.42500000273117422, 28.56700777964554661 ) ) ;
#18268 = CARTESIAN_POINT ( 'NONE',  ( -14.47279130897152122, 7.924999997268803220, 19.92008829642072243 ) ) ;
#18269 = CARTESIAN_POINT ( 'NONE',  ( -32.50000000000000000, 2.400000005462369579, -10.55989012756945300 ) ) ;
#18270 = ORIENTED_EDGE ( 'NONE', *, *, #23296, .F. ) ;
#18271 = EDGE_CURVE ( 'NONE', #5086, #15743, #12547, .T. ) ;
#18272 = CARTESIAN_POINT ( 'NONE',  ( 6.486482029760649416E-15, 55.87500000273118417, 35.31076352940723240 ) ) ;
#18273 = CARTESIAN_POINT ( 'NONE',  ( 2.445080149700053643E-15, 70.75000000546236834, 15.00000000000000000 ) ) ;
#18274 = AXIS2_PLACEMENT_3D ( 'NONE', #14072, #10262, #33771 ) ;
#18275 = CARTESIAN_POINT ( 'NONE',  ( -27.95245687107223986, 40.50819416759064495, -0.04044903254993292840 ) ) ;
#18276 = CARTESIAN_POINT ( 'NONE',  ( -27.16883889988623935, 75.57500000273120122, 19.73931689729374739 ) ) ;
#18277 = EDGE_CURVE ( 'NONE', #14369, #21231, #8963, .T. ) ;
#18278 = VERTEX_POINT ( 'NONE', #23018 ) ;
#18279 = CARTESIAN_POINT ( 'NONE',  ( -10.37757302488624411, 26.72500000273118914, -31.93888565452638417 ) ) ;
#18280 = VECTOR ( 'NONE', #21491, 1000.000000000000114 ) ;
#18281 = CARTESIAN_POINT ( 'NONE',  ( -30.02300923189239512, 18.44531249999999645, 2.654126918244515359E-13 ) ) ;
#18282 = ORIENTED_EDGE ( 'NONE', *, *, #21442, .T. ) ;
#18283 = CARTESIAN_POINT ( 'NONE',  ( -20.08610463437156923, 58.29999999999999716, 27.64615127144130113 ) ) ;
#18284 = CARTESIAN_POINT ( 'NONE',  ( 33.58253175000000113, 60.22500000273119980, -10.91162601494193751 ) ) ;
#18285 = CARTESIAN_POINT ( 'NONE',  ( 30.02300923189239512, 47.66406249999998579, -2.619432448724977703E-13 ) ) ;
#18286 = CARTESIAN_POINT ( 'NONE',  ( -3.880418787951124493, 7.198745712990782586, 24.50000000000000355 ) ) ;
#18287 = CARTESIAN_POINT ( 'NONE',  ( -7.236395654485763274, 2.524999997268823293, 22.27133577429736633 ) ) ;
#18288 = CARTESIAN_POINT ( 'NONE',  ( -2.162160676586881955E-15, 6.625000002731173510, -35.31076352940723240 ) ) ;
#18289 = CARTESIAN_POINT ( 'NONE',  ( -9.270509831248419985, 78.55000000546236549, 12.75976212528060039 ) ) ;
#18290 = CARTESIAN_POINT ( 'NONE',  ( 20.47846945139867003, 59.54649333240936215, -20.53372385742107653 ) ) ;
#18291 = CARTESIAN_POINT ( 'NONE',  ( 1.836970198721029589E-15, 70.00000000000000000, 15.00000000000000000 ) ) ;
#18292 = CARTESIAN_POINT ( 'NONE',  ( 15.00000000000000000, 81.00000000000001421, -1.836970198721029589E-15 ) ) ;
#18293 = CARTESIAN_POINT ( 'NONE',  ( -5.147494310547423346, 60.44874571845313227, 32.50000000000000000 ) ) ;
#18294 = CARTESIAN_POINT ( 'NONE',  ( -26.29305231718578995, 14.20000000000000462, 19.10302069950538595 ) ) ;
#18295 = CARTESIAN_POINT ( 'NONE',  ( 19.09188309203694800, 58.40625000000000711, 19.09188309203660694 ) ) ;
#18296 = CARTESIAN_POINT ( 'NONE',  ( -19.82091636218621389, 14.94999999453763806, 14.40073868116558842 ) ) ;
#18297 = CARTESIAN_POINT ( 'NONE',  ( 11.25946833292375793, 79.67500000273119554, 8.180482586598731842 ) ) ;
#18298 = CARTESIAN_POINT ( 'NONE',  ( 19.09188309203661049, 33.48437500000000000, -19.09188309203694445 ) ) ;
#18299 = CARTESIAN_POINT ( 'NONE',  ( -33.58253175000000113, 33.12500000273119127, 0.000000000000000000 ) ) ;
#18300 = CARTESIAN_POINT ( 'NONE',  ( -20.75514604977248112, 73.42500000273118133, 28.56700777964554661 ) ) ;
#18301 = CARTESIAN_POINT ( 'NONE',  ( 6.486482029760649416E-15, 35.87500000273118417, 35.31076352940723240 ) ) ;
#18302 = CARTESIAN_POINT ( 'NONE',  ( -2.162160676586882350E-15, 16.87500000273119483, -35.31076352940722529 ) ) ;
#18303 = DIRECTION ( 'NONE',  ( -1.000000000000000000, 0.000000000000000000, 0.000000000000000000 ) ) ;
#18304 = CARTESIAN_POINT ( 'NONE',  ( 27.95245687107223986, 49.10194416759064495, 0.04044903254993640479 ) ) ;
#18305 = CIRCLE ( 'NONE', #3484, 0.9999999999999988898 ) ;
#18306 = CARTESIAN_POINT ( 'NONE',  ( -27.16883889988623935, 73.32500000273117280, 19.73931689729374739 ) ) ;
#18307 = CARTESIAN_POINT ( 'NONE',  ( -32.50000000000000000, 26.60000000546239107, 10.55989012756946366 ) ) ;
#18308 = CARTESIAN_POINT ( 'NONE',  ( -26.29305231718579350, 57.80000000000000426, -19.10302069950537884 ) ) ;
#18309 = FACE_BOUND ( 'NONE', #21270, .T. ) ;
#18310 = CARTESIAN_POINT ( 'NONE',  ( -27.16883889988624290, 64.92500000273118133, -19.73931689729374028 ) ) ;
#18311 = CARTESIAN_POINT ( 'NONE',  ( -14.47279130897151589, 5.824999997268811569, -19.92008829642072598 ) ) ;
#18312 = EDGE_CURVE ( 'NONE', #19445, #11212, #33473, .T. ) ;
#18313 = CARTESIAN_POINT ( 'NONE',  ( 6.486482029760649416E-15, 75.87500000273119838, 35.31076352940723240 ) ) ;
#18314 = CARTESIAN_POINT ( 'NONE',  ( -10.37757302488623701, 9.525000002731182747, 31.93888565452638417 ) ) ;
#18315 = CARTESIAN_POINT ( 'NONE',  ( -14.47279130897151589, 1.324999997268808238, -19.92008829642072598 ) ) ;
#18316 = CARTESIAN_POINT ( 'NONE',  ( -6.950374756619716266, 13.72434000092397532, -26.09010956794232428 ) ) ;
#18317 = ORIENTED_EDGE ( 'NONE', *, *, #17404, .F. ) ;
#18318 = CARTESIAN_POINT ( 'NONE',  ( 33.58253175000000113, 46.12500000273119127, -4.112674001490185761E-15 ) ) ;
#18319 = ORIENTED_EDGE ( 'NONE', *, *, #13461, .T. ) ;
#18320 = CARTESIAN_POINT ( 'NONE',  ( 20.50609665440969565, 40.35937499999999289, -20.50609665441004736 ) ) ;
#18321 = CARTESIAN_POINT ( 'NONE',  ( 15.14183272437242422, 10.29999999999999361, -20.84094480462497856 ) ) ;
#18322 = CARTESIAN_POINT ( 'NONE',  ( 32.50000000000000000, 1.600000005462365760, -10.55989012756945833 ) ) ;
#18323 = CARTESIAN_POINT ( 'NONE',  ( -10.37757302488623701, 77.52500000273118985, 31.93888565452638417 ) ) ;
#18324 = CARTESIAN_POINT ( 'NONE',  ( -2.584737979205441561E-13, 22.74218749999999645, -30.02300923189239512 ) ) ;
#18325 = AXIS2_PLACEMENT_3D ( 'NONE', #16183, #31444, #31273 ) ;
#18326 = CARTESIAN_POINT ( 'NONE',  ( -15.14183272437242600, 1.299999999999988054, 20.84094480462497856 ) ) ;
#18327 = CARTESIAN_POINT ( 'NONE',  ( 6.486482029760649416E-15, 15.87500000273120015, 35.31076352940723240 ) ) ;
#18328 = CARTESIAN_POINT ( 'NONE',  ( -32.50000000000000000, 60.09999999999999432, 10.55989012756946366 ) ) ;
#18329 = CARTESIAN_POINT ( 'NONE',  ( -1.778240108872766143E-15, 58.00000000546237544, -32.49999999999999289 ) ) ;
#18330 = CARTESIAN_POINT ( 'NONE',  ( -32.63512777199724724, -24.47487373415291501, 0.000000000000000000 ) ) ;
#18331 = CARTESIAN_POINT ( 'NONE',  ( -14.97647472619899389, 33.62201416574269075, 26.02091320914878025 ) ) ;
#18332 = CARTESIAN_POINT ( 'NONE',  ( 8.601468415847520532, 78.07500000273117280, 11.83890561707634781 ) ) ;
#18333 = CARTESIAN_POINT ( 'NONE',  ( 2.740863092043355209E-13, 41.64843749999999289, 30.02300923189239867 ) ) ;
#18334 = LINE ( 'NONE', #28605, #20667 ) ;
#18335 = CARTESIAN_POINT ( 'NONE',  ( 3.880418787951178228, 16.44874571845315359, -24.49999999999998224 ) ) ;
#18336 = CARTESIAN_POINT ( 'NONE',  ( -2.092463501923844636E-15, 9.499999999999991118, -34.17252228774368916 ) ) ;
#18337 = CARTESIAN_POINT ( 'NONE',  ( 26.29305231718578995, 17.70000000546237473, -19.10302069950538240 ) ) ;
#18338 = CARTESIAN_POINT ( 'NONE',  ( 0.04044903255044120238, 53.96055583240936926, 27.95245687107223276 ) ) ;
#18339 = CARTESIAN_POINT ( 'NONE',  ( -20.75514604977248823, 48.82500000273117280, -28.56700777964554305 ) ) ;
#18340 = CARTESIAN_POINT ( 'NONE',  ( 10.37757302488624767, 53.97500000273118559, 31.93888565452638417 ) ) ;
#18341 = CARTESIAN_POINT ( 'NONE',  ( 20.75514604977248467, 38.67500000273116711, -28.56700777964554305 ) ) ;
#18342 = CARTESIAN_POINT ( 'NONE',  ( -1.778240108872766143E-15, 24.00000000546237899, -32.49999999999999289 ) ) ;
#18343 = CARTESIAN_POINT ( 'NONE',  ( 24.20753774853731244, 16.44010416666666430, -13.97622843553633132 ) ) ;
#18344 = DIRECTION ( 'NONE',  ( -0.8660254037844399289, -0.4999999999999977240, 0.000000000000000000 ) ) ;
#18345 =( GEOMETRIC_REPRESENTATION_CONTEXT ( 3 ) GLOBAL_UNCERTAINTY_ASSIGNED_CONTEXT ( ( #6159 ) ) GLOBAL_UNIT_ASSIGNED_CONTEXT ( ( #146, #20780, #33809 ) ) REPRESENTATION_CONTEXT ( 'NONE', 'WORKASPACE' ) );
#18346 = CARTESIAN_POINT ( 'NONE',  ( -26.29305231718578995, 22.70000000546237828, 19.10302069950538595 ) ) ;
#18347 = CARTESIAN_POINT ( 'NONE',  ( -32.50000000000000000, 78.10000000000000853, 10.55989012756946366 ) ) ;
#18348 = CARTESIAN_POINT ( 'NONE',  ( -27.16883889988624290, 14.92500000273118488, -19.73931689729374028 ) ) ;
#18349 = LINE ( 'NONE', #31201, #24289 ) ;
#18350 = CARTESIAN_POINT ( 'NONE',  ( -19.82091636218621034, 12.54999999453762527, -14.40073868116559552 ) ) ;
#18351 = CIRCLE ( 'NONE', #16689, 30.00000000000000000 ) ;
#18352 = CARTESIAN_POINT ( 'NONE',  ( -32.50000000000000000, 40.00000000000000711, 0.000000000000000000 ) ) ;
#18353 = CARTESIAN_POINT ( 'NONE',  ( 26.09010956794244507, 15.43190999907601935, 6.950374756619249084 ) ) ;
#18354 = CARTESIAN_POINT ( 'NONE',  ( 26.29305231718579350, 33.30000000546239391, 19.10302069950537529 ) ) ;
#18355 = CARTESIAN_POINT ( 'NONE',  ( 3.880418787951172011, 17.30125427608447097, 24.49999999999998579 ) ) ;
#18356 = CARTESIAN_POINT ( 'NONE',  ( -33.58253175000000113, 25.22500000273119625, 10.91162601494193929 ) ) ;
#18357 = CARTESIAN_POINT ( 'NONE',  ( 6.988114217767829928, 46.94791666666666430, -26.07999730980489872 ) ) ;
#18358 = PRODUCT_DEFINITION ( 'UNKNOWN', '', #9324, #31903 ) ;
#18359 = ORIENTED_EDGE ( 'NONE', *, *, #27039, .F. ) ;
#18360 = CARTESIAN_POINT ( 'NONE',  ( 33.58253175000000113, 62.22500000273119269, -10.91162601494193751 ) ) ;
#18361 = VERTEX_POINT ( 'NONE', #22841 ) ;
#18362 = CARTESIAN_POINT ( 'NONE',  ( 15.01150461594643204, 17.29947916666666430, 26.00068869287340334 ) ) ;
#18363 = CARTESIAN_POINT ( 'NONE',  ( 20.53372385742072481, 10.85975666759064318, -20.47846945139902175 ) ) ;
#18364 = CARTESIAN_POINT ( 'NONE',  ( 33.58253175000000113, 8.125000002731184168, -4.112674001490185761E-15 ) ) ;
#18365 = CYLINDRICAL_SURFACE ( 'NONE', #19042, 32.50000000000000000 ) ;
#18366 = CARTESIAN_POINT ( 'NONE',  ( -10.37757302488623701, 37.77500000273118275, 31.93888565452638417 ) ) ;
#18367 = STYLED_ITEM ( 'NONE', ( #15476 ), #32070 ) ;
#18368 = CARTESIAN_POINT ( 'NONE',  ( -32.50000000000000000, 40.40000000546239534, -10.55989012756945478 ) ) ;
#18369 = CARTESIAN_POINT ( 'NONE',  ( -10.04305231718579172, 75.59999999999999432, -30.90933677959248982 ) ) ;
#18370 = FACE_OUTER_BOUND ( 'NONE', #18698, .T. ) ;
#18371 = CARTESIAN_POINT ( 'NONE',  ( 10.37757302488624767, 21.72500000273119980, 31.93888565452638417 ) ) ;
#18372 = CARTESIAN_POINT ( 'NONE',  ( 8.891200544363830713E-16, 81.50000000000001421, -15.00000000000000000 ) ) ;
#18373 = CARTESIAN_POINT ( 'NONE',  ( -10.37757302488623701, 49.77500000273118985, 31.93888565452638417 ) ) ;
#18374 = CARTESIAN_POINT ( 'NONE',  ( -20.08610463437157989, 23.70000000000000639, -27.64615127144129758 ) ) ;
#18375 = CARTESIAN_POINT ( 'NONE',  ( 26.29305231718579350, 26.79999999999999005, 19.10302069950537529 ) ) ;
#18376 = CARTESIAN_POINT ( 'NONE',  ( 7.570916362186213000, 2.400000000000013234, -23.30088464923126423 ) ) ;
#18377 = CARTESIAN_POINT ( 'NONE',  ( -27.16883889988624290, 70.92500000273119554, -19.73931689729374028 ) ) ;
#18378 = CARTESIAN_POINT ( 'NONE',  ( 2.013924091267699445, 74.00000000000002842, -14.36055101182497040 ) ) ;
#18379 = CARTESIAN_POINT ( 'NONE',  ( -2.162160676586882350E-15, 62.87500000273120548, -35.31076352940722529 ) ) ;
#18380 = CARTESIAN_POINT ( 'NONE',  ( 5.334720326618300005E-14, 73.50000000000001421, -32.50000000000000000 ) ) ;
#18381 = CARTESIAN_POINT ( 'NONE',  ( 27.16883889988624290, 9.925000002731193760, 19.73931689729373673 ) ) ;
#18382 = CARTESIAN_POINT ( 'NONE',  ( -7.025853678916393008, 26.04204833425729859, 26.06988505166735592 ) ) ;
#18383 = CARTESIAN_POINT ( 'NONE',  ( 19.82091636218621389, 9.949999994537634507, -14.40073868116559197 ) ) ;
#18384 = CARTESIAN_POINT ( 'NONE',  ( 20.75514604977248467, 2.675000002731181770, -28.56700777964554305 ) ) ;
#18385 = CARTESIAN_POINT ( 'NONE',  ( -20.75514604977248823, 34.82500000273118701, -28.56700777964554305 ) ) ;
#18386 = CARTESIAN_POINT ( 'NONE',  ( -5.147494310547423346, 64.94874572391552192, 32.50000000000000000 ) ) ;
#18387 = LINE ( 'NONE', #28833, #19922 ) ;
#18388 = CARTESIAN_POINT ( 'NONE',  ( -13.91746824999999532, 78.97500000273117848, 4.522059556121122093 ) ) ;
#18389 = CARTESIAN_POINT ( 'NONE',  ( -30.02300923189239867, 47.94493083240935505, 0.04044903255044988294 ) ) ;
#18390 = CARTESIAN_POINT ( 'NONE',  ( -32.50000000000000000, 54.40000000546238823, -10.55989012756945478 ) ) ;
#18391 = CARTESIAN_POINT ( 'NONE',  ( -13.91746824999999887, 79.37500000273118417, 0.000000000000000000 ) ) ;
#18392 = DIRECTION ( 'NONE',  ( 0.000000000000000000, 0.000000000000000000, -1.000000000000000000 ) ) ;
#18393 = CARTESIAN_POINT ( 'NONE',  ( 24.20753774853731244, 19.87760416666666430, -13.97622843553632599 ) ) ;
#18394 = CARTESIAN_POINT ( 'NONE',  ( 10.04305231718579705, 63.10000000546239818, 30.90933677959248982 ) ) ;
#18395 = CARTESIAN_POINT ( 'NONE',  ( -32.50000000000000000, 70.40000000546237402, -10.55989012756945478 ) ) ;
#18396 = CARTESIAN_POINT ( 'NONE',  ( -7.505752307972844761, 24.60416666666666430, 28.01184896238304134 ) ) ;
#18397 = CARTESIAN_POINT ( 'NONE',  ( -27.16883889988623935, 25.57500000273120477, 19.73931689729374739 ) ) ;
#18398 = CARTESIAN_POINT ( 'NONE',  ( 23.41746824999999887, 15.12499999726882294, 0.000000000000000000 ) ) ;
#18399 = VERTEX_POINT ( 'NONE', #4648 ) ;
#18400 = CARTESIAN_POINT ( 'NONE',  ( -7.468012846824771955, 37.78684000092396644, -28.02196122052045624 ) ) ;
#18401 = CARTESIAN_POINT ( 'NONE',  ( 20.08610463437157279, 17.80000000546237615, -27.64615127144129758 ) ) ;
#18402 = EDGE_CURVE ( 'NONE', #23373, #28296, #12480, .T. ) ;
#18403 = CARTESIAN_POINT ( 'NONE',  ( -26.00068869287368756, 56.54427083333332149, -15.01150461594595775 ) ) ;
#18404 = CARTESIAN_POINT ( 'NONE',  ( 5.779280353836490358E-15, 36.49999999999998579, 32.49999999999999289 ) ) ;
#18405 = CARTESIAN_POINT ( 'NONE',  ( 20.75514604977248467, 56.67500000273119554, -28.56700777964554305 ) ) ;
#18406 = CARTESIAN_POINT ( 'NONE',  ( -10.04305231718579172, 58.10000000546239107, -30.90933677959248982 ) ) ;
#18407 = CARTESIAN_POINT ( 'NONE',  ( 0.000000000000000000, 0.000000000000000000, 0.000000000000000000 ) ) ;
#18408 = CARTESIAN_POINT ( 'NONE',  ( -2.162160676586881955E-15, 40.62500000273120548, -35.31076352940723240 ) ) ;
#18409 = DIRECTION ( 'NONE',  ( 0.000000000000000000, -1.000000000000000000, 0.000000000000000000 ) ) ;
#18410 = CARTESIAN_POINT ( 'NONE',  ( 20.75514604977249178, 68.07500000273118701, 28.56700777964553950 ) ) ;
#18411 = CARTESIAN_POINT ( 'NONE',  ( 5.779280353836490358E-15, 54.49999999999999289, 32.49999999999999289 ) ) ;
#18412 = CARTESIAN_POINT ( 'NONE',  ( 10.37757302488624056, 64.52500000273118985, -31.93888565452638417 ) ) ;
#18413 = EDGE_CURVE ( 'NONE', #29502, #14163, #677, .T. ) ;
#18414 = CARTESIAN_POINT ( 'NONE',  ( -26.00068869287340334, 25.03385416666666430, 15.01150461594643559 ) ) ;
#18415 = PRESENTATION_LAYER_ASSIGNMENT (  '', '', ( #1949 ) ) ;
#18416 = CARTESIAN_POINT ( 'NONE',  ( -26.29305231718579350, 43.80000000000000426, -19.10302069950537884 ) ) ;
#18417 = CARTESIAN_POINT ( 'NONE',  ( 18.94512977948576093, 2.824999997268817786, -13.76444248337722875 ) ) ;
#18418 =( BOUNDED_CURVE ( )  B_SPLINE_CURVE ( 2, ( #19837, #7817, #20360, #7649, #31157, #18307, #30806, #5075, #28751, #13312, #2327, #2506, #28245 ),
 .UNSPECIFIED., .F., .T. ) 
 B_SPLINE_CURVE_WITH_KNOTS ( ( 3, 2, 2, 2, 2, 2, 3 ),
 ( 0.6602564102564102422, 0.6615384615384615197, 0.6641025641025640747, 0.6666666666666666297, 0.6692307692307691847, 0.6717948717948717396, 0.6730769230769231282 ),
 .UNSPECIFIED. ) 
 CURVE ( )  GEOMETRIC_REPRESENTATION_ITEM ( )  RATIONAL_B_SPLINE_CURVE ( ( 0.9755282581475768211, 0.9755282581475768211, 1.000000000000000000, 0.9510565162951535312, 1.000000000000000000, 0.9510565162951535312, 1.000000000000000000, 0.9510565162951535312, 1.000000000000000000, 0.9510565162951535312, 1.000000000000000000, 0.9755282581475757109, 0.9755282581475768211 ) ) 
 REPRESENTATION_ITEM ( '' )  );
#18419 = CARTESIAN_POINT ( 'NONE',  ( 10.37757302488624056, 8.775000002731180970, -31.93888565452638417 ) ) ;
#18420 = CARTESIAN_POINT ( 'NONE',  ( 3.000384657911015469E-15, 0.000000000000000000, -24.50000000000000000 ) ) ;
#18421 = CARTESIAN_POINT ( 'NONE',  ( 6.950374756619257965, 31.76003499907602290, -26.09010956794244507 ) ) ;
#18422 = FACE_OUTER_BOUND ( 'NONE', #23417, .T. ) ;
#18423 = DIRECTION ( 'NONE',  ( 0.000000000000000000, 0.000000000000000000, 1.000000000000000000 ) ) ;
#18424 = DIRECTION ( 'NONE',  ( 0.000000000000000000, 0.000000000000000000, -1.000000000000000000 ) ) ;
#18425 = CARTESIAN_POINT ( 'NONE',  ( -33.58253175000000113, 75.27500000273118985, -10.91162601494193218 ) ) ;
#18426 = ORIENTED_EDGE ( 'NONE', *, *, #30738, .F. ) ;
#18427 = CARTESIAN_POINT ( 'NONE',  ( 3.980102097228898626E-15, 80.00000000000001421, 32.50000000000000000 ) ) ;
#18428 = CARTESIAN_POINT ( 'NONE',  ( -26.07999730980490583, 56.40104166666666430, -6.988114217767815717 ) ) ;
#18429 = CARTESIAN_POINT ( 'NONE',  ( -27.16883889988623935, 53.32500000273120122, 19.73931689729374739 ) ) ;
#18430 = AXIS2_PLACEMENT_3D ( 'NONE', #5790, #9188, #5957 ) ;
#18431 = CARTESIAN_POINT ( 'NONE',  ( 10.37757302488624767, 15.97500000273120691, 31.93888565452638417 ) ) ;
#18432 = CARTESIAN_POINT ( 'NONE',  ( -27.16883889988624290, 3.175000002731187543, -19.73931689729374028 ) ) ;
#18433 = CARTESIAN_POINT ( 'NONE',  ( 19.09188309203694800, 37.78124999999999289, 19.09188309203660694 ) ) ;
#18434 = CARTESIAN_POINT ( 'NONE',  ( -28.00173670424549499, 26.90142333425731280, -7.543491769121417612 ) ) ;
#18435 = CARTESIAN_POINT ( 'NONE',  ( -7.468012846824272799, 16.29128499907601579, 28.02196122052058413 ) ) ;
#18436 = CARTESIAN_POINT ( 'NONE',  ( -32.50000000000000000, 72.40000000546235981, -10.55989012756945478 ) ) ;
#18437 = CARTESIAN_POINT ( 'NONE',  ( 26.02353298184809560, 52.00000000000001421, -20.33883978280646332 ) ) ;
#18438 = CARTESIAN_POINT ( 'NONE',  ( -10.37757302488623701, 37.52500000273117564, 31.93888565452638417 ) ) ;
#18439 = CARTESIAN_POINT ( 'NONE',  ( -7.025853678916861966, 48.66107666574268364, -26.06988505166722803 ) ) ;
#18440 = CARTESIAN_POINT ( 'NONE',  ( 18.94512977948575738, 8.424999997268811214, 13.76444248337723408 ) ) ;
#18441 = CARTESIAN_POINT ( 'NONE',  ( 5.779280353836490358E-15, 3.000000005462374109, 32.49999999999999289 ) ) ;
#18442 = ORIENTED_EDGE ( 'NONE', *, *, #6511, .F. ) ;
#18443 = CARTESIAN_POINT ( 'NONE',  ( 10.37757302488624056, 52.77500000273120406, -31.93888565452638417 ) ) ;
#18444 = CARTESIAN_POINT ( 'NONE',  ( -32.50000000000000000, 50.50000000546239676, 0.000000000000000000 ) ) ;
#18445 = CARTESIAN_POINT ( 'NONE',  ( 24.22776226481241224, 41.94048583425730925, -13.94119854578936923 ) ) ;
#18446 = CARTESIAN_POINT ( 'NONE',  ( -20.75514604977248823, 75.07500000273118701, -28.56700777964554305 ) ) ;
#18447 = VERTEX_POINT ( 'NONE', #25757 ) ;
#18448 = CARTESIAN_POINT ( 'NONE',  ( -20.75514604977248112, 21.42500000273120264, 28.56700777964554661 ) ) ;
#18449 = CARTESIAN_POINT ( 'NONE',  ( 20.50609665441005092, 13.71874999999999467, 20.50609665440969209 ) ) ;
#18450 = ORIENTED_EDGE ( 'NONE', *, *, #30542, .T. ) ;
#18451 = CARTESIAN_POINT ( 'NONE',  ( -32.50000000000000000, 57.99999999999997868, 0.000000000000000000 ) ) ;
#18452 = CARTESIAN_POINT ( 'NONE',  ( 33.58253175000000823, 64.02500000273118985, 10.91162601494192863 ) ) ;
#18453 = CARTESIAN_POINT ( 'NONE',  ( -2.584737979205441561E-13, 50.24218750000000711, -30.02300923189239512 ) ) ;
#18454 = CARTESIAN_POINT ( 'NONE',  ( -1.756012107511856980E-14, 6.249999994537623671, -24.50000000000000000 ) ) ;
#18455 = CARTESIAN_POINT ( 'NONE',  ( -14.47279130897152299, 8.424999997268816543, 19.92008829642072243 ) ) ;
#18456 = CARTESIAN_POINT ( 'NONE',  ( -2.162160676586881955E-15, 2.625000002731183724, -35.31076352940723240 ) ) ;
#18457 = CARTESIAN_POINT ( 'NONE',  ( -1.778240108872766143E-15, 6.000000005462371888, -32.49999999999999289 ) ) ;
#18458 = CARTESIAN_POINT ( 'NONE',  ( 25.98046417659831775, 63.12722249907601224, -15.04653450569338879 ) ) ;
#18459 = CARTESIAN_POINT ( 'NONE',  ( 20.08610463437157279, 65.80000000546237970, -27.64615127144129758 ) ) ;
#18460 = CARTESIAN_POINT ( 'NONE',  ( -26.29305231718578995, 60.20000000000001705, 19.10302069950538595 ) ) ;
#18461 = CARTESIAN_POINT ( 'NONE',  ( 20.08610463437158344, 18.69999999999998863, 27.64615127144129403 ) ) ;
#18462 = CARTESIAN_POINT ( 'NONE',  ( 6.988114217768294445, 58.69270833333332860, 26.07999730980477437 ) ) ;
#18463 = CARTESIAN_POINT ( 'NONE',  ( 19.82091636218621034, 17.54999999453762882, 14.40073868116559730 ) ) ;
#18464 = CARTESIAN_POINT ( 'NONE',  ( 4.635254915624209993, 73.65000000546240244, -14.26584774442730463 ) ) ;
#18465 = CARTESIAN_POINT ( 'NONE',  ( 6.988114217767829928, 29.76041666666666430, -26.07999730980489872 ) ) ;
#18466 = EDGE_CURVE ( 'NONE', #25078, #11742, #2242, .T. ) ;
#18467 = CARTESIAN_POINT ( 'NONE',  ( 27.16883889988623935, 22.32500000273118701, -19.73931689729374384 ) ) ;
#18468 = CARTESIAN_POINT ( 'NONE',  ( -20.75514604977248112, 75.42500000273120975, 28.56700777964554661 ) ) ;
#18469 = VECTOR ( 'NONE', #33382, 1000.000000000000000 ) ;
#18470 = CARTESIAN_POINT ( 'NONE',  ( 33.58253175000000113, 38.37500000273118417, -4.112674001490185761E-15 ) ) ;
#18471 = CARTESIAN_POINT ( 'NONE',  ( 33.58253175000000113, 14.47500000273118737, -10.91162601494193574 ) ) ;
#18472 = CARTESIAN_POINT ( 'NONE',  ( 24.18731323226247554, 56.26340250092398065, 14.01125832528285997 ) ) ;
#18473 = CARTESIAN_POINT ( 'NONE',  ( -33.58253175000000113, 79.02500000273118985, -10.91162601494193041 ) ) ;
#18474 = CARTESIAN_POINT ( 'NONE',  ( 15.14183272437242422, 8.300000000000000711, -20.84094480462497856 ) ) ;
#18475 = CARTESIAN_POINT ( 'NONE',  ( 20.08610463437157279, 53.29999999999999716, -27.64615127144129758 ) ) ;
#18476 = CARTESIAN_POINT ( 'NONE',  ( 23.41746824999999887, 18.52499999726881796, 7.608796670333735079 ) ) ;
#18477 = CARTESIAN_POINT ( 'NONE',  ( 6.486482029760648627E-15, 59.62500000273118417, 35.31076352940722529 ) ) ;
#18478 = CARTESIAN_POINT ( 'NONE',  ( -23.41746825000000243, 6.024999997268805529, -7.608796670333730638 ) ) ;
#18479 = AXIS2_PLACEMENT_3D ( 'NONE', #29530, #6033, #19589 ) ;
#18480 = ORIENTED_EDGE ( 'NONE', *, *, #741, .F. ) ;
#18481 = CARTESIAN_POINT ( 'NONE',  ( -27.16883889988624290, 71.17500000273118133, -19.73931689729374028 ) ) ;
#18482 = CARTESIAN_POINT ( 'NONE',  ( -27.16883889988624290, 8.925000002731191984, -19.73931689729374028 ) ) ;
#18483 = CARTESIAN_POINT ( 'NONE',  ( 23.41746824999999887, 0.6249999972688102812, 0.000000000000000000 ) ) ;
#18484 = CARTESIAN_POINT ( 'NONE',  ( 26.06988505166735592, 18.30767333425730214, 7.025853678916393896 ) ) ;
#18485 = ORIENTED_EDGE ( 'NONE', *, *, #765, .F. ) ;
#18486 = AXIS2_PLACEMENT_3D ( 'NONE', #3939, #14414, #22464 ) ;
#18487 = CARTESIAN_POINT ( 'NONE',  ( -20.75514604977248823, 40.82500000273120122, -28.56700777964554305 ) ) ;
#18488 = LINE ( 'NONE', #10116, #24719 ) ;
#18489 = EDGE_LOOP ( 'NONE', ( #24747, #30085, #5972, #8706, #24538, #4836, #21806, #28257, #6305, #33335, #30995, #31625, #26865, #3601, #21555, #26069, #10535, #32581, #29034 ) ) ;
#18490 = CARTESIAN_POINT ( 'NONE',  ( 20.50609665440969565, 43.79687500000000000, -20.50609665441004736 ) ) ;
#18491 = CARTESIAN_POINT ( 'NONE',  ( 10.04305231718578817, 11.90000000546237402, -30.90933677959249337 ) ) ;
#18492 = CARTESIAN_POINT ( 'NONE',  ( 32.50000000000000711, 5.400000005462376684, 10.55989012756945122 ) ) ;
#18493 = CARTESIAN_POINT ( 'NONE',  ( -5.147494310547430452, 71.55125428154684641, -32.49999999999999289 ) ) ;
#18494 = CARTESIAN_POINT ( 'NONE',  ( 15.01150461594596308, 23.02864583333332149, -26.00068869287367335 ) ) ;
#18495 = CARTESIAN_POINT ( 'NONE',  ( 18.94512977948575738, 16.42499999726882010, 13.76444248337723408 ) ) ;
#18496 = CARTESIAN_POINT ( 'NONE',  ( 27.16883889988624290, 6.175000002731190207, 19.73931689729373673 ) ) ;
#18497 = CARTESIAN_POINT ( 'NONE',  ( 6.277390505771533514E-15, 58.49999999999997868, 34.17252228774368916 ) ) ;
#18498 = CARTESIAN_POINT ( 'NONE',  ( 8.601468415847520532, 77.57500000273120122, 11.83890561707634603 ) ) ;
#18499 = CARTESIAN_POINT ( 'NONE',  ( 5.147494310547434893, 73.05125428700921475, 32.49999999999999289 ) ) ;
#18500 = CARTESIAN_POINT ( 'NONE',  ( 28.02196122052058413, 36.05690999907600514, 7.468012846824272799 ) ) ;
#18501 = CARTESIAN_POINT ( 'NONE',  ( -13.91746824999999532, 77.47500000273120691, 4.522059556121122093 ) ) ;
#18502 = CARTESIAN_POINT ( 'NONE',  ( 28.01184896238290278, 37.20833333333332860, -7.505752307973347470 ) ) ;
#18503 = CARTESIAN_POINT ( 'NONE',  ( -3.880418787951136483, 16.30125427608446742, -24.50000000000000000 ) ) ;
#18504 = CARTESIAN_POINT ( 'NONE',  ( -24.50000000000000711, 1.099999999999994316, 7.960532557706201828 ) ) ;
#18505 = CARTESIAN_POINT ( 'NONE',  ( 26.29305231718579350, 4.799999999999998934, 19.10302069950537529 ) ) ;
#18506 = CARTESIAN_POINT ( 'NONE',  ( 10.04305231718579705, 17.10000000546238397, 30.90933677959248982 ) ) ;
#18507 = EDGE_CURVE ( 'NONE', #26616, #5592, #19503, .T. ) ;
#18508 = CARTESIAN_POINT ( 'NONE',  ( -27.95245687107223986, 58.25743083240935505, 0.04044903255043252877 ) ) ;
#18509 = CARTESIAN_POINT ( 'NONE',  ( -27.16883889988623935, 53.32500000273118701, 19.73931689729374739 ) ) ;
#18510 = CARTESIAN_POINT ( 'NONE',  ( -13.91746824999999532, 80.77500000273118985, -4.522059556121115875 ) ) ;
#18511 = CARTESIAN_POINT ( 'NONE',  ( 20.75514604977248467, 58.67500000273118843, -28.56700777964554305 ) ) ;
#18512 = CARTESIAN_POINT ( 'NONE',  ( 6.486482029760648627E-15, 31.87500000273119127, 35.31076352940722529 ) ) ;
#18513 = DIRECTION ( 'NONE',  ( 0.000000000000000000, -0.000000000000000000, 1.000000000000000000 ) ) ;
#18514 = EDGE_CURVE ( 'NONE', #15262, #16375, #20205, .T. ) ;
#18515 = CARTESIAN_POINT ( 'NONE',  ( -15.14183272437242778, 9.299999999999995381, 20.84094480462497856 ) ) ;
#18516 = CARTESIAN_POINT ( 'NONE',  ( -32.50000000000000000, 22.50000000546237189, 0.000000000000000000 ) ) ;
#18517 = CARTESIAN_POINT ( 'NONE',  ( 10.04305231718578817, 75.40000000000000568, -30.90933677959249337 ) ) ;
#18518 = CARTESIAN_POINT ( 'NONE',  ( 20.75514604977248467, 18.42500000273117422, -28.56700777964554305 ) ) ;
#18519 = CARTESIAN_POINT ( 'NONE',  ( 18.94512977948576093, 0.8249999972688160099, -13.76444248337722875 ) ) ;
#18520 = CARTESIAN_POINT ( 'NONE',  ( -1.778240108872766143E-15, 39.50000000000000000, -32.49999999999999289 ) ) ;
#18521 = CARTESIAN_POINT ( 'NONE',  ( 26.09010956794244507, 18.86940999907601935, 6.950374756619249084 ) ) ;
#18522 = CARTESIAN_POINT ( 'NONE',  ( -26.29305231718579350, 38.30000000546239391, -19.10302069950537884 ) ) ;
#18523 = CARTESIAN_POINT ( 'NONE',  ( 19.82091636218621389, 17.94999999453761319, -14.40073868116559197 ) ) ;
#18524 = CARTESIAN_POINT ( 'NONE',  ( -33.58253175000000113, 23.02500000273117919, -10.91162601494193041 ) ) ;
#18525 = CARTESIAN_POINT ( 'NONE',  ( 24.20753774853731244, 47.37760416666666430, -13.97622843553632599 ) ) ;
#18526 = EDGE_LOOP ( 'NONE', ( #24175, #28350, #5552, #9325 ) ) ;
#18527 = CARTESIAN_POINT ( 'NONE',  ( -20.75514604977248823, 60.82500000273121543, -28.56700777964554305 ) ) ;
#18528 = ORIENTED_EDGE ( 'NONE', *, *, #27464, .F. ) ;
#18529 = CARTESIAN_POINT ( 'NONE',  ( 7.505752307973351023, 14.00520833333333215, 28.01184896238290278 ) ) ;
#18530 = CARTESIAN_POINT ( 'NONE',  ( -0.04044903254990864921, 12.14881916759064140, 30.02300923189239867 ) ) ;
#18531 = CARTESIAN_POINT ( 'NONE',  ( -2.162160676586881955E-15, 6.625000002731173510, -35.31076352940723240 ) ) ;
#18532 = ORIENTED_EDGE ( 'NONE', *, *, #6380, .F. ) ;
#18533 = DIRECTION ( 'NONE',  ( -1.000000000000000000, 0.000000000000000000, -0.000000000000000000 ) ) ;
#18534 = CARTESIAN_POINT ( 'NONE',  ( 20.75514604977249178, 32.07500000273117990, 28.56700777964553950 ) ) ;
#18535 = AXIS2_PLACEMENT_3D ( 'NONE', #28438, #30488, #25865 ) ;
#18536 = CARTESIAN_POINT ( 'NONE',  ( 10.04305231718579705, 37.10000000546237686, 30.90933677959248982 ) ) ;
#18537 = CARTESIAN_POINT ( 'NONE',  ( -4.635254915624211769, 73.59999999999999432, -14.26584774442730286 ) ) ;
#18538 = LINE ( 'NONE', #15961, #31852 ) ;
#18539 = CARTESIAN_POINT ( 'NONE',  ( 5.779280353836490358E-15, 53.00000000546238255, 32.49999999999999289 ) ) ;
#18540 = CARTESIAN_POINT ( 'NONE',  ( -20.75514604977248823, 47.07500000273117990, -28.56700777964554305 ) ) ;
#18541 = CARTESIAN_POINT ( 'NONE',  ( -20.08610463437156923, 20.30000000000000071, 27.64615127144130113 ) ) ;
#18542 = CARTESIAN_POINT ( 'NONE',  ( -26.29305231718578995, 20.19999999999999574, 19.10302069950538595 ) ) ;
#18543 = CARTESIAN_POINT ( 'NONE',  ( -4.732186688966233175E-15, 3.500000000000005329, 25.76082449383753925 ) ) ;
#18544 = CARTESIAN_POINT ( 'NONE',  ( -20.75514604977248823, 66.82500000273118701, -28.56700777964554305 ) ) ;
#18545 = CARTESIAN_POINT ( 'NONE',  ( -28.37133278852432738, 66.99999999999998579, 17.03823453610152683 ) ) ;
#18546 = CARTESIAN_POINT ( 'NONE',  ( 4.841599045666881374, 74.00000000000004263, -13.55140770215843027 ) ) ;
#18547 = CARTESIAN_POINT ( 'NONE',  ( -20.75514604977248112, 53.67500000273119554, 28.56700777964554661 ) ) ;
#18548 = CARTESIAN_POINT ( 'NONE',  ( 5.147494310547453544, 73.44874571845316780, -32.49999999999999289 ) ) ;
#18549 = CARTESIAN_POINT ( 'NONE',  ( -33.58253175000000113, 13.12500000273120193, 0.000000000000000000 ) ) ;
#18550 = CARTESIAN_POINT ( 'NONE',  ( -26.09010956794232428, 26.61496500092397355, 6.950374756619732253 ) ) ;
#18551 = CYLINDRICAL_SURFACE ( 'NONE', #25014, 24.50000000000000000 ) ;
#18552 = CARTESIAN_POINT ( 'NONE',  ( 0.000000000000000000, 80.00000000000001421, 0.000000000000000000 ) ) ;
#18553 = CARTESIAN_POINT ( 'NONE',  ( 10.37757302488624056, 34.52500000273118985, -31.93888565452638417 ) ) ;
#18555 = CARTESIAN_POINT ( 'NONE',  ( 26.29305231718578995, 45.70000000546237118, -19.10302069950538240 ) ) ;
#18554 = ADVANCED_BREP_SHAPE_REPRESENTATION ( '', ( #32186, #1376 ), #13943 ) ;
#18556 = CARTESIAN_POINT ( 'NONE',  ( 32.50000000000000000, 18.99999999999998934, -3.980102097228898626E-15 ) ) ;
#18557 = CARTESIAN_POINT ( 'NONE',  ( 13.91746825000000065, 79.77500000273116143, 4.522059556121115875 ) ) ;
#18558 = CARTESIAN_POINT ( 'NONE',  ( -7.468012846824272799, 47.22878499907602645, 28.02196122052058413 ) ) ;
#18559 = CARTESIAN_POINT ( 'NONE',  ( -26.29305231718578995, 54.70000000546236407, 19.10302069950538595 ) ) ;
#18560 = AXIS2_PLACEMENT_3D ( 'NONE', #9413, #19397, #9083 ) ;
#18561 = CARTESIAN_POINT ( 'NONE',  ( 8.601468415847516980, 78.67500000273119554, -11.83890561707634781 ) ) ;
#18562 = CARTESIAN_POINT ( 'NONE',  ( 32.50000000000000711, 60.89999999999999147, 10.55989012756945122 ) ) ;
#18563 = CARTESIAN_POINT ( 'NONE',  ( 27.95245687107222921, 16.72656249999999645, -2.463307335887066074E-13 ) ) ;
#18564 = CARTESIAN_POINT ( 'NONE',  ( 7.236395654485760609, 5.524999997268825958, -22.27133577429736633 ) ) ;
#18565 = CARTESIAN_POINT ( 'NONE',  ( -20.08610463437157989, 72.20000000546237118, -27.64615127144129758 ) ) ;
#18566 = CARTESIAN_POINT ( 'NONE',  ( 20.50609665440969565, 19.73437500000000000, -20.50609665441004736 ) ) ;
#18567 = VECTOR ( 'NONE', #1288, 1000.000000000000000 ) ;
#18568 = EDGE_CURVE ( 'NONE', #19359, #29552, #19106, .T. ) ;
#18569 = CARTESIAN_POINT ( 'NONE',  ( 10.37757302488624056, 28.77500000273118630, -31.93888565452638417 ) ) ;
#18570 = CARTESIAN_POINT ( 'NONE',  ( -18.94512977948575738, 15.92499999726881832, -13.76444248337723231 ) ) ;
#18571 = ORIENTED_EDGE ( 'NONE', *, *, #6845, .T. ) ;
#18572 = CARTESIAN_POINT ( 'NONE',  ( -15.04653450569291984, 36.49777750092397355, 25.98046417659859486 ) ) ;
#18573 = CARTESIAN_POINT ( 'NONE',  ( -10.04305231718578462, 16.90000000546236336, 30.90933677959249337 ) ) ;
#18574 = CARTESIAN_POINT ( 'NONE',  ( -15.01150461594595775, 52.24739583333332860, 26.00068869287368756 ) ) ;
#18575 = CARTESIAN_POINT ( 'NONE',  ( 32.50000000000000000, 75.09999999999996589, -10.55989012756945833 ) ) ;
#18576 = CARTESIAN_POINT ( 'NONE',  ( 33.58253175000000113, 52.47500000273117138, -10.91162601494193751 ) ) ;
#18577 = CARTESIAN_POINT ( 'NONE',  ( 10.04305231718579705, 55.10000000546239107, 30.90933677959248982 ) ) ;
#18578 = CARTESIAN_POINT ( 'NONE',  ( -8.601468415847518756, 79.07500000273118701, -11.83890561707634781 ) ) ;
#18579 = CARTESIAN_POINT ( 'NONE',  ( 20.75514604977248467, 44.42500000273120264, -28.56700777964554305 ) ) ;
#18580 = CARTESIAN_POINT ( 'NONE',  ( -1.778240108872766143E-15, 55.49999999999999289, -32.49999999999999289 ) ) ;
#18581 = CARTESIAN_POINT ( 'NONE',  ( -20.75514604977248823, 71.07500000273117280, -28.56700777964554305 ) ) ;
#18582 = CARTESIAN_POINT ( 'NONE',  ( 10.49071758506610763, 74.00000000000000000, 9.190572033506278160 ) ) ;
#18583 = CARTESIAN_POINT ( 'NONE',  ( 27.16883889988623935, 62.32500000273120833, -19.73931689729374384 ) ) ;
#18584 = CARTESIAN_POINT ( 'NONE',  ( -7.505752307973343918, 19.16145833333332860, -28.01184896238290989 ) ) ;
#18585 = CARTESIAN_POINT ( 'NONE',  ( 26.29305231718578995, 37.20000000000000995, -19.10302069950538240 ) ) ;
#18586 = CARTESIAN_POINT ( 'NONE',  ( 1.507698388325705758E-15, 7.124999997268828267, -24.62258325217400312 ) ) ;
#18587 = CARTESIAN_POINT ( 'NONE',  ( 33.58253175000000823, 12.27500000273116854, 10.91162601494192863 ) ) ;
#18588 = CARTESIAN_POINT ( 'NONE',  ( 15.14183272437242067, 19.44999999453763806, 20.84094480462498211 ) ) ;
#18589 = CARTESIAN_POINT ( 'NONE',  ( -14.01125832528328985, 34.76784749907601935, -24.18731323226223040 ) ) ;
#18590 = DIRECTION ( 'NONE',  ( -0.000000000000000000, -1.000000000000000000, -0.000000000000000000 ) ) ;
#18591 = CARTESIAN_POINT ( 'NONE',  ( -10.37757302488623701, 75.77500000273118985, 31.93888565452638417 ) ) ;
#18592 = CARTESIAN_POINT ( 'NONE',  ( -40.00000000000000711, 52.00000000000000711, 23.09401076758504345 ) ) ;
#18593 = CARTESIAN_POINT ( 'NONE',  ( 33.58253175000000113, 72.47500000273119269, -10.91162601494193751 ) ) ;
#18594 = ORIENTED_EDGE ( 'NONE', *, *, #24875, .F. ) ;
#18595 = CARTESIAN_POINT ( 'NONE',  ( 0.000000000000000000, 82.00000000000001421, 0.000000000000000000 ) ) ;
#18596 = CARTESIAN_POINT ( 'NONE',  ( 13.97622843553589966, 60.84114583333332860, -24.20753774853756113 ) ) ;
#18597 = CARTESIAN_POINT ( 'NONE',  ( 20.75514604977249178, 51.82500000273120122, 28.56700777964553950 ) ) ;
#18598 = CARTESIAN_POINT ( 'NONE',  ( 27.16883889988624290, 18.17500000273118843, 19.73931689729373673 ) ) ;
#18599 = CARTESIAN_POINT ( 'NONE',  ( -2.162160676586881955E-15, 6.875000002731180615, -35.31076352940723240 ) ) ;
#18600 = CARTESIAN_POINT ( 'NONE',  ( 6.988114217767829928, 36.63541666666666430, -26.07999730980489872 ) ) ;
#18601 = CARTESIAN_POINT ( 'NONE',  ( -14.97647472619946285, 27.33111083425731280, -26.02091320914851025 ) ) ;
#18602 = EDGE_CURVE ( 'NONE', #13970, #33138, #29602, .T. ) ;
#18603 = CARTESIAN_POINT ( 'NONE',  ( 14.97647472619900455, 14.71576416574268720, -26.02091320914876960 ) ) ;
#18604 = CARTESIAN_POINT ( 'NONE',  ( -32.50000000000000000, 76.60000000546239107, 10.55989012756946366 ) ) ;
#18605 = CARTESIAN_POINT ( 'NONE',  ( 10.64935084019646538, 52.00000000000002132, -30.92824909085711838 ) ) ;
#18606 = CARTESIAN_POINT ( 'NONE',  ( 10.37757302488624056, 40.52500000273118275, -31.93888565452638417 ) ) ;
#18607 = CARTESIAN_POINT ( 'NONE',  ( -26.06988505166722803, 44.36420166574269075, 7.025853678916877953 ) ) ;
#18608 = CARTESIAN_POINT ( 'NONE',  ( -7.236395654485757944, 17.22499999726881370, -22.27133577429736988 ) ) ;
#18609 = EDGE_CURVE ( 'NONE', #23226, #11830, #13902, .T. ) ;
#18610 = CARTESIAN_POINT ( 'NONE',  ( 1.555960095263670572E-15, 14.50000000000000178, -24.50000000000000000 ) ) ;
#18611 = VERTEX_POINT ( 'NONE', #11649 ) ;
#18612 = CARTESIAN_POINT ( 'NONE',  ( -2.162160676586881955E-15, 46.87500000273118417, -35.31076352940723240 ) ) ;
#18613 = CARTESIAN_POINT ( 'NONE',  ( -13.38432950954956624, -58.51673569255127205, 0.000000000000000000 ) ) ;
#18614 = CARTESIAN_POINT ( 'NONE',  ( 24.22776226481241224, 48.81548583425731636, -13.94119854578936923 ) ) ;
#18615 = CARTESIAN_POINT ( 'NONE',  ( -20.75514604977248112, 69.67500000273119554, 28.56700777964554661 ) ) ;
#18616 = ORIENTED_EDGE ( 'NONE', *, *, #7565, .F. ) ;
#18617 = CARTESIAN_POINT ( 'NONE',  ( 10.37757302488624056, 22.52500000273117919, -31.93888565452638417 ) ) ;
#18618 = EDGE_CURVE ( 'NONE', #12120, #11025, #16695, .T. ) ;
#18619 = CARTESIAN_POINT ( 'NONE',  ( -20.50609665441004736, 29.18749999999999645, -20.50609665440969565 ) ) ;
#18620 = VERTEX_POINT ( 'NONE', #22297 ) ;
#18621 =( BOUNDED_CURVE ( )  B_SPLINE_CURVE ( 2, ( #511, #2423, #10996, #7736, #13717, #20800, #31244, #18562, #8076, #21136, #26442, #31577, #23701 ),
 .UNSPECIFIED., .F., .T. ) 
 B_SPLINE_CURVE_WITH_KNOTS ( ( 3, 2, 2, 2, 2, 2, 3 ),
 ( 0.2371794871794871973, 0.2384615384615384748, 0.2410256410256410298, 0.2435897435897435848, 0.2461538461538461675, 0.2487179487179487225, 0.2500000000000000000 ),
 .UNSPECIFIED. ) 
 CURVE ( )  GEOMETRIC_REPRESENTATION_ITEM ( )  RATIONAL_B_SPLINE_CURVE ( ( 0.9755282581475768211, 0.9755282581475770431, 1.000000000000000000, 0.9510565162951535312, 1.000000000000000000, 0.9510565162951535312, 1.000000000000000000, 0.9510565162951535312, 1.000000000000000000, 0.9510565162951535312, 1.000000000000000000, 0.9755282581475768211, 0.9755282581475768211 ) ) 
 REPRESENTATION_ITEM ( '' )  );
#18622 = CARTESIAN_POINT ( 'NONE',  ( 6.001560367445586717E-15, 3.249999994537631665, 24.50000000000000000 ) ) ;
#18623 = CARTESIAN_POINT ( 'NONE',  ( 10.37757302488624767, 61.72500000273117848, 31.93888565452638417 ) ) ;
#18624 = CARTESIAN_POINT ( 'NONE',  ( 20.50609665441005092, 48.09375000000000000, 20.50609665440969209 ) ) ;
#18625 = CARTESIAN_POINT ( 'NONE',  ( -24.50000000000001066, 17.10000000000001208, 7.960532557706201828 ) ) ;
#18626 = CARTESIAN_POINT ( 'NONE',  ( -14.47279130897152299, 10.42499999726881121, 19.92008829642072243 ) ) ;
#18627 = CARTESIAN_POINT ( 'NONE',  ( 33.58253175000000113, 4.125000002731193938, -4.112674001490185761E-15 ) ) ;
#18628 = CARTESIAN_POINT ( 'NONE',  ( 27.16883889988624290, 28.17500000273118133, 19.73931689729373673 ) ) ;
#18629 = SURFACE_STYLE_USAGE ( .BOTH. , #26836 ) ;
#18630 = CARTESIAN_POINT ( 'NONE',  ( -14.97647472619899389, 64.55951416574268364, 26.02091320914878025 ) ) ;
#18631 = CARTESIAN_POINT ( 'NONE',  ( -20.75514604977248823, 79.07500000273121543, -28.56700777964554305 ) ) ;
#18632 = CARTESIAN_POINT ( 'NONE',  ( -13.91746824999999532, 80.77500000273118985, -4.522059556121115875 ) ) ;
#18633 = CARTESIAN_POINT ( 'NONE',  ( 20.08610463437157279, 75.80000000546237970, -27.64615127144129758 ) ) ;
#18634 = CARTESIAN_POINT ( 'NONE',  ( 10.04305231718578817, 15.40000000000001101, -30.90933677959249337 ) ) ;
#18635 = CARTESIAN_POINT ( 'NONE',  ( -26.07999730980490583, 59.83854166666666430, -6.988114217767815717 ) ) ;
#18636 = CARTESIAN_POINT ( 'NONE',  ( -7.570916362186215665, 17.14999999453761959, 23.30088464923126423 ) ) ;
#18637 = CARTESIAN_POINT ( 'NONE',  ( -13.91746824999999532, 78.77500000273116143, -4.522059556121115875 ) ) ;
#18638 = CARTESIAN_POINT ( 'NONE',  ( -6.988114217767819270, 34.91666666666666430, 26.07999730980490583 ) ) ;
#18639 = CARTESIAN_POINT ( 'NONE',  ( -27.16883889988624290, 24.92500000273117777, -19.73931689729374028 ) ) ;
#18640 = CARTESIAN_POINT ( 'NONE',  ( 33.58253175000000823, 72.02500000273118985, 10.91162601494192863 ) ) ;
#18641 = CARTESIAN_POINT ( 'NONE',  ( -33.58253175000000113, 37.47500000273118559, 10.91162601494193929 ) ) ;
#18642 = CARTESIAN_POINT ( 'NONE',  ( 10.37757302488624056, 16.77500000273118985, -31.93888565452638417 ) ) ;
#18643 = CARTESIAN_POINT ( 'NONE',  ( 6.950374756619721595, 60.13059000092398065, 26.09010956794232428 ) ) ;
#18644 = CARTESIAN_POINT ( 'NONE',  ( -20.75514604977248823, 72.82500000273117280, -28.56700777964554305 ) ) ;
#18645 = CARTESIAN_POINT ( 'NONE',  ( 5.779280353836490358E-15, 59.00000000546238255, 32.49999999999999289 ) ) ;
#18646 = CARTESIAN_POINT ( 'NONE',  ( -32.50000000000000000, 51.89999999999998437, -10.55989012756945478 ) ) ;
#18647 = CARTESIAN_POINT ( 'NONE',  ( 4.635254915624209993, 79.65000000546237402, -14.26584774442730463 ) ) ;
#18648 = CARTESIAN_POINT ( 'NONE',  ( 27.16883889988623935, 58.32500000273119412, -19.73931689729374384 ) ) ;
#18649 = CARTESIAN_POINT ( 'NONE',  ( -23.41746825000000598, 8.224999997268824359, 7.608796670333726198 ) ) ;
#18650 = ORIENTED_EDGE ( 'NONE', *, *, #13886, .F. ) ;
#18651 = CARTESIAN_POINT ( 'NONE',  ( -2.162160676586881955E-15, 66.87500000273119838, -35.31076352940723240 ) ) ;
#18652 = CARTESIAN_POINT ( 'NONE',  ( 33.58253175000000113, 2.225000002731166937, -10.91162601494193574 ) ) ;
#18653 = CARTESIAN_POINT ( 'NONE',  ( 18.94512977948575738, 2.424999997268806329, 13.76444248337723408 ) ) ;
#18654 = CARTESIAN_POINT ( 'NONE',  ( 27.95245687107223986, 14.72694416759064318, 0.04044903254993640479 ) ) ;
#18655 = ORIENTED_EDGE ( 'NONE', *, *, #31502, .F. ) ;
#18656 = CARTESIAN_POINT ( 'NONE',  ( 27.16883889988624290, 45.92500000273118133, 19.73931689729373673 ) ) ;
#18657 = DIRECTION ( 'NONE',  ( 0.000000000000000000, 1.000000000000000000, 0.000000000000000000 ) ) ;
#18658 = ORIENTED_EDGE ( 'NONE', *, *, #18122, .T. ) ;
#18659 = CARTESIAN_POINT ( 'NONE',  ( 15.01150461594596308, 40.21614583333332860, -26.00068869287367335 ) ) ;
#18660 = CARTESIAN_POINT ( 'NONE',  ( 3.000384657911015469E-15, 16.99999999999998579, 24.50000000000000000 ) ) ;
#18661 = CARTESIAN_POINT ( 'NONE',  ( -26.29305231718578995, 4.700000005462376507, 19.10302069950538595 ) ) ;
#18662 = CARTESIAN_POINT ( 'NONE',  ( -10.04305231718579172, 71.59999999999999432, -30.90933677959248982 ) ) ;
#18663 = CARTESIAN_POINT ( 'NONE',  ( -26.00068869287368756, 18.73177083333332149, -15.01150461594595775 ) ) ;
#18664 = CARTESIAN_POINT ( 'NONE',  ( -7.570916362186210335, 2.599999999999991207, -23.30088464923126779 ) ) ;
#18665 = CARTESIAN_POINT ( 'NONE',  ( -27.16883889988624290, 11.17500000273119554, -19.73931689729374028 ) ) ;
#18666 = CARTESIAN_POINT ( 'NONE',  ( 10.04305231718578817, 61.40000000000001279, -30.90933677959249337 ) ) ;
#18667 = CARTESIAN_POINT ( 'NONE',  ( -8.601468415847515203, 79.17500000273120975, 11.83890561707634959 ) ) ;
#18668 = CARTESIAN_POINT ( 'NONE',  ( 2.694222958124179176E-15, -45.00000000000001421, 0.000000000000000000 ) ) ;
#18669 = CARTESIAN_POINT ( 'NONE',  ( -20.47846945139866648, 30.32774333240935150, 20.53372385742108008 ) ) ;
#18670 = CARTESIAN_POINT ( 'NONE',  ( 13.91746825000000065, 78.27500000273116143, 4.522059556121114987 ) ) ;
#18671 = CARTESIAN_POINT ( 'NONE',  ( 15.01150461594643382, 44.79947916666667140, 26.00068869287340334 ) ) ;
#18672 = CONTEXT_DEPENDENT_SHAPE_REPRESENTATION ( #10963, #12880 ) ;
#18673 = CARTESIAN_POINT ( 'NONE',  ( 0.000000000000000000, 74.00000000000001421, 0.000000000000000000 ) ) ;
#18674 = CARTESIAN_POINT ( 'NONE',  ( -19.82091636218621389, 1.200000000000006617, 14.40073868116558842 ) ) ;
#18675 = CARTESIAN_POINT ( 'NONE',  ( -26.29305231718578995, 4.199999999999981526, 19.10302069950538595 ) ) ;
#18676 = CYLINDRICAL_SURFACE ( 'NONE', #4464, 32.50000000000000000 ) ;
#18677 = CARTESIAN_POINT ( 'NONE',  ( -19.11951029504797006, 62.12461833240934794, -19.06425588902558133 ) ) ;
#18678 = CARTESIAN_POINT ( 'NONE',  ( -20.75514604977248823, 46.82500000273117990, -28.56700777964554305 ) ) ;
#18679 = CARTESIAN_POINT ( 'NONE',  ( -9.657523855033125146E-16, 73.75000000546233991, -15.77193336357400710 ) ) ;
#18680 = CARTESIAN_POINT ( 'NONE',  ( -20.75514604977248823, 55.07500000273117990, -28.56700777964554305 ) ) ;
#18681 = CARTESIAN_POINT ( 'NONE',  ( 2.688165632520823219E-15, 77.87500000273119838, 14.63369212191046387 ) ) ;
#18682 = CARTESIAN_POINT ( 'NONE',  ( -20.75514604977248112, 37.67500000273118133, 28.56700777964554661 ) ) ;
#18683 = CYLINDRICAL_SURFACE ( 'NONE', #33600, 24.50000000000000000 ) ;
#18684 = CARTESIAN_POINT ( 'NONE',  ( 19.09188309203661049, 23.17187499999999289, -19.09188309203694445 ) ) ;
#18685 = CARTESIAN_POINT ( 'NONE',  ( -7.579748464070165821E-14, 12.24999999453762456, -24.50000000000000000 ) ) ;
#18686 = CARTESIAN_POINT ( 'NONE',  ( -2.375766604868041476, 76.44874571845315359, 14.99999999999999822 ) ) ;
#18687 = CARTESIAN_POINT ( 'NONE',  ( -20.08610463437156923, 70.30000000000001137, 27.64615127144130113 ) ) ;
#18688 = CARTESIAN_POINT ( 'NONE',  ( 6.486482029760649416E-15, 17.62500000273117351, 35.31076352940723240 ) ) ;
#18689 = CARTESIAN_POINT ( 'NONE',  ( -23.41746825000000243, 7.724999997268811036, 7.608796670333725309 ) ) ;
#18690 = CARTESIAN_POINT ( 'NONE',  ( -10.04305231718579172, 39.59999999999999432, -30.90933677959248982 ) ) ;
#18691 = CARTESIAN_POINT ( 'NONE',  ( 6.950374756619257965, 14.57253499907601935, -26.09010956794244507 ) ) ;
#18692 = CARTESIAN_POINT ( 'NONE',  ( -10.04305231718579172, 11.59999999999999964, -30.90933677959248982 ) ) ;
#18693 = CARTESIAN_POINT ( 'NONE',  ( -33.58253175000000113, 19.02500000273118630, -10.91162601494193041 ) ) ;
#18694 = CARTESIAN_POINT ( 'NONE',  ( -2.428612866367529427E-13, 39.92968750000000000, -27.95245687107222921 ) ) ;
#18695 = ORIENTED_EDGE ( 'NONE', *, *, #30881, .T. ) ;
#18696 = CARTESIAN_POINT ( 'NONE',  ( 20.75514604977249178, 61.82500000273116569, 28.56700777964553950 ) ) ;
#18697 = EDGE_CURVE ( 'NONE', #32671, #33362, #2466, .T. ) ;
#18698 = EDGE_LOOP ( 'NONE', ( #26783, #1054, #4665, #18232 ) ) ;
#18699 = CARTESIAN_POINT ( 'NONE',  ( -28.01184896238304134, 18.58854166666666430, -7.505752307972844761 ) ) ;
#18700 = CARTESIAN_POINT ( 'NONE',  ( 0.04044903254992426173, 13.86756916759064318, -30.02300923189239867 ) ) ;
#18701 = CARTESIAN_POINT ( 'NONE',  ( -2.162160676586881955E-15, 2.625000002731183724, -35.31076352940723240 ) ) ;
#18702 = ADVANCED_FACE ( 'NONE', ( #16816 ), #1169, .F. ) ;
#18703 = VERTEX_POINT ( 'NONE', #33258 ) ;
#18704 = DIRECTION ( 'NONE',  ( 0.000000000000000000, 0.000000000000000000, 1.000000000000000000 ) ) ;
#18705 = CARTESIAN_POINT ( 'NONE',  ( -10.37757302488624411, 28.97500000273117848, -31.93888565452638417 ) ) ;
#18706 = CARTESIAN_POINT ( 'NONE',  ( -26.29305231718579350, 40.30000000546237970, -19.10302069950537884 ) ) ;
#18707 = CARTESIAN_POINT ( 'NONE',  ( 32.50000000000000000, 79.10000000000000853, -10.55989012756945833 ) ) ;
#18708 = CARTESIAN_POINT ( 'NONE',  ( -1.778240108872766143E-15, 34.00000000546236834, -32.49999999999999289 ) ) ;
#18709 = CARTESIAN_POINT ( 'NONE',  ( -10.04305231718578462, 52.90000000546239534, 30.90933677959249337 ) ) ;
#18710 = CARTESIAN_POINT ( 'NONE',  ( -27.16883889988624290, 43.17500000273119554, -19.73931689729374028 ) ) ;
#18711 = APPLICATION_PROTOCOL_DEFINITION ( 'draft international standard', 'automotive_design', 1998, #5501 ) ;
#18712 = CARTESIAN_POINT ( 'NONE',  ( -32.50000000000000000, 25.89999999999999503, -10.55989012756945478 ) ) ;
#18713 = CARTESIAN_POINT ( 'NONE',  ( 10.04305231718578817, 23.40000000000000568, -30.90933677959249337 ) ) ;
#18714 = CARTESIAN_POINT ( 'NONE',  ( 19.82091636218621389, 6.200000000000010836, -14.40073868116559197 ) ) ;
#18715 = CARTESIAN_POINT ( 'NONE',  ( 33.58253175000000823, 64.02500000273118985, 10.91162601494192863 ) ) ;
#18716 = CARTESIAN_POINT ( 'NONE',  ( -32.17340636219239514, 66.99999999999997158, 8.405285767817538556 ) ) ;
#18717 = CARTESIAN_POINT ( 'NONE',  ( -1.778240108872766143E-15, 37.50000000000000000, -32.49999999999999289 ) ) ;
#18718 = CARTESIAN_POINT ( 'NONE',  ( 20.75514604977248467, 52.67500000273116711, -28.56700777964554305 ) ) ;
#18719 = CARTESIAN_POINT ( 'NONE',  ( 23.41746824999999887, 2.624999997268812280, 0.000000000000000000 ) ) ;
#18720 = CARTESIAN_POINT ( 'NONE',  ( -1.756012107511856980E-14, 4.249999994537631665, -24.50000000000000000 ) ) ;
#18721 = CARTESIAN_POINT ( 'NONE',  ( 27.16883889988623935, 14.32500000273117990, -19.73931689729374384 ) ) ;
#18722 = CARTESIAN_POINT ( 'NONE',  ( 7.025853678916403666, 34.63579833425730925, -26.06988505166735237 ) ) ;
#18723 = CARTESIAN_POINT ( 'NONE',  ( 13.42768774669677612, 66.99999999999998579, -30.32522641246981365 ) ) ;
#18724 = CARTESIAN_POINT ( 'NONE',  ( 24.50000000000000000, 1.749999994537621006, 0.000000000000000000 ) ) ;
#18725 = CARTESIAN_POINT ( 'NONE',  ( -10.37757302488624411, 32.72500000273119269, -31.93888565452638417 ) ) ;
#18726 = AXIS2_PLACEMENT_3D ( 'NONE', #14377, #24836, #1314 ) ;
#18727 = CYLINDRICAL_SURFACE ( 'NONE', #31967, 32.50000000000000000 ) ;
#18728 = CARTESIAN_POINT ( 'NONE',  ( 11.25946833292375793, 77.67500000273119554, 8.180482586598731842 ) ) ;
#18729 = CARTESIAN_POINT ( 'NONE',  ( -28.02196122052058413, 44.65065999907601935, -7.468012846824272799 ) ) ;
#18730 = CARTESIAN_POINT ( 'NONE',  ( 32.50000000000000000, 53.50000000546238965, -3.980102097228898626E-15 ) ) ;
#18731 = CARTESIAN_POINT ( 'NONE',  ( -4.300734207923759378, 72.97500000273122112, -13.23629886949340495 ) ) ;
#18732 = CARTESIAN_POINT ( 'NONE',  ( 26.07999730980477437, 20.02083333333332860, -6.988114217768290004 ) ) ;
#18733 = CARTESIAN_POINT ( 'NONE',  ( -26.29305231718579350, 72.30000000546237970, -19.10302069950537884 ) ) ;
#18734 = CARTESIAN_POINT ( 'NONE',  ( 28.01184896238304134, 23.74479166666666430, 7.505752307972846538 ) ) ;
#18735 = CARTESIAN_POINT ( 'NONE',  ( -20.75514604977248823, 27.07500000273119412, -28.56700777964554305 ) ) ;
#18736 = CARTESIAN_POINT ( 'NONE',  ( 7.236395654485760609, 13.52499999726880553, -22.27133577429736633 ) ) ;
#18737 = ORIENTED_EDGE ( 'NONE', *, *, #337, .F. ) ;
#18738 = CARTESIAN_POINT ( 'NONE',  ( -30.02300923189239867, 37.07069416759063785, -0.04044903254991731589 ) ) ;
#18739 = CARTESIAN_POINT ( 'NONE',  ( 26.29305231718578995, 19.70000000546238894, -19.10302069950538240 ) ) ;
#18740 = CARTESIAN_POINT ( 'NONE',  ( -20.50609665440969209, 55.82812499999999289, 20.50609665441005092 ) ) ;
#18741 = CARTESIAN_POINT ( 'NONE',  ( 33.58253175000000823, 48.27500000273119696, 10.91162601494192863 ) ) ;
#18742 = EDGE_CURVE ( 'NONE', #30585, #29752, #17833, .T. ) ;
#18743 = CARTESIAN_POINT ( 'NONE',  ( 10.04305231718579705, 59.10000000546239107, 30.90933677959248982 ) ) ;
#18744 = CARTESIAN_POINT ( 'NONE',  ( 11.25946833292375793, 78.57500000273121543, -8.180482586598735395 ) ) ;
#18745 = CARTESIAN_POINT ( 'NONE',  ( 10.37757302488624767, 37.72500000273118559, 31.93888565452638417 ) ) ;
#18746 = CARTESIAN_POINT ( 'NONE',  ( 26.29305231718578995, 55.19999999999999574, -19.10302069950538240 ) ) ;
#18747 = CARTESIAN_POINT ( 'NONE',  ( -33.58253175000000113, 59.27500000273119696, -10.91162601494193218 ) ) ;
#18748 = FACE_OUTER_BOUND ( 'NONE', #22593, .T. ) ;
#18749 = CARTESIAN_POINT ( 'NONE',  ( 33.58253175000000113, 52.12500000273119838, -4.112674001490185761E-15 ) ) ;
#18750 = CARTESIAN_POINT ( 'NONE',  ( 20.50609665441005092, 20.59374999999999645, 20.50609665440969209 ) ) ;
#18751 = CARTESIAN_POINT ( 'NONE',  ( 32.50000000000000000, 42.99999999999998579, -3.980102097228898626E-15 ) ) ;
#18752 = CARTESIAN_POINT ( 'NONE',  ( 23.41746825000000243, 4.724999997268818142, -7.608796670333727974 ) ) ;
#18753 = CARTESIAN_POINT ( 'NONE',  ( 33.58253175000000113, 10.37500000273117173, -4.112674001490185761E-15 ) ) ;
#18754 = CARTESIAN_POINT ( 'NONE',  ( -4.223320258572819786E-15, 19.24999999453763166, 24.50000000000000000 ) ) ;
#18755 = FACE_OUTER_BOUND ( 'NONE', #11083, .T. ) ;
#18756 = CARTESIAN_POINT ( 'NONE',  ( -27.16883889988623935, 75.57500000273120122, 19.73931689729374739 ) ) ;
#18757 = DIRECTION ( 'NONE',  ( 0.000000000000000000, 0.000000000000000000, -1.000000000000000000 ) ) ;
#18758 = CARTESIAN_POINT ( 'NONE',  ( -20.75514604977248112, 65.67500000273118133, 28.56700777964554661 ) ) ;
#18759 = ORIENTED_EDGE ( 'NONE', *, *, #26240, .T. ) ;
#18760 = CARTESIAN_POINT ( 'NONE',  ( 3.980102097228898626E-15, 80.00000000000001421, 32.50000000000000000 ) ) ;
#18761 = CARTESIAN_POINT ( 'NONE',  ( 27.95245687107222921, 61.41406250000000711, -2.463307335887066074E-13 ) ) ;
#18762 = CARTESIAN_POINT ( 'NONE',  ( 6.486482029760649416E-15, 55.62500000273119838, 35.31076352940723240 ) ) ;
#18763 = CARTESIAN_POINT ( 'NONE',  ( -33.58253175000000113, 13.27500000273118097, -10.91162601494193218 ) ) ;
#18764 = CARTESIAN_POINT ( 'NONE',  ( -10.37757302488624411, 6.975000002731198911, -31.93888565452638417 ) ) ;
#18765 = CARTESIAN_POINT ( 'NONE',  ( -13.97622843553632777, 36.20572916666665719, -24.20753774853731599 ) ) ;
#18766 = CARTESIAN_POINT ( 'NONE',  ( 25.98046417659858420, 32.20090250092397355, 15.04653450569292872 ) ) ;
#18767 = CARTESIAN_POINT ( 'NONE',  ( 7.543491769121922985, 19.44232666574268364, 28.00173670424535644 ) ) ;
#18768 = CARTESIAN_POINT ( 'NONE',  ( -32.50000000000000000, 74.60000000546234844, 10.55989012756946366 ) ) ;
#18769 = DIRECTION ( 'NONE',  ( -0.000000000000000000, -1.000000000000000000, -0.000000000000000000 ) ) ;
#18770 = CARTESIAN_POINT ( 'NONE',  ( 33.58253175000000113, 36.12500000273119127, -4.112674001490185761E-15 ) ) ;
#18771 = CARTESIAN_POINT ( 'NONE',  ( -24.22776226481266448, 44.79388916574269075, -13.94119854578892514 ) ) ;
#18772 = CARTESIAN_POINT ( 'NONE',  ( 18.94512977948576093, 14.82499999726880091, -13.76444248337722875 ) ) ;
#18773 = CARTESIAN_POINT ( 'NONE',  ( 3.980102097228898626E-15, 80.00000000000001421, 32.50000000000000000 ) ) ;
#18774 = ORIENTED_EDGE ( 'NONE', *, *, #7702, .F. ) ;
#18775 = CARTESIAN_POINT ( 'NONE',  ( -27.16883889988624290, 45.17500000273118133, -19.73931689729374028 ) ) ;
#18776 = CARTESIAN_POINT ( 'NONE',  ( -1.778240108872766143E-15, 51.50000000000000711, -32.49999999999999289 ) ) ;
#18777 = CARTESIAN_POINT ( 'NONE',  ( 19.11951029504763611, 52.10975666759065206, -19.06425588902591173 ) ) ;
#18778 = CARTESIAN_POINT ( 'NONE',  ( -33.58253175000000113, 71.37500000273119838, 0.000000000000000000 ) ) ;
#18779 = ORIENTED_EDGE ( 'NONE', *, *, #12008, .F. ) ;
#18780 = CARTESIAN_POINT ( 'NONE',  ( 10.37757302488624056, 16.52500000273120051, -31.93888565452638417 ) ) ;
#18781 = CARTESIAN_POINT ( 'NONE',  ( -30.02300923189239512, 28.75781249999999645, 2.654126918244515359E-13 ) ) ;
#18782 = ORIENTED_EDGE ( 'NONE', *, *, #26576, .T. ) ;
#18783 = CIRCLE ( 'NONE', #16042, 24.50000000000000000 ) ;
#18784 = CARTESIAN_POINT ( 'NONE',  ( -12.11000150615021198, -45.00000000000000000, 0.000000000000000000 ) ) ;
#18785 = CARTESIAN_POINT ( 'NONE',  ( 20.75514604977249178, 51.82500000273120122, 28.56700777964553950 ) ) ;
#18786 = CARTESIAN_POINT ( 'NONE',  ( 15.01150461594643204, 48.23697916666665719, 26.00068869287340334 ) ) ;
#18787 = CARTESIAN_POINT ( 'NONE',  ( 6.277390505771533514E-15, 17.00000000546237544, 34.17252228774368916 ) ) ;
#18788 = VECTOR ( 'NONE', #24394, 1000.000000000000000 ) ;
#18789 = CARTESIAN_POINT ( 'NONE',  ( 0.000000000000000000, 52.00000000000000711, 32.50000000000000000 ) ) ;
#18790 = CARTESIAN_POINT ( 'NONE',  ( 14.47279130897151944, 7.424999997268819207, -19.92008829642072598 ) ) ;
#18791 = CARTESIAN_POINT ( 'NONE',  ( -27.16883889988623935, 31.57500000273119767, 19.73931689729374739 ) ) ;
#18792 = CARTESIAN_POINT ( 'NONE',  ( -32.50000000000000000, 63.99999999999998579, 0.000000000000000000 ) ) ;
#18793 = CARTESIAN_POINT ( 'NONE',  ( -26.02091320914878025, 58.54388916574269075, -14.97647472619899389 ) ) ;
#18794 = CARTESIAN_POINT ( 'NONE',  ( -26.29305231718578995, 32.20000000000000284, 19.10302069950538595 ) ) ;
#18795 = CARTESIAN_POINT ( 'NONE',  ( -20.08610463437156923, 60.29999999999997584, 27.64615127144130113 ) ) ;
#18796 = CARTESIAN_POINT ( 'NONE',  ( -2.092463501923844636E-15, 7.499999999999995559, -34.17252228774368916 ) ) ;
#18797 = CARTESIAN_POINT ( 'NONE',  ( 19.09188309203694800, 61.84374999999998579, 19.09188309203660694 ) ) ;
#18798 = CARTESIAN_POINT ( 'NONE',  ( 24.50000000000000355, 17.64999999453763380, 7.960532557706212486 ) ) ;
#18799 = CARTESIAN_POINT ( 'NONE',  ( -8.601468415847518756, 72.57500000273117280, -11.83890561707634781 ) ) ;
#18800 = CARTESIAN_POINT ( 'NONE',  ( 13.97622843553589966, 29.90364583333332504, -24.20753774853756113 ) ) ;
#18801 = CARTESIAN_POINT ( 'NONE',  ( -10.37757302488624411, 24.72500000273119980, -31.93888565452638417 ) ) ;
#18802 = CARTESIAN_POINT ( 'NONE',  ( 33.58253175000000113, 72.12500000273118417, -4.112674001490185761E-15 ) ) ;
#18803 = CARTESIAN_POINT ( 'NONE',  ( -33.58253175000000113, 39.37500000273118417, 0.000000000000000000 ) ) ;
#18804 = CARTESIAN_POINT ( 'NONE',  ( 33.58253175000000113, 14.37500000273117529, -4.112674001490185761E-15 ) ) ;
#18805 = CARTESIAN_POINT ( 'NONE',  ( -19.11951029504763611, 57.26600666759063785, 19.06425588902592239 ) ) ;
#18806 = CARTESIAN_POINT ( 'NONE',  ( 10.37757302488624056, 70.52500000273120406, -31.93888565452638417 ) ) ;
#18807 = DIRECTION ( 'NONE',  ( 0.000000000000000000, 0.000000000000000000, -1.000000000000000000 ) ) ;
#18808 = AXIS2_PLACEMENT_3D ( 'NONE', #29832, #6334, #19551 ) ;
#18809 = CARTESIAN_POINT ( 'NONE',  ( -20.08610463437156923, 52.30000000000001137, 27.64615127144130113 ) ) ;
#18810 = DIRECTION ( 'NONE',  ( -1.224646799147353454E-16, 1.000000000000000000, -0.000000000000000000 ) ) ;
#18811 = CARTESIAN_POINT ( 'NONE',  ( -20.75514604977248823, 56.82500000273118701, -28.56700777964554305 ) ) ;
#18812 = VECTOR ( 'NONE', #96, 1000.000000000000000 ) ;
#18813 = CARTESIAN_POINT ( 'NONE',  ( -14.47279130897152122, 12.42499999726880766, 19.92008829642072243 ) ) ;
#18814 = ORIENTED_EDGE ( 'NONE', *, *, #14919, .F. ) ;
#18815 = CARTESIAN_POINT ( 'NONE',  ( -2.162160676586881955E-15, 68.87500000273118417, -35.31076352940723240 ) ) ;
#18816 = CARTESIAN_POINT ( 'NONE',  ( -20.75514604977248112, 1.425000002731191984, 28.56700777964554661 ) ) ;
#18817 = CARTESIAN_POINT ( 'NONE',  ( 23.41746825000000243, 8.724999997268806595, -7.608796670333727974 ) ) ;
#18818 = CARTESIAN_POINT ( 'NONE',  ( -24.22776226481240514, 19.59673583425730925, 13.94119854578937812 ) ) ;
#18819 = ORIENTED_EDGE ( 'NONE', *, *, #1891, .F. ) ;
#18820 = CARTESIAN_POINT ( 'NONE',  ( -27.16883889988624290, 38.92500000273117422, -19.73931689729374028 ) ) ;
#18821 = CARTESIAN_POINT ( 'NONE',  ( -7.570916362186215665, 1.400000000000012346, 23.30088464923126423 ) ) ;
#18822 = EDGE_CURVE ( 'NONE', #4234, #9459, #7007, .T. ) ;
#18823 = ORIENTED_EDGE ( 'NONE', *, *, #32006, .F. ) ;
#18824 = CARTESIAN_POINT ( 'NONE',  ( 7.505752307973351023, 55.25520833333333570, 28.01184896238290278 ) ) ;
#18825 = CARTESIAN_POINT ( 'NONE',  ( 20.08610463437157279, 11.80000000546236372, -27.64615127144129758 ) ) ;
#18826 = CARTESIAN_POINT ( 'NONE',  ( -26.29305231718578995, 0.7000000054623728429, 19.10302069950538595 ) ) ;
#18827 = DIRECTION ( 'NONE',  ( 0.8660254037844398178, 0.4999999999999979461, -0.000000000000000000 ) ) ;
#18828 = CARTESIAN_POINT ( 'NONE',  ( 7.505752307972854531, 19.44791666666666075, -28.01184896238303423 ) ) ;
#18829 = CARTESIAN_POINT ( 'NONE',  ( -4.523095164977116484E-15, 18.12499999726880517, 24.62258325217400312 ) ) ;
#18830 = CARTESIAN_POINT ( 'NONE',  ( 10.37757302488624056, 6.775000002731179194, -31.93888565452638417 ) ) ;
#18831 = CARTESIAN_POINT ( 'NONE',  ( -10.04305231718578462, 58.40000000000000568, 30.90933677959249337 ) ) ;
#18832 = CARTESIAN_POINT ( 'NONE',  ( 32.50000000000000711, 57.40000000546237402, 10.55989012756945122 ) ) ;
#18833 = CARTESIAN_POINT ( 'NONE',  ( -26.02091320914878025, 34.48138916574268364, -14.97647472619899389 ) ) ;
#18834 = CARTESIAN_POINT ( 'NONE',  ( 2.688165632520823219E-15, 75.87500000273119838, 14.63369212191046387 ) ) ;
#18835 = CARTESIAN_POINT ( 'NONE',  ( 15.01150461594596486, 47.09114583333332860, -26.00068869287367690 ) ) ;
#18836 = VECTOR ( 'NONE', #10740, 1000.000000000000000 ) ;
#18837 = DIRECTION ( 'NONE',  ( 0.000000000000000000, 0.000000000000000000, -1.000000000000000000 ) ) ;
#18838 = CARTESIAN_POINT ( 'NONE',  ( 0.000000000000000000, 0.000000000000000000, 0.000000000000000000 ) ) ;
#18839 = CARTESIAN_POINT ( 'NONE',  ( -0.04044903255042732459, 59.11680583240937636, -27.95245687107223986 ) ) ;
#18840 = CARTESIAN_POINT ( 'NONE',  ( -33.58253175000000113, 43.22500000273118559, 10.91162601494193929 ) ) ;
#18841 = CARTESIAN_POINT ( 'NONE',  ( -11.25946833292375793, 80.67500000273119554, -8.180482586598733619 ) ) ;
#18842 = CARTESIAN_POINT ( 'NONE',  ( 10.37757302488624056, 56.77500000273121117, -31.93888565452638417 ) ) ;
#18843 = CARTESIAN_POINT ( 'NONE',  ( -33.58253175000000113, 35.37500000273119127, 0.000000000000000000 ) ) ;
#18844 = CARTESIAN_POINT ( 'NONE',  ( 20.08610463437157279, 25.29999999999998295, -27.64615127144129758 ) ) ;
#18845 = CARTESIAN_POINT ( 'NONE',  ( 13.97622843553589966, 26.46614583333332504, -24.20753774853756113 ) ) ;
#18846 = CARTESIAN_POINT ( 'NONE',  ( 8.891200544363830713E-16, 79.75000000546238255, -15.00000000000000000 ) ) ;
#18847 = CARTESIAN_POINT ( 'NONE',  ( -15.00000000000000000, 79.89999999999997726, -4.873795443493594171 ) ) ;
#18848 = CARTESIAN_POINT ( 'NONE',  ( -20.08610463437157989, 71.69999999999997442, -27.64615127144129758 ) ) ;
#18849 = CARTESIAN_POINT ( 'NONE',  ( 33.58253175000000113, 6.225000002731185589, -10.91162601494193751 ) ) ;
#18850 = CARTESIAN_POINT ( 'NONE',  ( -18.94512977948576093, 1.824999997268816898, 13.76444248337722698 ) ) ;
#18851 = DIRECTION ( 'NONE',  ( 0.000000000000000000, 0.000000000000000000, -1.000000000000000000 ) ) ;
#18852 = CARTESIAN_POINT ( 'NONE',  ( 27.95245687107223276, 25.60118083240935860, -0.04044903255042905932 ) ) ;
#18853 = DIRECTION ( 'NONE',  ( 0.000000000000000000, 0.000000000000000000, -1.000000000000000000 ) ) ;
#18854 = CARTESIAN_POINT ( 'NONE',  ( -10.37757302488624411, 18.72500000273119625, -31.93888565452638417 ) ) ;
#18855 = CARTESIAN_POINT ( 'NONE',  ( -19.09188309203660694, 52.39062499999999289, 19.09188309203694800 ) ) ;
#18856 = CIRCLE ( 'NONE', #6220, 13.38408793869266411 ) ;
#18857 = ORIENTED_EDGE ( 'NONE', *, *, #33212, .T. ) ;
#18858 = CARTESIAN_POINT ( 'NONE',  ( -10.37757302488623701, 55.52500000273118275, 31.93888565452638417 ) ) ;
#18859 = ORIENTED_EDGE ( 'NONE', *, *, #27617, .T. ) ;
#18860 = CARTESIAN_POINT ( 'NONE',  ( -7.505752307972844761, 17.72916666666666430, 28.01184896238304134 ) ) ;
#18861 = CARTESIAN_POINT ( 'NONE',  ( -20.47846945139902175, 13.43788166759064140, -20.53372385742072481 ) ) ;
#18862 = CARTESIAN_POINT ( 'NONE',  ( 33.58253175000000113, 2.125000002731192161, -4.112674001490185761E-15 ) ) ;
#18863 = ORIENTED_EDGE ( 'NONE', *, *, #29589, .F. ) ;
#18864 = CARTESIAN_POINT ( 'NONE',  ( 0.000000000000000000, 0.000000000000000000, 0.000000000000000000 ) ) ;
#18865 = CARTESIAN_POINT ( 'NONE',  ( -33.58253175000000113, 31.27500000273118275, -10.91162601494193218 ) ) ;
#18866 = CARTESIAN_POINT ( 'NONE',  ( 10.04305231718579705, 29.10000000546236620, 30.90933677959248982 ) ) ;
#18867 = CARTESIAN_POINT ( 'NONE',  ( 32.50000000000000000, 79.00000000000001421, -3.980102097228898626E-15 ) ) ;
#18868 = DIRECTION ( 'NONE',  ( 1.000000000000000000, 0.000000000000000000, 0.000000000000000000 ) ) ;
#18869 = CARTESIAN_POINT ( 'NONE',  ( 27.16883889988623935, 44.57500000273117990, -19.73931689729374384 ) ) ;
#18870 = SHAPE_REPRESENTATION_RELATIONSHIP ( 'NONE' , 'NONE' ,  #8075, #18554 ) ;
#18871 = CARTESIAN_POINT ( 'NONE',  ( -2.092463501923844636E-15, 25.50000000000001066, -34.17252228774368916 ) ) ;
#18872 = CARTESIAN_POINT ( 'NONE',  ( 32.50000000000000000, 20.99999999999998934, -3.980102097228898626E-15 ) ) ;
#18873 = CARTESIAN_POINT ( 'NONE',  ( -15.14183272437241889, 12.70000000000000639, -20.84094480462497856 ) ) ;
#18874 = CARTESIAN_POINT ( 'NONE',  ( 33.58253175000000113, 64.12500000273119838, -4.112674001490185761E-15 ) ) ;
#18875 = CARTESIAN_POINT ( 'NONE',  ( 15.14183272437241889, 5.449999994537614079, 20.84094480462498211 ) ) ;
#18876 = CARTESIAN_POINT ( 'NONE',  ( 0.2410918355672596325, 74.00000000000002842, -14.56788933630795491 ) ) ;
#18877 = CARTESIAN_POINT ( 'NONE',  ( -20.75514604977248112, 55.67500000273119554, 28.56700777964554661 ) ) ;
#18878 = CARTESIAN_POINT ( 'NONE',  ( 23.41746824999999887, 6.624999997268815832, 0.000000000000000000 ) ) ;
#18879 = CARTESIAN_POINT ( 'NONE',  ( -15.14183272437242778, 9.299999999999995381, 20.84094480462497856 ) ) ;
#18880 = CARTESIAN_POINT ( 'NONE',  ( -10.37757302488623701, 5.525000002731205839, 31.93888565452638417 ) ) ;
#18881 = CARTESIAN_POINT ( 'NONE',  ( -6.950374756619716266, 37.78684000092396644, -26.09010956794232428 ) ) ;
#18882 = EDGE_CURVE ( 'NONE', #14306, #4197, #32897, .T. ) ;
#18883 = CARTESIAN_POINT ( 'NONE',  ( 20.29802760220268709, 16.99999999999999289, -11.70263796218577745 ) ) ;
#18884 = CARTESIAN_POINT ( 'NONE',  ( -32.50000000000000000, 19.90000000000001279, -10.55989012756945300 ) ) ;
#18885 = UNCERTAINTY_MEASURE_WITH_UNIT (LENGTH_MEASURE( 1.000000000000000082E-05 ), #6321, 'distance_accuracy_value', 'NONE');
#18886 = CARTESIAN_POINT ( 'NONE',  ( -27.16883889988624290, 30.92500000273119909, -19.73931689729374028 ) ) ;
#18887 = CARTESIAN_POINT ( 'NONE',  ( -32.50000000000000000, 56.40000000546237402, -10.55989012756945300 ) ) ;
#18888 = DIRECTION ( 'NONE',  ( 0.000000000000000000, -1.000000000000000000, 0.000000000000000000 ) ) ;
#18889 = EDGE_CURVE ( 'NONE', #4296, #17375, #29171, .T. ) ;
#18890 = CARTESIAN_POINT ( 'NONE',  ( -8.601468415847518756, 74.57500000273120122, -11.83890561707634603 ) ) ;
#18891 = CARTESIAN_POINT ( 'NONE',  ( -28.02196122052058413, 51.52565999907602645, -7.468012846824272799 ) ) ;
#18892 = CARTESIAN_POINT ( 'NONE',  ( -10.04305231718579172, 54.10000000546237686, -30.90933677959248982 ) ) ;
#18893 = CARTESIAN_POINT ( 'NONE',  ( 8.601468415847520532, 72.07500000273117280, 11.83890561707634781 ) ) ;
#18894 = LINE ( 'NONE', #675, #32584 ) ;
#18895 = CARTESIAN_POINT ( 'NONE',  ( 6.988114217767829928, 16.01041666666666075, -26.07999730980489872 ) ) ;
#18896 = ORIENTED_EDGE ( 'NONE', *, *, #23201, .T. ) ;
#18897 = CARTESIAN_POINT ( 'NONE',  ( -26.29305231718578995, 68.70000000546238539, 19.10302069950538595 ) ) ;
#18898 = CARTESIAN_POINT ( 'NONE',  ( -20.50609665440969209, 31.76562499999999289, 20.50609665441005092 ) ) ;
#18899 = AXIS2_PLACEMENT_3D ( 'NONE', #27761, #22608, #25700 ) ;
#18900 = CARTESIAN_POINT ( 'NONE',  ( 7.236395654485755280, 12.72499999726881015, 22.27133577429736988 ) ) ;
#18901 = ORIENTED_EDGE ( 'NONE', *, *, #33839, .F. ) ;
#18902 = CARTESIAN_POINT ( 'NONE',  ( 26.02091320914851025, 38.50298583425730925, -14.97647472619946463 ) ) ;
#18903 = CARTESIAN_POINT ( 'NONE',  ( 10.04305231718579705, 19.10000000546237331, 30.90933677959248982 ) ) ;
#18904 = CARTESIAN_POINT ( 'NONE',  ( -15.01150461594642138, 53.39322916666665009, -26.00068869287340334 ) ) ;
#18905 = CARTESIAN_POINT ( 'NONE',  ( 8.305033359366087120E-16, -29.78157438140398483, 0.000000000000000000 ) ) ;
#18906 = CARTESIAN_POINT ( 'NONE',  ( -20.75514604977248112, 45.67500000273119554, 28.56700777964554661 ) ) ;
#18907 = CARTESIAN_POINT ( 'NONE',  ( 32.50000000000000711, 55.40000000546238113, 10.55989012756945122 ) ) ;
#18908 =( BOUNDED_CURVE ( )  B_SPLINE_CURVE ( 2, ( #2539, #13521, #33592, #5279, #18337, #3050, #31190, #8186, #31527, #28782, #18506, #5108, #20747 ),
 .UNSPECIFIED., .F., .F. ) 
 B_SPLINE_CURVE_WITH_KNOTS ( ( 3, 2, 2, 2, 2, 2, 3 ),
 ( 0.7756410256410256610, 0.7769230769230769384, 0.7794871794871794934, 0.7820512820512820484, 0.7846153846153846034, 0.7871794871794871584, 0.7884615384615384359 ),
 .UNSPECIFIED. ) 
 CURVE ( )  GEOMETRIC_REPRESENTATION_ITEM ( )  RATIONAL_B_SPLINE_CURVE ( ( 0.9755282581475768211, 0.9755282581475768211, 1.000000000000000000, 0.9510565162951535312, 1.000000000000000000, 0.9510565162951535312, 1.000000000000000000, 0.9510565162951535312, 1.000000000000000000, 0.9510565162951535312, 1.000000000000000000, 0.9755282581475768211, 0.9755282581475768211 ) ) 
 REPRESENTATION_ITEM ( '' )  );
#18909 = CARTESIAN_POINT ( 'NONE',  ( -13.91746824999999887, 81.37500000273118417, 0.000000000000000000 ) ) ;
#18910 = CARTESIAN_POINT ( 'NONE',  ( 6.486482029760649416E-15, 33.62500000273119127, 35.31076352940723240 ) ) ;
#18911 = CARTESIAN_POINT ( 'NONE',  ( 5.147494310547429563, 77.94874572391552192, -32.50000000000000000 ) ) ;
#18912 = CARTESIAN_POINT ( 'NONE',  ( 33.58253175000000113, 60.37500000273119127, -4.112674001490185761E-15 ) ) ;
#18913 = CARTESIAN_POINT ( 'NONE',  ( 9.527563637176564626, 74.00000000000000000, 10.15519155137115881 ) ) ;
#18914 = CARTESIAN_POINT ( 'NONE',  ( 20.75514604977249178, 53.82500000273119412, 28.56700777964553950 ) ) ;
#18915 = CARTESIAN_POINT ( 'NONE',  ( 28.01184896238290278, 20.02083333333332860, -7.505752307973347470 ) ) ;
#18916 = CARTESIAN_POINT ( 'NONE',  ( 26.29305231718578995, 39.20000000000000995, -19.10302069950538240 ) ) ;
#18917 = CARTESIAN_POINT ( 'NONE',  ( 7.236395654485755280, 6.224999997268803931, 22.27133577429736988 ) ) ;
#18918 = CARTESIAN_POINT ( 'NONE',  ( -2.162160676586881955E-15, 2.875000002731204596, -35.31076352940723240 ) ) ;
#18919 = CARTESIAN_POINT ( 'NONE',  ( -10.04305231718578462, 66.90000000546238823, 30.90933677959249337 ) ) ;
#18920 = CARTESIAN_POINT ( 'NONE',  ( 2.688165632520823219E-15, 73.87500000273119838, 14.63369212191046387 ) ) ;
#18921 = CARTESIAN_POINT ( 'NONE',  ( 20.75514604977248467, 72.67500000273118133, -28.56700777964554305 ) ) ;
#18922 = DIRECTION ( 'NONE',  ( -0.000000000000000000, -1.000000000000000000, -0.000000000000000000 ) ) ;
#18923 = CARTESIAN_POINT ( 'NONE',  ( 6.486482029760649416E-15, 67.87500000273116996, 35.31076352940723240 ) ) ;
#18924 = ORIENTED_EDGE ( 'NONE', *, *, #33, .F. ) ;
#18925 = CARTESIAN_POINT ( 'NONE',  ( 23.41746824999999887, 19.12499999726882649, 0.000000000000000000 ) ) ;
#18926 = AXIS2_PLACEMENT_3D ( 'NONE', #22457, #2034, #12509 ) ;
#18927 = CARTESIAN_POINT ( 'NONE',  ( -13.97622843553632421, 63.70572916666667140, -24.20753774853731599 ) ) ;
#18928 = EDGE_CURVE ( 'NONE', #23800, #30543, #17658, .T. ) ;
#18929 = DIRECTION ( 'NONE',  ( 0.000000000000000000, -1.000000000000000000, 0.000000000000000000 ) ) ;
#18930 = CARTESIAN_POINT ( 'NONE',  ( -33.58253175000000113, 55.02500000273118985, -10.91162601494193218 ) ) ;
#18931 = CARTESIAN_POINT ( 'NONE',  ( -2.162160676586881955E-15, 10.87500000273118417, -35.31076352940723240 ) ) ;
#18932 = CARTESIAN_POINT ( 'NONE',  ( 20.75514604977248467, 62.67500000273117422, -28.56700777964554305 ) ) ;
#18933 = CARTESIAN_POINT ( 'NONE',  ( -24.20753774853730889, 52.53385416666666430, 13.97622843553634020 ) ) ;
#18934 = CARTESIAN_POINT ( 'NONE',  ( -14.97647472619946285, 34.20611083425730925, -26.02091320914851025 ) ) ;
#18935 = EDGE_CURVE ( 'NONE', #31633, #5766, #27952, .T. ) ;
#18936 = CARTESIAN_POINT ( 'NONE',  ( -20.53372385742107653, 20.87461833240935505, -20.47846945139867003 ) ) ;
#18937 = CARTESIAN_POINT ( 'NONE',  ( -10.04305231718579172, 76.10000000546239107, -30.90933677959248982 ) ) ;
#18938 = CARTESIAN_POINT ( 'NONE',  ( -8.601468415847515203, 79.17500000273116711, 11.83890561707634959 ) ) ;
#18939 = CARTESIAN_POINT ( 'NONE',  ( 33.58253175000000113, 38.22500000273119269, -10.91162601494193574 ) ) ;
#18940 = CARTESIAN_POINT ( 'NONE',  ( 0.04044903255044120238, 50.52305583240934794, 27.95245687107223276 ) ) ;
#18941 = CARTESIAN_POINT ( 'NONE',  ( 23.41746825000000243, 12.72499999726882436, -7.608796670333727974 ) ) ;
#18942 = CARTESIAN_POINT ( 'NONE',  ( 15.14183272437242422, 14.30000000000001492, -20.84094480462497856 ) ) ;
#18943 = ORIENTED_EDGE ( 'NONE', *, *, #17634, .F. ) ;
#18944 = CARTESIAN_POINT ( 'NONE',  ( -33.58253175000000113, 49.47500000273118559, 10.91162601494193929 ) ) ;
#18945 = CARTESIAN_POINT ( 'NONE',  ( -15.00000000000000000, 70.35000000546237686, 4.873795443493597723 ) ) ;
#18946 = CARTESIAN_POINT ( 'NONE',  ( 6.950374756619721595, 53.25559000092396644, 26.09010956794232428 ) ) ;
#18947 = CARTESIAN_POINT ( 'NONE',  ( 33.58253175000000113, 68.47500000273119269, -10.91162601494193751 ) ) ;
#18948 = ORIENTED_EDGE ( 'NONE', *, *, #32716, .F. ) ;
#18949 = CARTESIAN_POINT ( 'NONE',  ( 20.75514604977249178, 19.82500000273119412, 28.56700777964553950 ) ) ;
#18950 = CARTESIAN_POINT ( 'NONE',  ( -28.01184896238304134, 22.02604166666666430, -7.505752307972844761 ) ) ;
#18951 = ORIENTED_EDGE ( 'NONE', *, *, #12936, .F. ) ;
#18952 = CARTESIAN_POINT ( 'NONE',  ( 32.50000000000000000, 65.50000000546238255, -3.980102097228898626E-15 ) ) ;
#18953 = CARTESIAN_POINT ( 'NONE',  ( 33.58253175000000113, 58.12500000273118417, -4.112674001490185761E-15 ) ) ;
#18954 = CARTESIAN_POINT ( 'NONE',  ( 20.50609665440969565, 50.67187500000000000, -20.50609665441004736 ) ) ;
#18955 = CARTESIAN_POINT ( 'NONE',  ( -32.50000000000000000, 20.60000000546237686, 10.55989012756946366 ) ) ;
#18956 = FACE_OUTER_BOUND ( 'NONE', #8267, .T. ) ;
#18957 = CARTESIAN_POINT ( 'NONE',  ( -14.47279130897151767, 9.824999997268800911, -19.92008829642072598 ) ) ;
#18958 = CARTESIAN_POINT ( 'NONE',  ( 33.58253175000000113, 26.47500000273118559, -10.91162601494193751 ) ) ;
#18959 = VECTOR ( 'NONE', #14978, 1000.000000000000000 ) ;
#18960 = SURFACE_STYLE_FILL_AREA ( #14847 ) ;
#18961 = CARTESIAN_POINT ( 'NONE',  ( 27.95245687107223276, 18.72618083240936215, -0.04044903255042905932 ) ) ;
#18962 = CARTESIAN_POINT ( 'NONE',  ( 2.688165632520823219E-15, 79.37500000273119838, 14.63369212191046387 ) ) ;
#18963 = CARTESIAN_POINT ( 'NONE',  ( -20.08610463437157989, 28.20000000546236762, -27.64615127144129758 ) ) ;
#18964 = CARTESIAN_POINT ( 'NONE',  ( 10.04305231718579705, 8.599999999999981881, 30.90933677959248982 ) ) ;
#18965 = ORIENTED_EDGE ( 'NONE', *, *, #5376, .T. ) ;
#18966 = CARTESIAN_POINT ( 'NONE',  ( 1.577395562988744260E-15, 16.24999999453762456, -25.76082449383753925 ) ) ;
#18967 = CARTESIAN_POINT ( 'NONE',  ( -13.91746824999999887, 74.87500000273116996, 0.000000000000000000 ) ) ;
#18968 = CARTESIAN_POINT ( 'NONE',  ( -26.07999730980477437, 28.61458333333333215, 6.988114217768305103 ) ) ;
#18969 = CARTESIAN_POINT ( 'NONE',  ( 33.58253175000000113, 26.12500000273118417, -4.112674001490185761E-15 ) ) ;
#18970 = CARTESIAN_POINT ( 'NONE',  ( -10.37757302488624411, 74.72500000273117848, -31.93888565452638417 ) ) ;
#18971 = CARTESIAN_POINT ( 'NONE',  ( -33.58253175000000113, 27.37500000273117351, 0.000000000000000000 ) ) ;
#18972 = CARTESIAN_POINT ( 'NONE',  ( -20.75514604977248112, 17.67500000273117422, 28.56700777964554661 ) ) ;
#18973 = CARTESIAN_POINT ( 'NONE',  ( -26.09010956794232428, 60.98996500092398065, 6.950374756619732253 ) ) ;
#18974 = CARTESIAN_POINT ( 'NONE',  ( -33.58253175000000113, 73.02500000273118985, -10.91162601494193041 ) ) ;
#18975 = CARTESIAN_POINT ( 'NONE',  ( 0.000000000000000000, 80.00000000000001421, -32.50000000000000000 ) ) ;
#18976 = CARTESIAN_POINT ( 'NONE',  ( 4.300734207923761154, 75.97500000273119269, 13.23629886949340495 ) ) ;
#18977 = CARTESIAN_POINT ( 'NONE',  ( 26.29305231718578995, 57.20000000000001705, -19.10302069950538240 ) ) ;
#18978 = CARTESIAN_POINT ( 'NONE',  ( -15.00000000000000000, 72.15000000546237402, -4.873795443493594171 ) ) ;
#18979 = CARTESIAN_POINT ( 'NONE',  ( 33.58253175000000113, 56.22500000273117138, -10.91162601494193574 ) ) ;
#18980 = CARTESIAN_POINT ( 'NONE',  ( -7.236395654485757944, 13.72499999726881015, -22.27133577429736988 ) ) ;
#18981 = ORIENTED_EDGE ( 'NONE', *, *, #18609, .T. ) ;
#18982 = CARTESIAN_POINT ( 'NONE',  ( -33.58253175000000113, 65.27500000273117564, -10.91162601494193218 ) ) ;
#18983 = CARTESIAN_POINT ( 'NONE',  ( -32.50000000000000000, 15.89999999999998970, -10.55989012756945300 ) ) ;
#18984 = AXIS2_PLACEMENT_3D ( 'NONE', #27170, #29730, #26552 ) ;
#18985 = CARTESIAN_POINT ( 'NONE',  ( 14.47279130897151589, 6.324999997268824892, 19.92008829642072953 ) ) ;
#18986 = CARTESIAN_POINT ( 'NONE',  ( 19.11951029504763611, 28.04725666759063429, -19.06425588902591173 ) ) ;
#18987 = ORIENTED_EDGE ( 'NONE', *, *, #1457, .T. ) ;
#18988 = CARTESIAN_POINT ( 'NONE',  ( 33.58253175000000823, 40.02500000273119696, 10.91162601494192863 ) ) ;
#18989 = LINE ( 'NONE', #14165, #9373 ) ;
#18990 = EDGE_LOOP ( 'NONE', ( #25306, #31290, #4915, #14499 ) ) ;
#18991 = CARTESIAN_POINT ( 'NONE',  ( 26.00068869287340334, 50.81510416666667140, -15.01150461594642316 ) ) ;
#18992 = CARTESIAN_POINT ( 'NONE',  ( 5.147494310547426899, 11.94874572391553436, -32.50000000000000000 ) ) ;
#18993 = CARTESIAN_POINT ( 'NONE',  ( 12.13525491562420910, 75.45000000546237118, -8.816778784387098611 ) ) ;
#18994 = CARTESIAN_POINT ( 'NONE',  ( 27.16883889988623935, 76.32500000273118701, -19.73931689729374384 ) ) ;
#18995 = CARTESIAN_POINT ( 'NONE',  ( -20.50609665441004736, 22.31250000000000000, -20.50609665440969565 ) ) ;
#18996 = CARTESIAN_POINT ( 'NONE',  ( -24.50000000000000355, 8.900000000000011013, -7.960532557706207157 ) ) ;
#18997 = CARTESIAN_POINT ( 'NONE',  ( 27.16883889988624290, 10.17500000273119376, 19.73931689729373673 ) ) ;
#18998 = CARTESIAN_POINT ( 'NONE',  ( 27.16883889988623935, 14.32500000273117990, -19.73931689729374384 ) ) ;
#18999 = CARTESIAN_POINT ( 'NONE',  ( -4.300734207923759378, 76.47500000273119269, -13.23629886949340495 ) ) ;
#19000 = DIRECTION ( 'NONE',  ( -1.224646799147353454E-16, 1.000000000000000000, -0.000000000000000000 ) ) ;
#19001 = CARTESIAN_POINT ( 'NONE',  ( -0.04044903255044120238, 38.49180583240935505, -30.02300923189239867 ) ) ;
#19002 = CARTESIAN_POINT ( 'NONE',  ( -8.601468415847515203, 75.67500000273118133, 11.83890561707634959 ) ) ;
#19003 = CARTESIAN_POINT ( 'NONE',  ( 15.01150461594643382, 48.23697916666665009, 26.00068869287340334 ) ) ;
#19004 = CARTESIAN_POINT ( 'NONE',  ( 20.08610463437158344, 53.20000000546237118, 27.64615127144129403 ) ) ;
#19005 = CARTESIAN_POINT ( 'NONE',  ( 20.08610463437157279, 71.29999999999999716, -27.64615127144129758 ) ) ;
#19006 = CARTESIAN_POINT ( 'NONE',  ( -26.06988505166722803, 61.55170166574269786, 7.025853678916877953 ) ) ;
#19007 = CARTESIAN_POINT ( 'NONE',  ( 27.16883889988624290, 45.92500000273119554, 19.73931689729373673 ) ) ;
#19008 = CARTESIAN_POINT ( 'NONE',  ( 4.635254915624212657, 70.85000000546237686, 14.26584774442730286 ) ) ;
#19009 = CARTESIAN_POINT ( 'NONE',  ( 10.37757302488624767, 47.97500000273117848, 31.93888565452638417 ) ) ;
#19010 = CARTESIAN_POINT ( 'NONE',  ( 33.58253175000000113, 36.47500000273119269, -10.91162601494193574 ) ) ;
#19011 =( BOUNDED_CURVE ( )  B_SPLINE_CURVE ( 2, ( #9214, #27250, #16792, #9380, #29813, #19862, #32554, #30316, #6813, #27928, #17294, #9053, #14717 ),
 .UNSPECIFIED., .F., .T. ) 
 B_SPLINE_CURVE_WITH_KNOTS ( ( 3, 2, 2, 2, 2, 2, 3 ),
 ( 0.9166666666666666297, 0.9179487179487179072, 0.9205128205128204621, 0.9230769230769231282, 0.9256410256410256832, 0.9282051282051282382, 0.9294871794871795156 ),
 .UNSPECIFIED. ) 
 CURVE ( )  GEOMETRIC_REPRESENTATION_ITEM ( )  RATIONAL_B_SPLINE_CURVE ( ( 0.9755282581475768211, 0.9755282581475768211, 1.000000000000000000, 0.9510565162951535312, 1.000000000000000000, 0.9510565162951535312, 1.000000000000000000, 0.9510565162951535312, 1.000000000000000000, 0.9510565162951535312, 1.000000000000000000, 0.9755282581475768211, 0.9755282581475768211 ) ) 
 REPRESENTATION_ITEM ( '' )  );
#19012 = CARTESIAN_POINT ( 'NONE',  ( 18.29076905308899370, 16.99999999999997868, 14.90902754751065906 ) ) ;
#19013 = CARTESIAN_POINT ( 'NONE',  ( 27.95245687107223276, 23.60156250000000000, -2.463307335887066074E-13 ) ) ;
#19014 = DIRECTION ( 'NONE',  ( -1.000000000000000000, 0.000000000000000000, 0.000000000000000000 ) ) ;
#19015 = AXIS2_PLACEMENT_3D ( 'NONE', #7677, #31524, #15760 ) ;
#19016 = CARTESIAN_POINT ( 'NONE',  ( 5.779280353836490358E-15, 30.49999999999999645, 32.49999999999999289 ) ) ;
#19017 =( BOUNDED_CURVE ( )  B_SPLINE_CURVE ( 2, ( #15371, #7288, #12446, #2665, #22916, #31309, #18292, #17773, #28564, #2316, #5060, #15197, #28737 ),
 .UNSPECIFIED., .F., .T. ) 
 B_SPLINE_CURVE_WITH_KNOTS ( ( 3, 2, 2, 2, 2, 2, 3 ),
 ( 0.05000000000000000278, 0.05999999999999999778, 0.08000000000000000167, 0.1000000000000000056, 0.1199999999999999956, 0.1400000000000000133, 0.1500000000000000222 ),
 .UNSPECIFIED. ) 
 CURVE ( )  GEOMETRIC_REPRESENTATION_ITEM ( )  RATIONAL_B_SPLINE_CURVE ( ( 0.9755282581475768211, 0.9755282581475768211, 1.000000000000000000, 0.9510565162951535312, 1.000000000000000000, 0.9510565162951535312, 1.000000000000000000, 0.9510565162951535312, 1.000000000000000000, 0.9510565162951535312, 1.000000000000000000, 0.9755282581475767101, 0.9755282581475768211 ) ) 
 REPRESENTATION_ITEM ( '' )  );
#19018 = CARTESIAN_POINT ( 'NONE',  ( -26.29305231718578995, 72.20000000000000284, 19.10302069950538595 ) ) ;
#19019 = CARTESIAN_POINT ( 'NONE',  ( -27.16883889988623935, 11.32500000273119234, 19.73931689729374739 ) ) ;
#19020 = CARTESIAN_POINT ( 'NONE',  ( -18.94512977948575738, 1.424999997268805441, -13.76444248337723231 ) ) ;
#19021 = ADVANCED_FACE ( 'NONE', ( #25717 ), #33432, .T. ) ;
#19022 = CARTESIAN_POINT ( 'NONE',  ( 1.093617666956751375E-13, 60.00000000546238255, -32.50000000000000711 ) ) ;
#19023 = CARTESIAN_POINT ( 'NONE',  ( -27.95245687107223986, 27.31993083240935505, 0.04044903255043252877 ) ) ;
#19024 = CARTESIAN_POINT ( 'NONE',  ( 27.16883889988624290, 19.92500000273117422, 19.73931689729373673 ) ) ;
#19025 = CARTESIAN_POINT ( 'NONE',  ( -6.988114217768288228, 50.09895833333332860, -26.07999730980477437 ) ) ;
#19026 = EDGE_CURVE ( 'NONE', #17621, #12035, #32903, .T. ) ;
#19027 = ORIENTED_EDGE ( 'NONE', *, *, #32630, .T. ) ;
#19028 = CARTESIAN_POINT ( 'NONE',  ( 27.16883889988623935, 54.32500000273120122, -19.73931689729374384 ) ) ;
#19029 = ADVANCED_FACE ( 'NONE', ( #25374 ), #23140, .T. ) ;
#19030 = ORIENTED_EDGE ( 'NONE', *, *, #19442, .F. ) ;
#19031 = CARTESIAN_POINT ( 'NONE',  ( 26.00068869287367335, 27.32552083333332860, 15.01150461594596308 ) ) ;
#19032 = CARTESIAN_POINT ( 'NONE',  ( -26.02091320914849959, 19.59673583425730925, 14.97647472619947528 ) ) ;
#19033 = CARTESIAN_POINT ( 'NONE',  ( 6.486482029760649416E-15, 1.625000002731185944, 35.31076352940723240 ) ) ;
#19034 = EDGE_CURVE ( 'NONE', #18081, #5219, #33606, .T. ) ;
#19035 = CARTESIAN_POINT ( 'NONE',  ( 1.507698388325705758E-15, 7.124999997268799845, -24.62258325217400312 ) ) ;
#19036 = CARTESIAN_POINT ( 'NONE',  ( 33.58253175000000823, 30.27500000273118630, 10.91162601494192863 ) ) ;
#19037 = CARTESIAN_POINT ( 'NONE',  ( -26.29305231718578995, 28.70000000546238539, 19.10302069950538595 ) ) ;
#19038 = CARTESIAN_POINT ( 'NONE',  ( 20.08610463437158344, 76.70000000000000284, 27.64615127144129403 ) ) ;
#19039 = LINE ( 'NONE', #10969, #17628 ) ;
#19040 = CARTESIAN_POINT ( 'NONE',  ( 5.147494310547434893, 37.05125428700922185, 32.49999999999999289 ) ) ;
#19041 = CARTESIAN_POINT ( 'NONE',  ( -20.75514604977248112, 45.67500000273119554, 28.56700777964554661 ) ) ;
#19042 = AXIS2_PLACEMENT_3D ( 'NONE', #2906, #13547, #33965 ) ;
#19043 = CARTESIAN_POINT ( 'NONE',  ( 26.29305231718578995, 25.19999999999998508, -19.10302069950538240 ) ) ;
#19044 = CARTESIAN_POINT ( 'NONE',  ( -32.50000000000000000, 19.90000000000001279, -10.55989012756945478 ) ) ;
#19045 = CARTESIAN_POINT ( 'NONE',  ( 7.570916362186213000, 14.39999999999999680, -23.30088464923126423 ) ) ;
#19046 = CARTESIAN_POINT ( 'NONE',  ( 10.37757302488624056, 62.52500000273120406, -31.93888565452638417 ) ) ;
#19047 = CARTESIAN_POINT ( 'NONE',  ( -2.162160676586882350E-15, 56.87500000273117706, -35.31076352940722529 ) ) ;
#19048 = CARTESIAN_POINT ( 'NONE',  ( 18.94512977948576093, 12.82499999726882578, -13.76444248337722875 ) ) ;
#19049 = CARTESIAN_POINT ( 'NONE',  ( 19.82091636218621034, 3.799999999999998046, 14.40073868116559730 ) ) ;
#19050 = CARTESIAN_POINT ( 'NONE',  ( 10.37757302488624056, 2.525000002731203619, -31.93888565452638417 ) ) ;
#19051 = CARTESIAN_POINT ( 'NONE',  ( 7.025853678916403666, 38.07329833425730925, -26.06988505166735237 ) ) ;
#19052 = CARTESIAN_POINT ( 'NONE',  ( 5.779280353836490358E-15, 25.00000000546237899, 32.49999999999999289 ) ) ;
#19053 = CARTESIAN_POINT ( 'NONE',  ( 0.000000000000000000, 0.000000000000000000, 0.000000000000000000 ) ) ;
#19054 = CARTESIAN_POINT ( 'NONE',  ( 20.75514604977248467, 30.42500000273117777, -28.56700777964554305 ) ) ;
#19055 = CARTESIAN_POINT ( 'NONE',  ( -40.00000000000000711, 52.00000000000000711, 23.09401076758504345 ) ) ;
#19056 = DIRECTION ( 'NONE',  ( -1.224646799147353454E-16, 1.000000000000000000, -0.000000000000000000 ) ) ;
#19057 = CARTESIAN_POINT ( 'NONE',  ( 7.570916362186207671, 13.60000000000000142, 23.30088464923126779 ) ) ;
#19058 = CARTESIAN_POINT ( 'NONE',  ( 20.47846945139867003, 59.54649333240936215, -20.53372385742107653 ) ) ;
#19059 = CARTESIAN_POINT ( 'NONE',  ( -32.50000000000000000, 46.40000000546238113, -10.55989012756945478 ) ) ;
#19060 = DIRECTION ( 'NONE',  ( 0.000000000000000000, 1.000000000000000000, 0.000000000000000000 ) ) ;
#19061 = CARTESIAN_POINT ( 'NONE',  ( -26.07999730980477437, 25.17708333333332860, 6.988114217768305103 ) ) ;
#19062 = ORIENTED_EDGE ( 'NONE', *, *, #12725, .F. ) ;
#19063 = VECTOR ( 'NONE', #15789, 1000.000000000000000 ) ;
#19064 = CARTESIAN_POINT ( 'NONE',  ( 10.37757302488624056, 78.52500000273120406, -31.93888565452638417 ) ) ;
#19065 = CARTESIAN_POINT ( 'NONE',  ( 20.50609665440969565, 33.48437500000000000, -20.50609665441004736 ) ) ;
#19066 = CARTESIAN_POINT ( 'NONE',  ( -14.47279130897152299, 16.42499999726882720, 19.92008829642072243 ) ) ;
#19067 = VERTEX_POINT ( 'NONE', #2197 ) ;
#19068 = CARTESIAN_POINT ( 'NONE',  ( 7.468012846824777284, 53.25559000092396644, 28.02196122052045268 ) ) ;
#19069 = CARTESIAN_POINT ( 'NONE',  ( -2.092463501923844636E-15, 16.00000000546237544, -34.17252228774368916 ) ) ;
#19070 = CARTESIAN_POINT ( 'NONE',  ( 28.01184896238290278, 50.95833333333332860, -7.505752307973347470 ) ) ;
#19071 = CARTESIAN_POINT ( 'NONE',  ( -10.04305231718578462, 36.39999999999999147, 30.90933677959249337 ) ) ;
#19072 = CARTESIAN_POINT ( 'NONE',  ( -27.16883889988623935, 47.57500000273117990, 19.73931689729374739 ) ) ;
#19073 = CARTESIAN_POINT ( 'NONE',  ( 26.29305231718578995, 49.70000000546237118, -19.10302069950538240 ) ) ;
#19074 = EDGE_CURVE ( 'NONE', #22688, #10580, #20405, .T. ) ;
#19075 = CARTESIAN_POINT ( 'NONE',  ( 13.91746824999999532, 78.47500000273120691, -4.522059556121118540 ) ) ;
#19076 = CARTESIAN_POINT ( 'NONE',  ( 10.37757302488624056, 34.52500000273117564, -31.93888565452638417 ) ) ;
#19077 = DIRECTION ( 'NONE',  ( -0.000000000000000000, -1.000000000000000000, -0.000000000000000000 ) ) ;
#19078 = CARTESIAN_POINT ( 'NONE',  ( 33.58253175000000113, 64.47500000273120691, -10.91162601494193751 ) ) ;
#19079 = CARTESIAN_POINT ( 'NONE',  ( 6.277390505771533514E-15, 42.50000000000000000, 34.17252228774368916 ) ) ;
#19080 = CARTESIAN_POINT ( 'NONE',  ( 23.41746824999999887, 10.62499999726881938, 0.000000000000000000 ) ) ;
#19081 = CARTESIAN_POINT ( 'NONE',  ( 33.58253175000000113, 4.375000002731193938, -4.112674001490185761E-15 ) ) ;
#19082 = DIRECTION ( 'NONE',  ( 0.000000000000000000, 0.000000000000000000, -1.000000000000000000 ) ) ;
#19083 = CARTESIAN_POINT ( 'NONE',  ( 11.25946833292375793, 74.57500000273120122, -8.180482586598735395 ) ) ;
#19084 = CARTESIAN_POINT ( 'NONE',  ( -33.58253175000000113, 73.37500000273116996, 0.000000000000000000 ) ) ;
#19085 = CARTESIAN_POINT ( 'NONE',  ( 24.50000000000000000, 3.649999994537613812, 7.960532557706212486 ) ) ;
#19086 = APPLICATION_CONTEXT ( 'automotive_design' ) ;
#19087 = CARTESIAN_POINT ( 'NONE',  ( -27.16883889988624290, 69.17500000273118133, -19.73931689729374028 ) ) ;
#19088 = ORIENTED_EDGE ( 'NONE', *, *, #24946, .T. ) ;
#19089 = CARTESIAN_POINT ( 'NONE',  ( 0.000000000000000000, 16.99999999999998579, 0.000000000000000000 ) ) ;
#19090 = AXIS2_PLACEMENT_3D ( 'NONE', #11220, #32140, #4670 ) ;
#19091 = CARTESIAN_POINT ( 'NONE',  ( -19.09188309203660694, 66.14062500000000000, 19.09188309203694800 ) ) ;
#19092 = CARTESIAN_POINT ( 'NONE',  ( 4.412827539393359662E-15, -59.03347138510255832, 0.000000000000000000 ) ) ;
#19093 = CARTESIAN_POINT ( 'NONE',  ( -33.58253175000000113, 45.22500000273117848, 10.91162601494193929 ) ) ;
#19094 = CARTESIAN_POINT ( 'NONE',  ( 20.75514604977248467, 10.67500000273119021, -28.56700777964554305 ) ) ;
#19095 = CARTESIAN_POINT ( 'NONE',  ( -2.162160676586882350E-15, 60.87500000273117706, -35.31076352940722529 ) ) ;
#19096 = CARTESIAN_POINT ( 'NONE',  ( 19.09188309203694800, 51.53124999999999289, 19.09188309203660694 ) ) ;
#19097 = CARTESIAN_POINT ( 'NONE',  ( -20.47846945139902175, 40.93788166759063785, -20.53372385742072481 ) ) ;
#19098 = CARTESIAN_POINT ( 'NONE',  ( -15.04653450569338524, 27.89284749907601935, -25.98046417659831775 ) ) ;
#19099 = CARTESIAN_POINT ( 'NONE',  ( 20.08610463437157279, 65.80000000546237970, -27.64615127144129758 ) ) ;
#19100 = CARTESIAN_POINT ( 'NONE',  ( 3.980102097228898626E-15, 80.00000000000001421, 32.50000000000000000 ) ) ;
#19101 = CARTESIAN_POINT ( 'NONE',  ( 26.09010956794244507, 53.24440999907603356, 6.950374756619249084 ) ) ;
#19102 = CARTESIAN_POINT ( 'NONE',  ( -7.236395654485763274, 16.02499999726880731, 22.27133577429736633 ) ) ;
#19103 = CARTESIAN_POINT ( 'NONE',  ( 10.04305231718579705, 13.10000000546238041, 30.90933677959248982 ) ) ;
#19104 = ORIENTED_EDGE ( 'NONE', *, *, #31881, .T. ) ;
#19105 = CARTESIAN_POINT ( 'NONE',  ( -33.58253175000000113, 49.27500000273118985, -10.91162601494193218 ) ) ;
#19106 =( BOUNDED_CURVE ( )  B_SPLINE_CURVE ( 2, ( #6164, #3930, #29660, #671, #21630, #27271, #21960, #8738, #19223, #19389, #27438, #32076, #16317 ),
 .UNSPECIFIED., .F., .T. ) 
 B_SPLINE_CURVE_WITH_KNOTS ( ( 3, 2, 2, 2, 2, 2, 3 ),
 ( 0.9807692307692307265, 0.9820512820512820040, 0.9846153846153846700, 0.9871794871794872250, 0.9897435897435897800, 0.9923076923076923350, 0.9935897435897436125 ),
 .UNSPECIFIED. ) 
 CURVE ( )  GEOMETRIC_REPRESENTATION_ITEM ( )  RATIONAL_B_SPLINE_CURVE ( ( 0.9755282581475768211, 0.9755282581475768211, 1.000000000000000000, 0.9510565162951535312, 1.000000000000000000, 0.9510565162951535312, 1.000000000000000000, 0.9510565162951535312, 1.000000000000000000, 0.9510565162951535312, 1.000000000000000000, 0.9755282581475768211, 0.9755282581475768211 ) ) 
 REPRESENTATION_ITEM ( '' )  );
#19107 = CARTESIAN_POINT ( 'NONE',  ( -32.50000000000000000, 50.60000000546236265, 10.55989012756946366 ) ) ;
#19108 = CARTESIAN_POINT ( 'NONE',  ( -7.025853678916393008, 53.54204833425730925, 26.06988505166735592 ) ) ;
#19109 = CARTESIAN_POINT ( 'NONE',  ( -10.37757302488624411, 66.97500000273117848, -31.93888565452638417 ) ) ;
#19110 = ORIENTED_EDGE ( 'NONE', *, *, #31228, .T. ) ;
#19111 = CARTESIAN_POINT ( 'NONE',  ( 27.16883889988624290, 15.92500000273118488, 19.73931689729373673 ) ) ;
#19112 = CARTESIAN_POINT ( 'NONE',  ( 15.01150461594643204, 24.17447916666666785, 26.00068869287340334 ) ) ;
#19114 = ORIENTED_EDGE ( 'NONE', *, *, #26149, .F. ) ;
#19113 = EDGE_CURVE ( 'NONE', #14205, #19228, #18783, .T. ) ;
#19115 = CARTESIAN_POINT ( 'NONE',  ( -26.29305231718579350, 48.30000000546236549, -19.10302069950537884 ) ) ;
#19116 = CARTESIAN_POINT ( 'NONE',  ( -10.37757302488623701, 57.52500000273119696, 31.93888565452638417 ) ) ;
#19117 = CARTESIAN_POINT ( 'NONE',  ( 15.01150461594643204, 61.98697916666665009, 26.00068869287340334 ) ) ;
#19118 = EDGE_CURVE ( 'NONE', #12293, #23252, #5967, .T. ) ;
#19119 = CARTESIAN_POINT ( 'NONE',  ( 6.277390505771533514E-15, 19.00000000546236834, 34.17252228774368916 ) ) ;
#19120 = DIRECTION ( 'NONE',  ( 0.000000000000000000, 0.000000000000000000, 1.000000000000000000 ) ) ;
#19121 = CARTESIAN_POINT ( 'NONE',  ( 23.41746824999999887, 11.22499999726881548, -7.608796670333727974 ) ) ;
#19122 = CARTESIAN_POINT ( 'NONE',  ( -2.162160676586881955E-15, 20.87500000273119127, -35.31076352940723240 ) ) ;
#19123 = FILL_AREA_STYLE ('',( #17217 ) ) ;
#19124 = CARTESIAN_POINT ( 'NONE',  ( 13.94119854578893580, 14.71576416574268720, -24.22776226481265383 ) ) ;
#19125 = CARTESIAN_POINT ( 'NONE',  ( 0.000000000000000000, 0.000000000000000000, 26.50000000000000355 ) ) ;
#19126 = DIRECTION ( 'NONE',  ( 1.000000000000000000, 0.000000000000000000, 0.000000000000000000 ) ) ;
#19127 = CARTESIAN_POINT ( 'NONE',  ( -20.08610463437156923, 10.30000000000000782, 27.64615127144130113 ) ) ;
#19128 = VERTEX_POINT ( 'NONE', #20064 ) ;
#19129 = CARTESIAN_POINT ( 'NONE',  ( -4.732186688966233175E-15, 19.24999999453761745, 25.76082449383753925 ) ) ;
#19130 = CARTESIAN_POINT ( 'NONE',  ( 8.601468415847516980, 74.17500000273119554, -11.83890561707634781 ) ) ;
#19131 = CARTESIAN_POINT ( 'NONE',  ( -27.95245687107222921, 39.07031249999997868, 2.498001805406602216E-13 ) ) ;
#19132 = CARTESIAN_POINT ( 'NONE',  ( -10.37757302488624411, 22.72500000273119980, -31.93888565452638417 ) ) ;
#19133 = CARTESIAN_POINT ( 'NONE',  ( 10.37757302488624767, 63.72500000273119269, 31.93888565452638417 ) ) ;
#19134 = CARTESIAN_POINT ( 'NONE',  ( -33.58253175000000113, 27.47500000273118204, 10.91162601494193929 ) ) ;
#19135 = CARTESIAN_POINT ( 'NONE',  ( -2.162160676586881955E-15, 16.87500000273120193, -35.31076352940723240 ) ) ;
#19136 = CARTESIAN_POINT ( 'NONE',  ( -27.16883889988624290, 9.175000002731191984, -19.73931689729374028 ) ) ;
#19137 = CARTESIAN_POINT ( 'NONE',  ( 7.025853678916403666, 62.13579833425730925, -26.06988505166735237 ) ) ;
#19138 = CARTESIAN_POINT ( 'NONE',  ( 33.58253175000000823, 72.02500000273118985, 10.91162601494192685 ) ) ;
#19139 = CARTESIAN_POINT ( 'NONE',  ( -26.00068869287340334, 52.53385416666666430, 15.01150461594643382 ) ) ;
#19140 = LINE ( 'NONE', #13983, #8535 ) ;
#19141 = CARTESIAN_POINT ( 'NONE',  ( 4.300734207923761154, 77.97500000273119269, 13.23629886949340495 ) ) ;
#19142 = CARTESIAN_POINT ( 'NONE',  ( 10.04305231718579705, 52.60000000000002274, 30.90933677959248982 ) ) ;
#19143 = CARTESIAN_POINT ( 'NONE',  ( 10.37757302488624056, 60.52500000273119696, -31.93888565452638417 ) ) ;
#19144 = CARTESIAN_POINT ( 'NONE',  ( -7.236395654485763274, 16.52499999726880731, 22.27133577429736633 ) ) ;
#19145 =( BOUNDED_CURVE ( )  B_SPLINE_CURVE ( 2, ( #18380, #18548, #5324, #15804, #20620, #5493, #33641, #4983, #17869, #154, #10138, #26260, #2748 ),
 .UNSPECIFIED., .F., .F. ) 
 B_SPLINE_CURVE_WITH_KNOTS ( ( 3, 2, 2, 2, 2, 2, 3 ),
 ( 0.08333333333333334259, 0.08461538461538462008, 0.08717948717948717507, 0.08974358974358974395, 0.09230769230769231282, 0.09487179487179486781, 0.09615384615384615918 ),
 .UNSPECIFIED. ) 
 CURVE ( )  GEOMETRIC_REPRESENTATION_ITEM ( )  RATIONAL_B_SPLINE_CURVE ( ( 0.9755282581475767101, 0.9755282581475768211, 1.000000000000000000, 0.9510565162951535312, 1.000000000000000000, 0.9510565162951535312, 1.000000000000000000, 0.9510565162951535312, 1.000000000000000000, 0.9510565162951535312, 1.000000000000000000, 0.9755282581475765991, 0.9755282581475767101 ) ) 
 REPRESENTATION_ITEM ( '' )  );
#19146 = ORIENTED_EDGE ( 'NONE', *, *, #5812, .F. ) ;
#19147 = CARTESIAN_POINT ( 'NONE',  ( 33.58253175000000113, 66.37500000273121259, -4.112674001490185761E-15 ) ) ;
#19148 = CARTESIAN_POINT ( 'NONE',  ( 27.16883889988624290, 1.925000002731186433, 19.73931689729373673 ) ) ;
#19149 = CARTESIAN_POINT ( 'NONE',  ( 23.41746825000000243, 4.724999997268818142, -7.608796670333727974 ) ) ;
#19150 = CARTESIAN_POINT ( 'NONE',  ( 13.94119854578937812, 25.61236083425731636, 24.22776226481240514 ) ) ;
#19151 = VERTEX_POINT ( 'NONE', #13359 ) ;
#19152 = CARTESIAN_POINT ( 'NONE',  ( -10.37757302488624411, 34.72500000273119269, -31.93888565452638417 ) ) ;
#19153 = CARTESIAN_POINT ( 'NONE',  ( -4.934616302121927505E-14, 69.00000000546236834, 32.50000000000000000 ) ) ;
#19154 = ORIENTED_EDGE ( 'NONE', *, *, #19026, .T. ) ;
#19155 = CARTESIAN_POINT ( 'NONE',  ( -28.01184896238304134, 52.96354166666666430, -7.505752307972844761 ) ) ;
#19156 = CARTESIAN_POINT ( 'NONE',  ( 26.29305231718578995, 11.70000000546239605, -19.10302069950538240 ) ) ;
#19157 = DIRECTION ( 'NONE',  ( 0.000000000000000000, 0.000000000000000000, -1.000000000000000000 ) ) ;
#19158 = CARTESIAN_POINT ( 'NONE',  ( -20.75514604977248823, 74.82500000273115859, -28.56700777964554305 ) ) ;
#19159 = CARTESIAN_POINT ( 'NONE',  ( 2.740863092043355209E-13, 34.77343750000000000, 30.02300923189239512 ) ) ;
#19160 = CARTESIAN_POINT ( 'NONE',  ( 1.577395562988744260E-15, 4.500000000000003553, -25.76082449383753925 ) ) ;
#19161 = EDGE_CURVE ( 'NONE', #29590, #30543, #33107, .T. ) ;
#19162 = CARTESIAN_POINT ( 'NONE',  ( -2.162160676586881955E-15, 6.875000002731195714, -35.31076352940723240 ) ) ;
#19163 = ADVANCED_FACE ( 'NONE', ( #31203 ), #26569, .T. ) ;
#19164 = CARTESIAN_POINT ( 'NONE',  ( 33.58253175000000823, 18.02500000273118630, 10.91162601494192863 ) ) ;
#19165 = CARTESIAN_POINT ( 'NONE',  ( -8.960552108402744065E-16, 76.37500000273116996, -14.63369212191046209 ) ) ;
#19166 = CARTESIAN_POINT ( 'NONE',  ( 2.375766604868040144, 76.80125428700922896, 15.00000000000000178 ) ) ;
#19167 = CARTESIAN_POINT ( 'NONE',  ( 30.02300923189239867, 42.78868083240935505, -0.04044903255044467877 ) ) ;
#19168 = CARTESIAN_POINT ( 'NONE',  ( -9.657523855033125146E-16, 81.50000000000002842, -15.77193336357400710 ) ) ;
#19169 = CARTESIAN_POINT ( 'NONE',  ( 2.740863092043355209E-13, 48.52343749999999289, 30.02300923189239867 ) ) ;
#19170 = DIRECTION ( 'NONE',  ( 0.000000000000000000, 1.000000000000000000, 0.000000000000000000 ) ) ;
#19171 = CARTESIAN_POINT ( 'NONE',  ( 26.29305231718578995, 71.19999999999998863, -19.10302069950538240 ) ) ;
#19172 = CARTESIAN_POINT ( 'NONE',  ( -2.428612866367529427E-13, 15.86718749999999645, -27.95245687107222921 ) ) ;
#19173 = CARTESIAN_POINT ( 'NONE',  ( 33.58253175000000823, 42.02500000273118985, 10.91162601494192863 ) ) ;
#19174 = CARTESIAN_POINT ( 'NONE',  ( -8.601468415847515203, 73.17500000273119554, 11.83890561707634959 ) ) ;
#19175 = CARTESIAN_POINT ( 'NONE',  ( 20.75514604977248467, 46.67500000273118133, -28.56700777964554305 ) ) ;
#19176 = CARTESIAN_POINT ( 'NONE',  ( -10.37757302488623701, 25.77500000273119696, 31.93888565452638417 ) ) ;
#19177 = CARTESIAN_POINT ( 'NONE',  ( -15.82193040522741967, 16.99999999999999645, 18.67333929100095347 ) ) ;
#19178 = CARTESIAN_POINT ( 'NONE',  ( -24.20753774853730889, 18.15885416666666075, 13.97622843553634020 ) ) ;
#19179 = CARTESIAN_POINT ( 'NONE',  ( 1.102182119232617911E-15, 74.00000000000001421, 9.000000000000001776 ) ) ;
#19180 = CARTESIAN_POINT ( 'NONE',  ( 10.04305231718579705, 74.59999999999998010, 30.90933677959248982 ) ) ;
#19181 = CARTESIAN_POINT ( 'NONE',  ( 6.486482029760649416E-15, 7.625000002731185056, 35.31076352940723240 ) ) ;
#19182 = CARTESIAN_POINT ( 'NONE',  ( -4.523095164977117273E-15, 4.124999997268806951, 24.62258325217400312 ) ) ;
#19183 = CYLINDRICAL_SURFACE ( 'NONE', #29695, 26.50000000000000355 ) ;
#19184 = CARTESIAN_POINT ( 'NONE',  ( -7.025853678916861966, 28.03607666574268364, -26.06988505166722803 ) ) ;
#19185 = CARTESIAN_POINT ( 'NONE',  ( 1.555960095263670572E-15, 12.50000000000000355, -24.50000000000000000 ) ) ;
#19186 = CARTESIAN_POINT ( 'NONE',  ( -33.58253175000000113, 21.02500000273118275, -10.91162601494193041 ) ) ;
#19187 = CARTESIAN_POINT ( 'NONE',  ( 23.41746825000000243, 3.024999997268812635, 7.608796670333735079 ) ) ;
#19188 = CARTESIAN_POINT ( 'NONE',  ( 2.584737979205441561E-13, 51.96093750000000000, 27.95245687107222921 ) ) ;
#19189 = ORIENTED_EDGE ( 'NONE', *, *, #28085, .T. ) ;
#19190 = CARTESIAN_POINT ( 'NONE',  ( -27.16883889988623935, 55.32500000273120122, 19.73931689729374739 ) ) ;
#19191 = ORIENTED_EDGE ( 'NONE', *, *, #31468, .F. ) ;
#19192 = CARTESIAN_POINT ( 'NONE',  ( -28.01184896238304134, 22.02604166666666430, -7.505752307972844761 ) ) ;
#19193 = CARTESIAN_POINT ( 'NONE',  ( 7.468012846824777284, 25.75559000092397710, 28.02196122052045268 ) ) ;
#19194 = CARTESIAN_POINT ( 'NONE',  ( 32.50000000000000000, 39.00000000000000711, -3.980102097228898626E-15 ) ) ;
#19195 = CARTESIAN_POINT ( 'NONE',  ( -14.47279130897152122, 3.924999997268813434, 19.92008829642072243 ) ) ;
#19196 = CARTESIAN_POINT ( 'NONE',  ( -33.58253175000000113, 27.37500000273118772, 0.000000000000000000 ) ) ;
#19197 = CARTESIAN_POINT ( 'NONE',  ( -20.08610463437157989, 28.20000000546236762, -27.64615127144129758 ) ) ;
#19198 = CARTESIAN_POINT ( 'NONE',  ( 10.04305231718579705, 74.59999999999999432, 30.90933677959248982 ) ) ;
#19199 = DIRECTION ( 'NONE',  ( 0.000000000000000000, 1.000000000000000000, 0.000000000000000000 ) ) ;
#19200 = DIRECTION ( 'NONE',  ( 0.000000000000000000, 0.000000000000000000, -1.000000000000000000 ) ) ;
#19201 = CARTESIAN_POINT ( 'NONE',  ( 7.543491769121427382, 51.82329833425730925, -28.00173670424548433 ) ) ;
#19202 = CARTESIAN_POINT ( 'NONE',  ( -33.58253175000000113, 41.27500000273117564, -10.91162601494193218 ) ) ;
#19203 = PRODUCT_DEFINITION_FORMATION_WITH_SPECIFIED_SOURCE ( 'ANY', '', #7096, .NOT_KNOWN. ) ;
#19204 =( BOUNDED_CURVE ( )  B_SPLINE_CURVE ( 2, ( #24967, #1449, #6775, #29943, #12092, #29769, #9338 ),
 .UNSPECIFIED., .F., .T. ) 
 B_SPLINE_CURVE_WITH_KNOTS ( ( 3, 2, 2, 3 ),
 ( 0.9935897435897436125, 0.9948717948717948900, 0.9974358974358974450, 1.000000000000000000 ),
 .UNSPECIFIED. ) 
 CURVE ( )  GEOMETRIC_REPRESENTATION_ITEM ( )  RATIONAL_B_SPLINE_CURVE ( ( 0.9755282581475768211, 0.9755282581475768211, 1.000000000000000000, 0.9510565162951535312, 1.000000000000000000, 0.9510565162951535312, 1.000000000000000000 ) ) 
 REPRESENTATION_ITEM ( '' )  );
#19205 = CARTESIAN_POINT ( 'NONE',  ( 23.41746825000000243, 7.224999997268826135, -7.608796670333727974 ) ) ;
#19206 = CARTESIAN_POINT ( 'NONE',  ( -20.08610463437156923, 18.30000000000000782, 27.64615127144130113 ) ) ;
#19207 = CARTESIAN_POINT ( 'NONE',  ( -24.50000000000000000, 11.00000000000001066, -3.000384657911015469E-15 ) ) ;
#19208 = CARTESIAN_POINT ( 'NONE',  ( 13.94119854578893580, 38.77826416574269075, -24.22776226481265383 ) ) ;
#19209 =( BOUNDED_CURVE ( )  B_SPLINE_CURVE ( 2, ( #4377, #10047, #30971, #17432, #7470, #31145, #17599, #30796, #17953, #4209, #20177, #4891, #1790 ),
 .UNSPECIFIED., .F., .F. ) 
 B_SPLINE_CURVE_WITH_KNOTS ( ( 3, 2, 2, 2, 2, 2, 3 ),
 ( 0.7500000000000000000, 0.7512820512820512775, 0.7538461538461538325, 0.7564102564102563875, 0.7589743589743589425, 0.7615384615384614975, 0.7628205128205127750 ),
 .UNSPECIFIED. ) 
 CURVE ( )  GEOMETRIC_REPRESENTATION_ITEM ( )  RATIONAL_B_SPLINE_CURVE ( ( 0.9755282581475768211, 0.9755282581475768211, 1.000000000000000000, 0.9510565162951535312, 1.000000000000000000, 0.9510565162951535312, 1.000000000000000000, 0.9510565162951535312, 1.000000000000000000, 0.9510565162951535312, 1.000000000000000000, 0.9755282581475768211, 0.9755282581475768211 ) ) 
 REPRESENTATION_ITEM ( '' )  );
#19210 = CARTESIAN_POINT ( 'NONE',  ( -10.37757302488623701, 65.52500000273120406, 31.93888565452638417 ) ) ;
#19211 = CARTESIAN_POINT ( 'NONE',  ( -27.16883889988623935, 53.57500000273118701, 19.73931689729374739 ) ) ;
#19212 = CARTESIAN_POINT ( 'NONE',  ( -14.47279130897151767, 9.324999997268816898, -19.92008829642072598 ) ) ;
#19213 = B_SPLINE_CURVE_WITH_KNOTS ( 'NONE', 3,
 ( #28881, #42, #16028, #21007, #5719, #13103, #18605, #10363, #23409, #20841, #26314, #10530, #31456, #26144, #2803, #28540, #7612, #12933, #16197, #18437, #26483, #13270, #21345, #25973, #10199, #33698, #7950, #2977, #13446, #23745, #8277, #23913, #209, #5036, #5379, #31286, #15858, #5547, #20679, #10697, #2640, #7779, #18266, #21178 ),
 .UNSPECIFIED., .F., .F.,
 ( 4, 2, 2, 2, 2, 2, 2, 2, 2, 2, 2, 2, 2, 2, 2, 2, 2, 2, 2, 2, 2, 4 ),
 ( 0.000000000000000000, 0.004057857163981401158, 0.008115714327962802316, 0.01217357149194420000, 0.01420250007393489972, 0.01623142865592559769, 0.02028928581990698324, 0.02231821440189768121, 0.02434714298388837572, 0.02840500014786977862, 0.03246285731185117457, 0.03652071447583257052, 0.03854964305782326156, 0.04057857163981395260, 0.04463642880379534855, 0.04869428596777673757, 0.05072321454976744248, 0.05275214313175814740, 0.05681000029573955029, 0.05883892887773024827, 0.06086785745972094624, 0.06492571462370234914 ),
 .UNSPECIFIED. ) ;
#19214 = CARTESIAN_POINT ( 'NONE',  ( -7.570916362186215665, 9.399999999999991473, 23.30088464923126423 ) ) ;
#19215 = CARTESIAN_POINT ( 'NONE',  ( 6.486482029760649416E-15, 3.625000002731181059, 35.31076352940723240 ) ) ;
#19216 = CARTESIAN_POINT ( 'NONE',  ( 19.11951029504763611, 41.79725666759063785, -19.06425588902591173 ) ) ;
#19217 = CARTESIAN_POINT ( 'NONE',  ( 0.000000000000000000, 80.00000000000001421, 0.000000000000000000 ) ) ;
#19218 = DIRECTION ( 'NONE',  ( 0.000000000000000000, 0.000000000000000000, -1.000000000000000000 ) ) ;
#19219 = CARTESIAN_POINT ( 'NONE',  ( 20.75514604977249178, 27.82500000273116925, 28.56700777964553950 ) ) ;
#19220 = CYLINDRICAL_SURFACE ( 'NONE', #11653, 15.00000000000000000 ) ;
#19221 = DIRECTION ( 'NONE',  ( 0.8660254037844410391, -0.4999999999999958367, -0.000000000000000000 ) ) ;
#19222 = ADVANCED_FACE ( 'NONE', ( #3065 ), #5462, .T. ) ;
#19223 = CARTESIAN_POINT ( 'NONE',  ( 26.29305231718579350, 1.300000005462376151, 19.10302069950537529 ) ) ;
#19224 = CARTESIAN_POINT ( 'NONE',  ( -14.97647472619899389, 57.68451416574269075, 26.02091320914878025 ) ) ;
#19225 = CARTESIAN_POINT ( 'NONE',  ( 6.277390505771533514E-15, 47.00000000546238965, 34.17252228774368916 ) ) ;
#19226 = CARTESIAN_POINT ( 'NONE',  ( -8.601468415847518756, 73.07500000273118701, -11.83890561707634781 ) ) ;
#19227 = CARTESIAN_POINT ( 'NONE',  ( 26.07999730980490227, 30.61979166666666075, 6.988114217767821046 ) ) ;
#19228 = VERTEX_POINT ( 'NONE', #7694 ) ;
#19229 = CARTESIAN_POINT ( 'NONE',  ( 6.486482029760649416E-15, 77.62500000273121259, 35.31076352940723240 ) ) ;
#19230 = CARTESIAN_POINT ( 'NONE',  ( 30.02300923189239512, 30.47656250000000355, -2.619432448724977703E-13 ) ) ;
#19231 = DIRECTION ( 'NONE',  ( -0.7071067811865526798, 0.000000000000000000, -0.7071067811865423547 ) ) ;
#19232 = ORIENTED_EDGE ( 'NONE', *, *, #10938, .F. ) ;
#19233 = CARTESIAN_POINT ( 'NONE',  ( -0.04044903254990864921, 46.52381916759065206, 30.02300923189239867 ) ) ;
#19234 = CARTESIAN_POINT ( 'NONE',  ( -32.50000000000000000, 8.500000005462373664, 0.000000000000000000 ) ) ;
#19235 = CARTESIAN_POINT ( 'NONE',  ( 26.00068869287340334, 57.69010416666667140, -15.01150461594642316 ) ) ;
#19236 = CARTESIAN_POINT ( 'NONE',  ( 5.779280353836490358E-15, 47.00000000546238255, 32.49999999999999289 ) ) ;
#19237 = CARTESIAN_POINT ( 'NONE',  ( 33.58253175000000823, 50.27500000273118985, 10.91162601494192863 ) ) ;
#19238 = CARTESIAN_POINT ( 'NONE',  ( -32.50000000000000000, 48.60000000546236976, 10.55989012756946366 ) ) ;
#19239 = CARTESIAN_POINT ( 'NONE',  ( 8.601468415847516980, 78.67500000273119554, -11.83890561707634781 ) ) ;
#19240 = CARTESIAN_POINT ( 'NONE',  ( 20.75514604977248467, 38.42500000273118133, -28.56700777964554305 ) ) ;
#19241 = CARTESIAN_POINT ( 'NONE',  ( 20.08610463437158344, 77.20000000546238539, 27.64615127144129403 ) ) ;
#19242 = CARTESIAN_POINT ( 'NONE',  ( 27.16883889988624290, 64.17500000273118133, 19.73931689729373673 ) ) ;
#19243 = CARTESIAN_POINT ( 'NONE',  ( 20.08610463437158344, 38.70000000000000284, 27.64615127144129403 ) ) ;
#19244 = CARTESIAN_POINT ( 'NONE',  ( 23.41746824999999887, 12.62499999726882116, 0.000000000000000000 ) ) ;
#19245 = CARTESIAN_POINT ( 'NONE',  ( 20.75514604977248467, 6.675000002731201754, -28.56700777964554305 ) ) ;
#19246 = DIRECTION ( 'NONE',  ( 0.000000000000000000, -1.000000000000000000, 0.000000000000000000 ) ) ;
#19247 = CARTESIAN_POINT ( 'NONE',  ( 2.688165632520823219E-15, 77.87500000273119838, 14.63369212191046209 ) ) ;
#19248 = CARTESIAN_POINT ( 'NONE',  ( -33.58253175000000113, 75.37500000273116996, 0.000000000000000000 ) ) ;
#19249 = CARTESIAN_POINT ( 'NONE',  ( -1.778240108872766143E-15, 59.50000000000000711, -32.49999999999999289 ) ) ;
#19250 = CARTESIAN_POINT ( 'NONE',  ( 27.16883889988624290, 68.17500000273118133, 19.73931689729373673 ) ) ;
#19251 = VERTEX_POINT ( 'NONE', #15943 ) ;
#19252 = CARTESIAN_POINT ( 'NONE',  ( -7.570916362186210335, 2.349999994537638415, -23.30088464923126779 ) ) ;
#19253 = CARTESIAN_POINT ( 'NONE',  ( 26.07999730980477437, 64.70833333333334281, -6.988114217768290004 ) ) ;
#19254 = CARTESIAN_POINT ( 'NONE',  ( 15.00000000000000000, 75.00000000000001421, -1.836970198721029589E-15 ) ) ;
#19255 = CARTESIAN_POINT ( 'NONE',  ( 27.16883889988624290, 45.92500000273118133, 19.73931689729373673 ) ) ;
#19256 = CARTESIAN_POINT ( 'NONE',  ( -20.75514604977248823, 9.075000002731183457, -28.56700777964554305 ) ) ;
#19257 = CARTESIAN_POINT ( 'NONE',  ( -33.58253175000000113, 65.37500000273121259, 0.000000000000000000 ) ) ;
#19258 = CARTESIAN_POINT ( 'NONE',  ( 27.95245687107223276, 47.66406249999999289, -2.463307335887066074E-13 ) ) ;
#19259 = CARTESIAN_POINT ( 'NONE',  ( -20.47846945139902175, 37.50038166759063074, -20.53372385742072481 ) ) ;
#19260 = CARTESIAN_POINT ( 'NONE',  ( -30.02300923189239867, 27.31993083240935505, 0.04044903255044988294 ) ) ;
#19261 = CARTESIAN_POINT ( 'NONE',  ( -32.50000000000000000, 70.50000000546239676, 0.000000000000000000 ) ) ;
#19262 = VECTOR ( 'NONE', #25249, 1000.000000000000000 ) ;
#19263 = CARTESIAN_POINT ( 'NONE',  ( -8.601468415847518756, 80.57500000273118701, -11.83890561707634781 ) ) ;
#19264 = CARTESIAN_POINT ( 'NONE',  ( 19.06425588902558133, 59.54649333240936215, -19.11951029504797006 ) ) ;
#19265 = CARTESIAN_POINT ( 'NONE',  ( 14.47279130897151589, 14.32499999726880624, 19.92008829642072953 ) ) ;
#19266 = CARTESIAN_POINT ( 'NONE',  ( 32.50000000000000711, 58.90000000000000568, 10.55989012756945122 ) ) ;
#19267 = EDGE_LOOP ( 'NONE', ( #11951, #11866, #26744, #2306 ) ) ;
#19268 = CARTESIAN_POINT ( 'NONE',  ( -20.75514604977248112, 45.67500000273119554, 28.56700777964554661 ) ) ;
#19269 = CARTESIAN_POINT ( 'NONE',  ( 14.47279130897151944, 1.424999997268804997, -19.92008829642072598 ) ) ;
#19270 = AXIS2_PLACEMENT_3D ( 'NONE', #4023, #28390, #33881 ) ;
#19271 = CARTESIAN_POINT ( 'NONE',  ( 7.025853678916403666, 51.82329833425730925, -26.06988505166735237 ) ) ;
#19272 = CARTESIAN_POINT ( 'NONE',  ( -27.16883889988623935, 71.57500000273120122, 19.73931689729374739 ) ) ;
#19273 = ORIENTED_EDGE ( 'NONE', *, *, #28135, .F. ) ;
#19274 = CARTESIAN_POINT ( 'NONE',  ( -20.75514604977248112, 17.42500000273117777, 28.56700777964554661 ) ) ;
#19275 = CARTESIAN_POINT ( 'NONE',  ( 7.505752307972854531, 26.32291666666666075, -28.01184896238303423 ) ) ;
#19276 = ORIENTED_EDGE ( 'NONE', *, *, #3804, .F. ) ;
#19277 = CARTESIAN_POINT ( 'NONE',  ( 26.29305231718579350, 65.30000000546237970, 19.10302069950537529 ) ) ;
#19278 = CARTESIAN_POINT ( 'NONE',  ( 20.75514604977249178, 53.82500000273119412, 28.56700777964553950 ) ) ;
#19279 = CARTESIAN_POINT ( 'NONE',  ( 30.02300923189239512, 61.41406250000000711, -2.619432448724977703E-13 ) ) ;
#19280 = CARTESIAN_POINT ( 'NONE',  ( -20.08610463437156923, 10.80000000546236549, 27.64615127144130113 ) ) ;
#19281 = CARTESIAN_POINT ( 'NONE',  ( 24.50000000000000000, 15.74999999453763344, 0.000000000000000000 ) ) ;
#19282 = CARTESIAN_POINT ( 'NONE',  ( 23.41746824999999887, 17.22499999726879594, -7.608796670333727974 ) ) ;
#19283 = CARTESIAN_POINT ( 'NONE',  ( 10.37757302488624056, 24.77500000273119696, -31.93888565452638417 ) ) ;
#19284 = CARTESIAN_POINT ( 'NONE',  ( -26.29305231718578995, 24.70000000546238184, 19.10302069950538595 ) ) ;
#19285 = CARTESIAN_POINT ( 'NONE',  ( -7.468012846824272799, 67.85378499907602645, 28.02196122052058413 ) ) ;
#19286 = CARTESIAN_POINT ( 'NONE',  ( -11.25946833292375793, 74.67500000273119554, -8.180482586598733619 ) ) ;
#19287 = CARTESIAN_POINT ( 'NONE',  ( 20.08610463437158344, 64.70000000000001705, 27.64615127144129403 ) ) ;
#19288 = CARTESIAN_POINT ( 'NONE',  ( 4.445600272181915325E-13, 15.49999999999999822, -32.50000000000000000 ) ) ;
#19289 = CARTESIAN_POINT ( 'NONE',  ( 32.50000000000000000, 13.09999999999999432, -10.55989012756945833 ) ) ;
#19290 = ORIENTED_EDGE ( 'NONE', *, *, #17767, .T. ) ;
#19291 = CARTESIAN_POINT ( 'NONE',  ( -18.94512977948576093, 6.324999997268820451, 13.76444248337722698 ) ) ;
#19292 = CARTESIAN_POINT ( 'NONE',  ( 11.25946833292375793, 75.67500000273119554, 8.180482586598731842 ) ) ;
#19293 = CARTESIAN_POINT ( 'NONE',  ( 19.09188309203694800, 44.65624999999999289, 19.09188309203660694 ) ) ;
#19294 = CARTESIAN_POINT ( 'NONE',  ( -2.162160676586881955E-15, 18.62500000273117351, -35.31076352940723240 ) ) ;
#19295 = CARTESIAN_POINT ( 'NONE',  ( -33.58253175000000113, 69.12500000273118417, 0.000000000000000000 ) ) ;
#19296 = CARTESIAN_POINT ( 'NONE',  ( -27.16883889988623935, 31.57500000273118346, 19.73931689729374739 ) ) ;
#19297 = CARTESIAN_POINT ( 'NONE',  ( -20.75514604977248112, 15.67500000273117600, 28.56700777964554661 ) ) ;
#19298 = CARTESIAN_POINT ( 'NONE',  ( 20.75514604977248467, 6.675000002731200865, -28.56700777964554305 ) ) ;
#19299 = CARTESIAN_POINT ( 'NONE',  ( -19.11951029504763611, 64.14100666759063074, 19.06425588902592239 ) ) ;
#19300 = CARTESIAN_POINT ( 'NONE',  ( -26.00068869287368756, 53.10677083333331439, -15.01150461594595775 ) ) ;
#19301 = CYLINDRICAL_SURFACE ( 'NONE', #20419, 24.50000000000000000 ) ;
#19302 = EDGE_CURVE ( 'NONE', #25891, #10457, #17672, .T. ) ;
#19303 =( BOUNDED_CURVE ( )  B_SPLINE_CURVE ( 2, ( #18217, #13216, #2415, #28996, #16148, #21298, #31568 ),
 .UNSPECIFIED., .F., .F. ) 
 B_SPLINE_CURVE_WITH_KNOTS ( ( 3, 2, 2, 3 ),
 ( 0.000000000000000000, 0.01111111111111111154, 0.02222222222222222307, 0.02777777777777777624 ),
 .UNSPECIFIED. ) 
 CURVE ( )  GEOMETRIC_REPRESENTATION_ITEM ( )  RATIONAL_B_SPLINE_CURVE ( ( 1.000000000000000000, 0.9510565162951535312, 1.000000000000000000, 0.9510565162951535312, 1.000000000000000000, 0.9755282581475768211, 0.9755282581475768211 ) ) 
 REPRESENTATION_ITEM ( '' )  );
#19304 = CARTESIAN_POINT ( 'NONE',  ( -8.601468415847518756, 75.07500000273118701, -11.83890561707634603 ) ) ;
#19305 = CARTESIAN_POINT ( 'NONE',  ( -10.04305231718579172, 47.60000000000001563, -30.90933677959248982 ) ) ;
#19306 = FACE_OUTER_BOUND ( 'NONE', #23071, .T. ) ;
#19307 = CARTESIAN_POINT ( 'NONE',  ( -2.162160676586882350E-15, 48.62500000273118417, -35.31076352940722529 ) ) ;
#19308 = EDGE_CURVE ( 'NONE', #30741, #29542, #3758, .T. ) ;
#19309 = CARTESIAN_POINT ( 'NONE',  ( 18.94512977948576093, 13.32499999726879913, -13.76444248337722875 ) ) ;
#19310 = ORIENTED_EDGE ( 'NONE', *, *, #7949, .T. ) ;
#19311 = CARTESIAN_POINT ( 'NONE',  ( -27.16883889988624290, 65.17500000273116711, -19.73931689729374028 ) ) ;
#19312 = CARTESIAN_POINT ( 'NONE',  ( -5.147494310547423346, 62.44874571845315359, 32.50000000000000000 ) ) ;
#19313 = CARTESIAN_POINT ( 'NONE',  ( -18.94512977948575738, 7.424999997268811214, -13.76444248337723231 ) ) ;
#19314 = CARTESIAN_POINT ( 'NONE',  ( -19.06425588902591173, 27.18788166759063785, -19.11951029504763611 ) ) ;
#19315 = ORIENTED_EDGE ( 'NONE', *, *, #9555, .T. ) ;
#19316 = CARTESIAN_POINT ( 'NONE',  ( 20.75514604977249178, 35.82500000273117990, 28.56700777964553950 ) ) ;
#19317 = CARTESIAN_POINT ( 'NONE',  ( -3.880418787951138260, 1.448745718453166020, 24.50000000000000000 ) ) ;
#19318 = ORIENTED_EDGE ( 'NONE', *, *, #12937, .T. ) ;
#19319 = CARTESIAN_POINT ( 'NONE',  ( -15.01150461594642138, 49.95572916666665009, -26.00068869287340334 ) ) ;
#19320 = CARTESIAN_POINT ( 'NONE',  ( 10.37757302488624767, 61.97500000273120691, 31.93888565452638417 ) ) ;
#19321 = CARTESIAN_POINT ( 'NONE',  ( 26.29305231718578995, 69.70000000546238539, -19.10302069950538240 ) ) ;
#19322 = CARTESIAN_POINT ( 'NONE',  ( -2.162160676586881955E-15, 72.62500000273118417, -35.31076352940723240 ) ) ;
#19323 = CARTESIAN_POINT ( 'NONE',  ( -26.00068869287368756, 29.04427083333332504, -15.01150461594595775 ) ) ;
#19324 = CARTESIAN_POINT ( 'NONE',  ( -7.570916362186210335, 6.599999999999994316, -23.30088464923126779 ) ) ;
#19325 = DIRECTION ( 'NONE',  ( -0.000000000000000000, -1.000000000000000000, -0.000000000000000000 ) ) ;
#19326 = CARTESIAN_POINT ( 'NONE',  ( -20.75514604977248112, 19.42500000273117777, 28.56700777964554661 ) ) ;
#19327 = CARTESIAN_POINT ( 'NONE',  ( 2.688165632520823219E-15, 71.37500000273119838, 14.63369212191046209 ) ) ;
#19328 = CARTESIAN_POINT ( 'NONE',  ( 0.04044903255045854962, 47.08555583240935505, 30.02300923189239867 ) ) ;
#19329 = CARTESIAN_POINT ( 'NONE',  ( 9.270509831248425314, 80.69999999999998863, 12.75976212528059683 ) ) ;
#19330 = CARTESIAN_POINT ( 'NONE',  ( 7.505752307972854531, 50.38541666666666430, -28.01184896238303423 ) ) ;
#19331 = CARTESIAN_POINT ( 'NONE',  ( -19.82091636218621034, 16.54999999453762882, -14.40073868116559552 ) ) ;
#19332 = CARTESIAN_POINT ( 'NONE',  ( -5.147494310547423346, 54.94874572391554324, 32.50000000000000000 ) ) ;
#19333 = CARTESIAN_POINT ( 'NONE',  ( 27.95245687107222921, 13.28906249999999289, -2.463307335887066074E-13 ) ) ;
#19334 = CARTESIAN_POINT ( 'NONE',  ( -27.16883889988623935, 43.32500000273120833, 19.73931689729374739 ) ) ;
#19335 = AXIS2_PLACEMENT_3D ( 'NONE', #17654, #15425, #4602 ) ;
#19336 = CARTESIAN_POINT ( 'NONE',  ( 2.688165632520823219E-15, 73.37500000273118417, 14.63369212191046387 ) ) ;
#19337 = CARTESIAN_POINT ( 'NONE',  ( 10.37757302488624056, 46.77500000273120406, -31.93888565452638417 ) ) ;
#19338 = CARTESIAN_POINT ( 'NONE',  ( 27.16883889988624290, 30.17500000273118488, 19.73931689729373673 ) ) ;
#19339 = DIRECTION ( 'NONE',  ( 0.8660254037844410391, 0.4999999999999958367, 0.000000000000000000 ) ) ;
#19340 = AXIS2_PLACEMENT_3D ( 'NONE', #31258, #28351, #7751 ) ;
#19341 = CARTESIAN_POINT ( 'NONE',  ( -24.20753774853756823, 18.73177083333332504, -13.97622843553588723 ) ) ;
#19342 = DIRECTION ( 'NONE',  ( 0.000000000000000000, -1.000000000000000000, 0.000000000000000000 ) ) ;
#19343 =( BOUNDED_CURVE ( )  B_SPLINE_CURVE ( 2, ( #498, #8896, #13726, #19380, #29826, #6330, #3754, #14228, #1159, #11640, #31898, #31735, #18720 ),
 .UNSPECIFIED., .F., .T. ) 
 B_SPLINE_CURVE_WITH_KNOTS ( ( 3, 2, 2, 2, 2, 2, 3 ),
 ( 0.08333333333333334259, 0.08888888888888889228, 0.1000000000000000056, 0.1111111111111111049, 0.1222222222222222321, 0.1333333333333333315, 0.1388888888888888951 ),
 .UNSPECIFIED. ) 
 CURVE ( )  GEOMETRIC_REPRESENTATION_ITEM ( )  RATIONAL_B_SPLINE_CURVE ( ( 0.9755282581475768211, 0.9755282581475768211, 1.000000000000000000, 0.9510565162951535312, 1.000000000000000000, 0.9510565162951535312, 1.000000000000000000, 0.9510565162951535312, 1.000000000000000000, 0.9510565162951535312, 1.000000000000000000, 0.9755282581475767101, 0.9755282581475768211 ) ) 
 REPRESENTATION_ITEM ( '' )  );
#19344 = ADVANCED_FACE ( 'NONE', ( #20921 ), #7527, .T. ) ;
#19345 = CARTESIAN_POINT ( 'NONE',  ( -10.04305231718578462, 44.90000000546237402, 30.90933677959249337 ) ) ;
#19346 = CARTESIAN_POINT ( 'NONE',  ( -10.04305231718578462, 66.40000000000000568, 30.90933677959249337 ) ) ;
#19347 = CARTESIAN_POINT ( 'NONE',  ( 6.486482029760649416E-15, 9.625000002731178839, 35.31076352940723240 ) ) ;
#19348 = CARTESIAN_POINT ( 'NONE',  ( -7.236395654485763274, 4.024999997268824181, 22.27133577429736633 ) ) ;
#19349 = CARTESIAN_POINT ( 'NONE',  ( -28.02196122052058413, 27.46315999907601935, -7.468012846824272799 ) ) ;
#19350 = CARTESIAN_POINT ( 'NONE',  ( -32.50000000000000000, 52.40000000546238823, -10.55989012756945300 ) ) ;
#19351 = CARTESIAN_POINT ( 'NONE',  ( 7.025853678916867295, 26.31732666574268364, 26.06988505166722803 ) ) ;
#19352 = CARTESIAN_POINT ( 'NONE',  ( -15.00000000000000000, 76.35000000546234844, 4.873795443493597723 ) ) ;
#19353 = CARTESIAN_POINT ( 'NONE',  ( -33.58253175000000113, 21.12500000273118062, 0.000000000000000000 ) ) ;
#19354 = CARTESIAN_POINT ( 'NONE',  ( 23.41746824999999887, 3.124999997268812280, 0.000000000000000000 ) ) ;
#19355 = CARTESIAN_POINT ( 'NONE',  ( -27.95245687107222921, 56.25781249999997868, 2.498001805406602216E-13 ) ) ;
#19356 = VERTEX_POINT ( 'NONE', #15429 ) ;
#19357 = CARTESIAN_POINT ( 'NONE',  ( -20.75514604977248112, 53.42500000273117422, 28.56700777964554661 ) ) ;
#19358 = CARTESIAN_POINT ( 'NONE',  ( 33.58253175000000823, 28.27500000273118985, 10.91162601494192863 ) ) ;
#19359 = VERTEX_POINT ( 'NONE', #7861 ) ;
#19360 = CARTESIAN_POINT ( 'NONE',  ( -28.01184896238290278, 25.17708333333332860, 7.505752307973363457 ) ) ;
#19361 = CARTESIAN_POINT ( 'NONE',  ( -30.02300923189239867, 23.32069416759064140, -0.04044903254991731589 ) ) ;
#19362 = AXIS2_PLACEMENT_3D ( 'NONE', #21799, #16320, #16156 ) ;
#19363 = CARTESIAN_POINT ( 'NONE',  ( -26.29305231718578995, 10.19999999999998685, 19.10302069950538595 ) ) ;
#19364 = CARTESIAN_POINT ( 'NONE',  ( -7.570916362186210335, 14.34999999453762065, -23.30088464923126779 ) ) ;
#19365 = AXIS2_PLACEMENT_3D ( 'NONE', #33637, #22656, #22829 ) ;
#19366 = CARTESIAN_POINT ( 'NONE',  ( 23.41746825000000243, 6.724999997268811924, -7.608796670333727974 ) ) ;
#19367 = CARTESIAN_POINT ( 'NONE',  ( -27.16883889988623935, 29.57500000273119412, 19.73931689729374739 ) ) ;
#19368 = CARTESIAN_POINT ( 'NONE',  ( 26.29305231718578995, 33.70000000546238539, -19.10302069950538240 ) ) ;
#19369 = CARTESIAN_POINT ( 'NONE',  ( 20.08610463437157279, 71.29999999999999716, -27.64615127144129758 ) ) ;
#19370 = CARTESIAN_POINT ( 'NONE',  ( -14.45873412499999944, 70.56250000409680467, 0.000000000000000000 ) ) ;
#19371 = CARTESIAN_POINT ( 'NONE',  ( 7.543491769121427382, 55.26079833425730214, -28.00173670424548433 ) ) ;
#19372 = CARTESIAN_POINT ( 'NONE',  ( -33.58253175000000113, 41.37500000273119838, 0.000000000000000000 ) ) ;
#19373 = CARTESIAN_POINT ( 'NONE',  ( 14.47279130897151589, 8.824999997268804464, 19.92008829642072953 ) ) ;
#19374 = CARTESIAN_POINT ( 'NONE',  ( -32.50000000000000000, 12.09999999999999787, 10.55989012756946366 ) ) ;
#19375 = CARTESIAN_POINT ( 'NONE',  ( 24.50000000000000355, 11.90000000000000391, 7.960532557706212486 ) ) ;
#19376 = CARTESIAN_POINT ( 'NONE',  ( 26.06988505166722803, 42.64545166574268364, -7.025853678916862854 ) ) ;
#19377 = CARTESIAN_POINT ( 'NONE',  ( -33.58253175000000113, 61.22500000273118559, 10.91162601494193929 ) ) ;
#19378 = CARTESIAN_POINT ( 'NONE',  ( -33.58253175000000113, 47.37500000273120548, 0.000000000000000000 ) ) ;
#19379 = CARTESIAN_POINT ( 'NONE',  ( -14.47279130897152299, 9.924999997268827201, 19.92008829642072243 ) ) ;
#19380 = CARTESIAN_POINT ( 'NONE',  ( 15.14183272437242067, 3.449999994537619852, 20.84094480462498211 ) ) ;
#19381 = CARTESIAN_POINT ( 'NONE',  ( 33.58253175000000113, 4.125000002731193938, -4.112674001490185761E-15 ) ) ;
#19382 = CARTESIAN_POINT ( 'NONE',  ( 13.94119854578937812, 39.36236083425731636, 24.22776226481240514 ) ) ;
#19383 = DIRECTION ( 'NONE',  ( -0.000000000000000000, -1.000000000000000000, -0.000000000000000000 ) ) ;
#19384 = CARTESIAN_POINT ( 'NONE',  ( -18.68038058909792554, 52.00000000000000000, 27.25458793344659369 ) ) ;
#19385 = CARTESIAN_POINT ( 'NONE',  ( 20.75514604977249178, 25.82500000273117280, 28.56700777964553950 ) ) ;
#19386 = CARTESIAN_POINT ( 'NONE',  ( -10.04305231718579172, 56.10000000546237686, -30.90933677959248982 ) ) ;
#19387 = CARTESIAN_POINT ( 'NONE',  ( 5.779280353836490358E-15, 21.00000000546237544, 32.49999999999999289 ) ) ;
#19388 = VECTOR ( 'NONE', #5293, 1000.000000000000000 ) ;
#19389 = CARTESIAN_POINT ( 'NONE',  ( 20.08610463437158344, 1.200000005462378283, 27.64615127144129403 ) ) ;
#19390 = CARTESIAN_POINT ( 'NONE',  ( -14.97647472619899389, 54.24701416574269075, 26.02091320914878025 ) ) ;
#19391 = CARTESIAN_POINT ( 'NONE',  ( 26.29305231718578995, 47.70000000546238539, -19.10302069950538240 ) ) ;
#19392 = CARTESIAN_POINT ( 'NONE',  ( 4.300734207923761154, 71.97500000273122112, 13.23629886949340495 ) ) ;
#19393 =( NAMED_UNIT ( * ) PLANE_ANGLE_UNIT ( ) SI_UNIT ( $, .RADIAN. ) );
#19394 = CARTESIAN_POINT ( 'NONE',  ( 19.09188309203694800, 24.03124999999999645, 19.09188309203660694 ) ) ;
#19395 = CARTESIAN_POINT ( 'NONE',  ( 20.75514604977248467, 78.42500000273116711, -28.56700777964554305 ) ) ;
#19396 = CARTESIAN_POINT ( 'NONE',  ( -20.50609665441004736, 29.18749999999999645, -20.50609665440969565 ) ) ;
#19397 = DIRECTION ( 'NONE',  ( -0.000000000000000000, -1.000000000000000000, -0.000000000000000000 ) ) ;
#19398 = ORIENTED_EDGE ( 'NONE', *, *, #3894, .F. ) ;
#19399 = CARTESIAN_POINT ( 'NONE',  ( 7.468012846824777284, 49.81809000092397355, 28.02196122052045268 ) ) ;
#19400 = CARTESIAN_POINT ( 'NONE',  ( 32.50000000000000000, 9.600000005462375086, -10.55989012756945833 ) ) ;
#19401 =( BOUNDED_CURVE ( )  B_SPLINE_CURVE ( 2, ( #2300, #7450, #33707, #33355, #15355, #15180, #12772, #2474, #28044, #20686, #15528, #10369, #25645 ),
 .UNSPECIFIED., .F., .T. ) 
 B_SPLINE_CURVE_WITH_KNOTS ( ( 3, 2, 2, 2, 2, 2, 3 ),
 ( 0.2371794871794871973, 0.2384615384615384748, 0.2410256410256410298, 0.2435897435897435848, 0.2461538461538461675, 0.2487179487179487225, 0.2500000000000000000 ),
 .UNSPECIFIED. ) 
 CURVE ( )  GEOMETRIC_REPRESENTATION_ITEM ( )  RATIONAL_B_SPLINE_CURVE ( ( 0.9755282581475768211, 0.9755282581475770431, 1.000000000000000000, 0.9510565162951535312, 1.000000000000000000, 0.9510565162951535312, 1.000000000000000000, 0.9510565162951535312, 1.000000000000000000, 0.9510565162951535312, 1.000000000000000000, 0.9755282581475768211, 0.9755282581475768211 ) ) 
 REPRESENTATION_ITEM ( '' )  );
#19402 = CARTESIAN_POINT ( 'NONE',  ( 28.01184896238304134, 58.11979166666665719, 7.505752307972846538 ) ) ;
#19403 = CARTESIAN_POINT ( 'NONE',  ( -26.29305231718579350, 46.30000000546238681, -19.10302069950537884 ) ) ;
#19404 = CARTESIAN_POINT ( 'NONE',  ( 27.16883889988624290, 48.17500000273117422, 19.73931689729373673 ) ) ;
#19405 = CARTESIAN_POINT ( 'NONE',  ( -20.08610463437157989, 50.20000000546237118, -27.64615127144129758 ) ) ;
#19406 = CARTESIAN_POINT ( 'NONE',  ( -13.91746824999999532, 73.27500000273118985, -4.522059556121115875 ) ) ;
#19407 = CARTESIAN_POINT ( 'NONE',  ( 20.75514604977249178, 33.82500000273117990, 28.56700777964553950 ) ) ;
#19408 = CLOSED_SHELL ( 'NONE', ( #2093, #3381, #21216, #8304 ) ) ;
#19409 = CARTESIAN_POINT ( 'NONE',  ( 33.58253175000000113, 64.37500000273119838, -4.112674001490185761E-15 ) ) ;
#19410 = CARTESIAN_POINT ( 'NONE',  ( -26.29305231718579350, 33.79999999999998295, -19.10302069950537884 ) ) ;
#19411 = CARTESIAN_POINT ( 'NONE',  ( 20.08610463437157279, 35.29999999999999716, -27.64615127144129758 ) ) ;
#19412 = CARTESIAN_POINT ( 'NONE',  ( -18.94512977948576093, 13.82499999726879913, 13.76444248337722698 ) ) ;
#19413 = CARTESIAN_POINT ( 'NONE',  ( -33.58253175000000113, 5.475000002731181148, 10.91162601494193929 ) ) ;
#19414 = CARTESIAN_POINT ( 'NONE',  ( 20.08610463437157279, 13.29999999999998650, -27.64615127144129758 ) ) ;
#19415 = CARTESIAN_POINT ( 'NONE',  ( -4.300734207923755825, 79.77500000273118985, 13.23629886949340673 ) ) ;
#19416 = CARTESIAN_POINT ( 'NONE',  ( -10.37757302488624411, 64.97500000273120691, -31.93888565452638417 ) ) ;
#19417 = DIRECTION ( 'NONE',  ( -1.000000000000000000, 0.000000000000000000, 0.000000000000000000 ) ) ;
#19418 = CARTESIAN_POINT ( 'NONE',  ( 33.58253175000000113, 68.37500000273121259, -4.112674001490185761E-15 ) ) ;
#19419 = EDGE_LOOP ( 'NONE', ( #12814, #1735, #22487, #31251 ) ) ;
#19420 = CARTESIAN_POINT ( 'NONE',  ( -4.732186688966233175E-15, 7.249999994537616566, 25.76082449383753925 ) ) ;
#19421 = CARTESIAN_POINT ( 'NONE',  ( -13.94119854578936923, 10.14361083425730925, -24.22776226481241224 ) ) ;
#19422 = LINE ( 'NONE', #1378, #28332 ) ;
#19423 = CARTESIAN_POINT ( 'NONE',  ( 33.58253175000000113, 48.22500000273119269, -10.91162601494193751 ) ) ;
#19424 = CARTESIAN_POINT ( 'NONE',  ( -27.16883889988624290, 9.175000002731179549, -19.73931689729374028 ) ) ;
#19425 = CARTESIAN_POINT ( 'NONE',  ( -20.75514604977248823, 61.07500000273119412, -28.56700777964554305 ) ) ;
#19426 = CARTESIAN_POINT ( 'NONE',  ( -26.07999730980477437, 49.23958333333332860, 6.988114217768305103 ) ) ;
#19427 = CARTESIAN_POINT ( 'NONE',  ( -25.98046417659859486, 37.35715250092397355, -15.04653450569291628 ) ) ;
#19428 = CARTESIAN_POINT ( 'NONE',  ( 28.02196122052058413, 29.18190999907601579, 7.468012846824272799 ) ) ;
#19429 = CARTESIAN_POINT ( 'NONE',  ( 10.04305231718578817, 67.90000000546238823, -30.90933677959249337 ) ) ;
#19430 =( GEOMETRIC_REPRESENTATION_CONTEXT ( 3 ) GLOBAL_UNCERTAINTY_ASSIGNED_CONTEXT ( ( #18885 ) ) GLOBAL_UNIT_ASSIGNED_CONTEXT ( ( #6321, #22281, #1320 ) ) REPRESENTATION_CONTEXT ( 'NONE', 'WORKASPACE' ) );
#19431 = CARTESIAN_POINT ( 'NONE',  ( -11.25946833292375793, 78.67500000273119554, -8.180482586598733619 ) ) ;
#19432 = CARTESIAN_POINT ( 'NONE',  ( -26.06988505166722803, 58.11420166574269075, 7.025853678916877953 ) ) ;
#19433 = CARTESIAN_POINT ( 'NONE',  ( -20.08610463437156923, 58.29999999999999716, 27.64615127144130113 ) ) ;
#19434 = EDGE_CURVE ( 'NONE', #24093, #14205, #28795, .T. ) ;
#19435 = CARTESIAN_POINT ( 'NONE',  ( 5.147494310547434893, 58.55125428154682510, 32.49999999999999289 ) ) ;
#19436 = EDGE_LOOP ( 'NONE', ( #3070, #29310, #19643, #597 ) ) ;
#19437 = CARTESIAN_POINT ( 'NONE',  ( 27.16883889988624290, 38.17500000273120264, 19.73931689729373673 ) ) ;
#19438 = CARTESIAN_POINT ( 'NONE',  ( 23.41746824999999887, 1.124999997268810725, 0.000000000000000000 ) ) ;
#19439 = CARTESIAN_POINT ( 'NONE',  ( 20.08610463437158344, 27.20000000546237118, 27.64615127144129403 ) ) ;
#19440 = ORIENTED_EDGE ( 'NONE', *, *, #31799, .T. ) ;
#19441 = CARTESIAN_POINT ( 'NONE',  ( 10.37757302488624056, 8.525000002731195181, -31.93888565452638417 ) ) ;
#19442 = EDGE_CURVE ( 'NONE', #3647, #22014, #23715, .T. ) ;
#19443 = ADVANCED_FACE ( 'NONE', ( #21591 ), #3230, .T. ) ;
#19444 = CARTESIAN_POINT ( 'NONE',  ( -7.505752307973343918, 36.34895833333333570, -28.01184896238290989 ) ) ;
#19445 = VERTEX_POINT ( 'NONE', #24163 ) ;
#19446 = DIRECTION ( 'NONE',  ( -1.224646799147353454E-16, 1.000000000000000000, -0.000000000000000000 ) ) ;
#19447 = CARTESIAN_POINT ( 'NONE',  ( -10.37757302488623701, 53.52500000273118985, 31.93888565452638417 ) ) ;
#19448 = CARTESIAN_POINT ( 'NONE',  ( -7.505752307973343918, 53.53645833333332860, -28.01184896238290989 ) ) ;
#19449 = CARTESIAN_POINT ( 'NONE',  ( 32.50000000000000000, 9.600000005462375086, -10.55989012756945833 ) ) ;
#19450 = DIRECTION ( 'NONE',  ( -0.8660254037844387076, 0.000000000000000000, -0.4999999999999998335 ) ) ;
#19451 = CARTESIAN_POINT ( 'NONE',  ( 18.94512977948576093, 17.32499999726880446, -13.76444248337722875 ) ) ;
#19452 = COLOUR_RGB ( '', 0.72549020, 0.75294118, 0.79215686) ;
#19453 = CARTESIAN_POINT ( 'NONE',  ( 10.04305231718579705, 56.59999999999998010, 30.90933677959248982 ) ) ;
#19454 = CARTESIAN_POINT ( 'NONE',  ( -33.58253175000000113, 21.27500000273117209, -10.91162601494193218 ) ) ;
#19455 = CARTESIAN_POINT ( 'NONE',  ( 6.950374756619257965, 14.57253499907601935, -26.09010956794244507 ) ) ;
#19456 = CARTESIAN_POINT ( 'NONE',  ( 11.25946833292375793, 73.67500000273119554, 8.180482586598731842 ) ) ;
#19457 = CARTESIAN_POINT ( 'NONE',  ( 3.880418787951172011, 15.55125428154684819, 24.49999999999998579 ) ) ;
#19458 = CARTESIAN_POINT ( 'NONE',  ( 5.779280353836490358E-15, 29.00000000546237544, 32.49999999999999289 ) ) ;
#19459 = CARTESIAN_POINT ( 'NONE',  ( 26.29305231718578995, 9.199999999999999289, -19.10302069950538240 ) ) ;
#19460 = ORIENTED_EDGE ( 'NONE', *, *, #20163, .F. ) ;
#19461 = CARTESIAN_POINT ( 'NONE',  ( 7.236395654485755280, 6.724999997268804819, 22.27133577429736988 ) ) ;
#19462 = CARTESIAN_POINT ( 'NONE',  ( -4.300734207923755825, 71.27500000273117564, 13.23629886949340673 ) ) ;
#19463 = CARTESIAN_POINT ( 'NONE',  ( -24.20753774853730889, 38.78385416666665719, 13.97622843553633842 ) ) ;
#19464 = CARTESIAN_POINT ( 'NONE',  ( 33.58253175000000113, 20.12500000273118062, -4.112674001490185761E-15 ) ) ;
#19465 = CARTESIAN_POINT ( 'NONE',  ( 27.16883889988623935, 64.32500000273121543, -19.73931689729374384 ) ) ;
#19466 = CARTESIAN_POINT ( 'NONE',  ( -33.58253175000000113, 29.37500000273117351, 0.000000000000000000 ) ) ;
#19467 = CARTESIAN_POINT ( 'NONE',  ( -33.58253175000000113, 15.27500000273118985, -10.91162601494193218 ) ) ;
#19468 = CARTESIAN_POINT ( 'NONE',  ( 33.58253175000000823, 12.27500000273116854, 10.91162601494192685 ) ) ;
#19469 = CARTESIAN_POINT ( 'NONE',  ( 26.02091320914851025, 14.44048583425730925, -14.97647472619946463 ) ) ;
#19470 = CARTESIAN_POINT ( 'NONE',  ( -7.505752307973343918, 56.97395833333333570, -28.01184896238290989 ) ) ;
#19471 = CARTESIAN_POINT ( 'NONE',  ( 13.91746824999999887, 76.37500000273116996, -1.704398294459741270E-15 ) ) ;
#19472 = CARTESIAN_POINT ( 'NONE',  ( -32.50000000000000000, 48.00000000000000000, 0.000000000000000000 ) ) ;
#19473 = DIRECTION ( 'NONE',  ( 0.000000000000000000, 1.000000000000000000, 0.000000000000000000 ) ) ;
#19474 = CARTESIAN_POINT ( 'NONE',  ( 20.75514604977249178, 49.82500000273117990, 28.56700777964553950 ) ) ;
#19475 = CARTESIAN_POINT ( 'NONE',  ( -4.523095164977116484E-15, 14.62499999726882649, 24.62258325217400312 ) ) ;
#19476 = AXIS2_PLACEMENT_3D ( 'NONE', #1822, #2000, #33576 ) ;
#19477 = ORIENTED_EDGE ( 'NONE', *, *, #22577, .F. ) ;
#19478 = CARTESIAN_POINT ( 'NONE',  ( -33.58253175000000113, 57.37500000273119838, 0.000000000000000000 ) ) ;
#19479 = DIRECTION ( 'NONE',  ( 0.000000000000000000, 0.000000000000000000, -1.000000000000000000 ) ) ;
#19480 = CARTESIAN_POINT ( 'NONE',  ( -18.94512977948575738, 5.424999997268809437, -13.76444248337723231 ) ) ;
#19481 = CARTESIAN_POINT ( 'NONE',  ( -19.11951029504763611, 22.89100666759064495, 19.06425588902592239 ) ) ;
#19482 = ORIENTED_EDGE ( 'NONE', *, *, #14265, .F. ) ;
#19483 = CARTESIAN_POINT ( 'NONE',  ( 20.75514604977248467, 36.42500000273118843, -28.56700777964554305 ) ) ;
#19484 = CARTESIAN_POINT ( 'NONE',  ( 19.82091636218621389, 6.200000000000010836, -14.40073868116559197 ) ) ;
#19485 = ORIENTED_EDGE ( 'NONE', *, *, #17210, .T. ) ;
#19486 = CARTESIAN_POINT ( 'NONE',  ( -28.01184896238290278, 56.11458333333332860, 7.505752307973363457 ) ) ;
#19487 = CARTESIAN_POINT ( 'NONE',  ( 33.58253175000000823, 60.27500000273116143, 10.91162601494192863 ) ) ;
#19488 = CARTESIAN_POINT ( 'NONE',  ( 9.270509831248421762, 75.55000000546240813, -12.75976212528059861 ) ) ;
#19489 = CARTESIAN_POINT ( 'NONE',  ( -27.16883889988623935, 73.32500000273117280, 19.73931689729374739 ) ) ;
#19490 = CARTESIAN_POINT ( 'NONE',  ( 7.505752307972854531, 29.76041666666666430, -28.01184896238303423 ) ) ;
#19491 = CARTESIAN_POINT ( 'NONE',  ( 19.82091636218621389, 6.200000000000010836, -14.40073868116559197 ) ) ;
#19492 = CARTESIAN_POINT ( 'NONE',  ( 33.58253175000000113, 2.375000002731192161, -4.112674001490185761E-15 ) ) ;
#19493 = ADVANCED_FACE ( 'NONE', ( #19514 ), #11285, .F. ) ;
#19494 = CARTESIAN_POINT ( 'NONE',  ( -10.37757302488623701, 19.52500000273118985, 31.93888565452638417 ) ) ;
#19495 = FILL_AREA_STYLE_COLOUR ( '', #31872 ) ;
#19496 = CARTESIAN_POINT ( 'NONE',  ( -25.98046417659831420, 40.78347249907601935, 15.04653450569339945 ) ) ;
#19497 = CARTESIAN_POINT ( 'NONE',  ( 4.635254915624209993, 79.39999999999999147, -14.26584774442730463 ) ) ;
#19498 = CARTESIAN_POINT ( 'NONE',  ( 30.02300923189239867, 57.97656249999998579, -2.619432448724978208E-13 ) ) ;
#19499 = DIRECTION ( 'NONE',  ( -0.000000000000000000, -1.000000000000000000, -0.000000000000000000 ) ) ;
#19500 = CARTESIAN_POINT ( 'NONE',  ( 24.50000000000000355, 5.649999994537638237, 7.960532557706212486 ) ) ;
#19501 = CARTESIAN_POINT ( 'NONE',  ( 5.147494310547434893, 49.05125428700922185, 32.49999999999999289 ) ) ;
#19502 = CARTESIAN_POINT ( 'NONE',  ( 6.988114217768294445, 14.00520833333333215, 26.07999730980477437 ) ) ;
#19503 =( BOUNDED_CURVE ( )  B_SPLINE_CURVE ( 2, ( #11562, #24608, #23187, #33649, #10146, #16894, #27357 ),
 .UNSPECIFIED., .F., .T. ) 
 B_SPLINE_CURVE_WITH_KNOTS ( ( 3, 2, 2, 3 ),
 ( 0.000000000000000000, 0.02000000000000000042, 0.04000000000000000083, 0.05000000000000000971 ),
 .UNSPECIFIED. ) 
 CURVE ( )  GEOMETRIC_REPRESENTATION_ITEM ( )  RATIONAL_B_SPLINE_CURVE ( ( 1.000000000000000000, 0.9510565162951535312, 1.000000000000000000, 0.9510565162951535312, 1.000000000000000000, 0.9755282581475768211, 0.9755282581475768211 ) ) 
 REPRESENTATION_ITEM ( '' )  );
#19504 = CARTESIAN_POINT ( 'NONE',  ( -20.75514604977248112, 39.42500000273118843, 28.56700777964554661 ) ) ;
#19505 = CARTESIAN_POINT ( 'NONE',  ( 13.91746824999999887, 77.87500000273116996, -1.704398294459741270E-15 ) ) ;
#19506 = CARTESIAN_POINT ( 'NONE',  ( 20.75514604977249178, 52.07500000273119412, 28.56700777964553950 ) ) ;
#19507 = CARTESIAN_POINT ( 'NONE',  ( -10.37757302488624411, 28.97500000273117848, -31.93888565452638417 ) ) ;
#19508 = CARTESIAN_POINT ( 'NONE',  ( 2.535219702907248518, 16.99999999999999289, 23.89400104877895714 ) ) ;
#19509 = CARTESIAN_POINT ( 'NONE',  ( -26.07999730980477437, 32.05208333333332860, 6.988114217768305103 ) ) ;
#19510 = CARTESIAN_POINT ( 'NONE',  ( 2.375766604868043697, 80.55125428154684641, 15.00000000000000178 ) ) ;
#19511 = CARTESIAN_POINT ( 'NONE',  ( 32.50000000000000000, 67.10000000000000853, -10.55989012756945833 ) ) ;
#19512 = CARTESIAN_POINT ( 'NONE',  ( 14.47279130897151767, 12.32499999726880802, 19.92008829642072953 ) ) ;
#19513 = CARTESIAN_POINT ( 'NONE',  ( 20.53372385742108008, 29.46836833240935505, 20.47846945139866648 ) ) ;
#19514 = FACE_OUTER_BOUND ( 'NONE', #8915, .T. ) ;
#19515 = CARTESIAN_POINT ( 'NONE',  ( 6.950374756619257965, 31.76003499907602290, -26.09010956794244507 ) ) ;
#19516 = CARTESIAN_POINT ( 'NONE',  ( -32.50000000000000000, 65.99999999999998579, 0.000000000000000000 ) ) ;
#19517 = CARTESIAN_POINT ( 'NONE',  ( 27.16883889988624290, 15.92500000273117067, 19.73931689729373673 ) ) ;
#19518 = CARTESIAN_POINT ( 'NONE',  ( 18.94512977948575738, 4.924999997268808549, 13.76444248337723408 ) ) ;
#19519 = CARTESIAN_POINT ( 'NONE',  ( 27.95245687107222921, 54.53906249999998579, -2.463307335887066074E-13 ) ) ;
#19520 = ORIENTED_EDGE ( 'NONE', *, *, #30596, .F. ) ;
#19521 = CARTESIAN_POINT ( 'NONE',  ( 20.75514604977248467, 56.42500000273120264, -28.56700777964554305 ) ) ;
#19522 = CARTESIAN_POINT ( 'NONE',  ( 27.16883889988624290, 26.17500000273119554, 19.73931689729373673 ) ) ;
#19523 = ORIENTED_EDGE ( 'NONE', *, *, #1457, .F. ) ;
#19524 = CARTESIAN_POINT ( 'NONE',  ( 20.50609665441005092, 24.03124999999999645, 20.50609665440969209 ) ) ;
#19525 = CARTESIAN_POINT ( 'NONE',  ( -14.97647472619946285, 23.89361083425731280, -26.02091320914851025 ) ) ;
#19526 = CARTESIAN_POINT ( 'NONE',  ( 3.880418787951134707, 15.30125427608446742, 24.50000000000000000 ) ) ;
#19527 = CARTESIAN_POINT ( 'NONE',  ( 1.577395562988744260E-15, 18.24999999453762101, -25.76082449383753925 ) ) ;
#19528 = CARTESIAN_POINT ( 'NONE',  ( 23.41746825000000243, 2.524999997268798868, 7.608796670333735079 ) ) ;
#19529 = CARTESIAN_POINT ( 'NONE',  ( -20.75514604977248112, 19.67500000273119909, 28.56700777964554661 ) ) ;
#19530 = CARTESIAN_POINT ( 'NONE',  ( -20.08610463437157989, 32.20000000546238539, -27.64615127144129758 ) ) ;
#19531 = EDGE_CURVE ( 'NONE', #29552, #8544, #21428, .T. ) ;
#19532 = CARTESIAN_POINT ( 'NONE',  ( -10.04305231718578462, 74.40000000000001990, 30.90933677959249337 ) ) ;
#19533 = CARTESIAN_POINT ( 'NONE',  ( 0.000000000000000000, -23.00000000000000000, 0.000000000000000000 ) ) ;
#19534 = CARTESIAN_POINT ( 'NONE',  ( 26.29305231718579350, 37.30000000546237970, 19.10302069950537529 ) ) ;
#19535 = CARTESIAN_POINT ( 'NONE',  ( 20.53372385742072481, 55.54725666759064495, -20.47846945139902175 ) ) ;
#19536 = CARTESIAN_POINT ( 'NONE',  ( -33.58253175000000113, 35.27500000273120406, -10.91162601494193218 ) ) ;
#19537 = CARTESIAN_POINT ( 'NONE',  ( 27.16883889988624290, 55.92500000273119554, 19.73931689729373673 ) ) ;
#19538 = CARTESIAN_POINT ( 'NONE',  ( -7.505752307972844761, 34.91666666666666430, 28.01184896238304134 ) ) ;
#19539 = ADVANCED_FACE ( 'NONE', ( #3725 ), #19183, .T. ) ;
#19540 = CARTESIAN_POINT ( 'NONE',  ( 23.41746825000000243, 9.024999997268826846, 7.608796670333735079 ) ) ;
#19541 = CARTESIAN_POINT ( 'NONE',  ( -20.08610463437157989, 11.70000000000000995, -27.64615127144129758 ) ) ;
#19542 = CARTESIAN_POINT ( 'NONE',  ( -24.50000000000001066, 11.09999999999999964, 7.960532557706201828 ) ) ;
#19543 = CARTESIAN_POINT ( 'NONE',  ( 0.04044903255044120238, 47.08555583240935505, 27.95245687107223276 ) ) ;
#19544 = CARTESIAN_POINT ( 'NONE',  ( 6.486482029760649416E-15, 55.62500000273119838, 35.31076352940723240 ) ) ;
#19545 = CARTESIAN_POINT ( 'NONE',  ( -2.162160676586882350E-15, 44.87500000273119127, -35.31076352940722529 ) ) ;
#19546 = CARTESIAN_POINT ( 'NONE',  ( 23.41746824999999887, 8.524999997268812635, 7.608796670333735079 ) ) ;
#19547 = CARTESIAN_POINT ( 'NONE',  ( 32.50000000000000000, 67.50000000546238255, -3.980102097228898626E-15 ) ) ;
#19548 = CARTESIAN_POINT ( 'NONE',  ( -20.75514604977248112, 7.425000002731177773, 28.56700777964554661 ) ) ;
#19549 = CARTESIAN_POINT ( 'NONE',  ( -24.18731323226248264, 37.35715250092397355, -14.01125832528284931 ) ) ;
#19550 = CARTESIAN_POINT ( 'NONE',  ( 14.28720042100528609, 16.99999999999998579, -18.56979130494320529 ) ) ;
#19551 = DIRECTION ( 'NONE',  ( 0.000000000000000000, 0.000000000000000000, -1.000000000000000000 ) ) ;
#19552 = PRODUCT_DEFINITION_CONTEXT ( 'detailed design', #4386, 'design' ) ;
#19553 = CARTESIAN_POINT ( 'NONE',  ( 20.75514604977248467, 26.42500000273118843, -28.56700777964554305 ) ) ;
#19554 = CARTESIAN_POINT ( 'NONE',  ( 1.555960095263670572E-15, 14.50000000000000178, -24.50000000000000000 ) ) ;
#19555 = CARTESIAN_POINT ( 'NONE',  ( 5.779280353836490358E-15, 48.50000000000000000, 32.49999999999999289 ) ) ;
#19556 = CARTESIAN_POINT ( 'NONE',  ( 15.14183272437242422, 14.29999999999998472, -20.84094480462497856 ) ) ;
#19557 = CARTESIAN_POINT ( 'NONE',  ( -15.04653450569338524, 51.95534749907602645, -25.98046417659831775 ) ) ;
#19558 = CARTESIAN_POINT ( 'NONE',  ( 6.277390505771533514E-15, 51.00000000546238255, 34.17252228774368916 ) ) ;
#19559 = CARTESIAN_POINT ( 'NONE',  ( 5.779280353836490358E-15, 59.00000000546238255, 32.49999999999999289 ) ) ;
#19560 = CARTESIAN_POINT ( 'NONE',  ( -33.58253175000000113, 33.12500000273119127, 0.000000000000000000 ) ) ;
#19561 = CARTESIAN_POINT ( 'NONE',  ( 19.09188309203694800, 27.46875000000000000, 19.09188309203660694 ) ) ;
#19562 = CARTESIAN_POINT ( 'NONE',  ( -10.37757302488623701, 75.52500000273120406, 31.93888565452638417 ) ) ;
#19563 = VECTOR ( 'NONE', #26383, 1000.000000000000000 ) ;
#19564 = CARTESIAN_POINT ( 'NONE',  ( 26.00068869287367335, 27.32552083333332860, 15.01150461594596308 ) ) ;
#19565 = DIRECTION ( 'NONE',  ( -1.224646799147353454E-16, 1.000000000000000000, -0.000000000000000000 ) ) ;
#19566 = EDGE_LOOP ( 'NONE', ( #32632, #1032, #1996, #10291 ) ) ;
#19567 = CARTESIAN_POINT ( 'NONE',  ( -7.543491769121417612, 46.66704833425730925, 28.00173670424549499 ) ) ;
#19568 = CARTESIAN_POINT ( 'NONE',  ( -32.50000000000000000, 12.40000000546237224, -10.55989012756945478 ) ) ;
#19569 = VECTOR ( 'NONE', #10031, 1000.000000000000000 ) ;
#19570 = CARTESIAN_POINT ( 'NONE',  ( 26.00068869287340334, 61.12760416666665719, -15.01150461594642316 ) ) ;
#19571 = CARTESIAN_POINT ( 'NONE',  ( 26.29305231718579350, 56.80000000000001847, 19.10302069950537529 ) ) ;
#19572 = CARTESIAN_POINT ( 'NONE',  ( 27.16883889988623935, 42.57500000273117990, -19.73931689729374384 ) ) ;
#19573 = CARTESIAN_POINT ( 'NONE',  ( -32.50000000000000000, 48.40000000546237402, -10.55989012756945478 ) ) ;
#19574 = CARTESIAN_POINT ( 'NONE',  ( -11.25946833292375793, 71.57500000273120122, 8.180482586598737171 ) ) ;
#19575 = CARTESIAN_POINT ( 'NONE',  ( 33.58253175000000113, 30.22500000273118559, -10.91162601494193751 ) ) ;
#19576 = CARTESIAN_POINT ( 'NONE',  ( 7.570916362186213000, 12.39999999999999503, -23.30088464923126423 ) ) ;
#19577 = CARTESIAN_POINT ( 'NONE',  ( -33.58253175000000113, 55.27500000273120406, -10.91162601494193218 ) ) ;
#19578 = CARTESIAN_POINT ( 'NONE',  ( 10.04305231718578817, 37.40000000000000568, -30.90933677959249337 ) ) ;
#19579 = CARTESIAN_POINT ( 'NONE',  ( -10.04305231718578462, 32.39999999999998437, 30.90933677959249337 ) ) ;
#19580 = CARTESIAN_POINT ( 'NONE',  ( -23.41746824999999887, 11.62499999726881938, -2.867812753649727150E-15 ) ) ;
#19581 = CARTESIAN_POINT ( 'NONE',  ( 20.75514604977249178, 2.075000002731171467, 28.56700777964553950 ) ) ;
#19582 = CARTESIAN_POINT ( 'NONE',  ( 5.779280353836490358E-15, 12.49999999999999112, 32.49999999999999289 ) ) ;
#19583 = CARTESIAN_POINT ( 'NONE',  ( 4.300734207923761154, 77.97500000273122112, 13.23629886949340495 ) ) ;
#19584 = CARTESIAN_POINT ( 'NONE',  ( -27.16883889988623935, 67.57500000273120122, 19.73931689729374739 ) ) ;
#19585 = CARTESIAN_POINT ( 'NONE',  ( 15.14183272437242067, 3.449999994537619852, 20.84094480462498211 ) ) ;
#19586 = ORIENTED_EDGE ( 'NONE', *, *, #5804, .F. ) ;
#19587 = CARTESIAN_POINT ( 'NONE',  ( 7.570916362186213000, 4.149999994537633796, -23.30088464923126423 ) ) ;
#19588 = CARTESIAN_POINT ( 'NONE',  ( 19.11951029504763611, 10.85975666759064318, -19.06425588902591173 ) ) ;
#19589 = DIRECTION ( 'NONE',  ( 0.000000000000000000, 0.000000000000000000, -1.000000000000000000 ) ) ;
#19590 = CARTESIAN_POINT ( 'NONE',  ( -10.37757302488623701, 49.52500000273117564, 31.93888565452638417 ) ) ;
#19591 = CARTESIAN_POINT ( 'NONE',  ( 27.16883889988623935, 4.575000002731186122, -19.73931689729374384 ) ) ;
#19592 = CARTESIAN_POINT ( 'NONE',  ( -33.58253175000000113, 61.47500000273118559, 10.91162601494193929 ) ) ;
#19593 = CARTESIAN_POINT ( 'NONE',  ( -27.95245687107223276, 49.38281249999999289, 2.498001805406602216E-13 ) ) ;
#19594 = CARTESIAN_POINT ( 'NONE',  ( 7.468012846824777284, 39.50559000092398065, 28.02196122052045268 ) ) ;
#19595 = CARTESIAN_POINT ( 'NONE',  ( -7.543491769121917656, 31.47357666574268364, -28.00173670424536354 ) ) ;
#19596 = CARTESIAN_POINT ( 'NONE',  ( -10.04305231718578462, 64.90000000546237402, 30.90933677959249337 ) ) ;
#19597 = EDGE_CURVE ( 'NONE', #1732, #31503, #32016, .T. ) ;
#19598 = FACE_OUTER_BOUND ( 'NONE', #28050, .T. ) ;
#19599 = CARTESIAN_POINT ( 'NONE',  ( 19.06425588902558133, 56.10899333240935505, -19.11951029504797006 ) ) ;
#19600 = CARTESIAN_POINT ( 'NONE',  ( -5.147494310547423346, 54.44874571845314648, 32.50000000000000000 ) ) ;
#19601 = CARTESIAN_POINT ( 'NONE',  ( -24.50000000000000000, 16.89999999999998792, -7.960532557706207157 ) ) ;
#19602 = ORIENTED_EDGE ( 'NONE', *, *, #22567, .T. ) ;
#19603 = CARTESIAN_POINT ( 'NONE',  ( -10.37757302488624411, 38.97500000273117138, -31.93888565452638417 ) ) ;
#19604 = CARTESIAN_POINT ( 'NONE',  ( -18.94512977948576093, 2.324999997268817342, 13.76444248337722698 ) ) ;
#19605 = CARTESIAN_POINT ( 'NONE',  ( 32.50000000000000711, 29.40000000546239178, 10.55989012756945122 ) ) ;
#19606 = EDGE_LOOP ( 'NONE', ( #22812, #26325 ) ) ;
#19607 = CARTESIAN_POINT ( 'NONE',  ( -15.01150461594595775, 38.49739583333332860, 26.00068869287368756 ) ) ;
#19608 = VERTEX_POINT ( 'NONE', #11123 ) ;
#19609 = VERTEX_POINT ( 'NONE', #19022 ) ;
#19610 = CARTESIAN_POINT ( 'NONE',  ( 26.29305231718579350, 26.79999999999999005, 19.10302069950537529 ) ) ;
#19611 = CARTESIAN_POINT ( 'NONE',  ( -20.75514604977248823, 46.82500000273117990, -28.56700777964554305 ) ) ;
#19612 = CARTESIAN_POINT ( 'NONE',  ( -26.00068869287340334, 59.40885416666666430, 15.01150461594643382 ) ) ;
#19613 = CARTESIAN_POINT ( 'NONE',  ( -20.08610463437157989, 14.20000000546237295, -27.64615127144129758 ) ) ;
#19614 = CARTESIAN_POINT ( 'NONE',  ( 27.16883889988623935, 66.32500000273118701, -19.73931689729374384 ) ) ;
#19615 = CARTESIAN_POINT ( 'NONE',  ( -23.41746824999999887, 14.02499999726881263, -7.608796670333730638 ) ) ;
#19616 = AXIS2_PLACEMENT_3D ( 'NONE', #28071, #9533, #22252 ) ;
#19617 = CARTESIAN_POINT ( 'NONE',  ( -10.04305231718579172, 53.60000000000000853, -30.90933677959248982 ) ) ;
#19618 = CARTESIAN_POINT ( 'NONE',  ( -33.58253175000000113, 23.37500000273118417, 0.000000000000000000 ) ) ;
#19619 = CARTESIAN_POINT ( 'NONE',  ( -7.025853678916861966, 14.28607666574268720, -26.06988505166722803 ) ) ;
#19620 = CARTESIAN_POINT ( 'NONE',  ( -8.960552108402742093E-16, 74.37500000273118417, -14.63369212191046387 ) ) ;
#19621 = DIRECTION ( 'NONE',  ( 0.000000000000000000, 1.000000000000000000, 0.000000000000000000 ) ) ;
#19622 = CARTESIAN_POINT ( 'NONE',  ( -32.50000000000000000, 28.60000000546238397, 10.55989012756946366 ) ) ;
#19623 = EDGE_CURVE ( 'NONE', #28042, #601, #5965, .T. ) ;
#19624 = CARTESIAN_POINT ( 'NONE',  ( -10.04305231718578462, 6.400000000000003020, 30.90933677959249337 ) ) ;
#19625 = ORIENTED_EDGE ( 'NONE', *, *, #22429, .T. ) ;
#19626 = CARTESIAN_POINT ( 'NONE',  ( -23.41746824999999887, 10.12499999726881938, -2.867812753649727150E-15 ) ) ;
#19627 = CARTESIAN_POINT ( 'NONE',  ( -11.25946833292375793, 71.07500000273120122, 8.180482586598737171 ) ) ;
#19628 = CARTESIAN_POINT ( 'NONE',  ( -6.988114217767819270, 41.79166666666666430, 26.07999730980490583 ) ) ;
#19629 = CARTESIAN_POINT ( 'NONE',  ( -33.58253175000000113, 67.02500000273117564, -10.91162601494193218 ) ) ;
#19630 = CARTESIAN_POINT ( 'NONE',  ( 33.58253175000000113, 30.47500000273117493, -10.91162601494193751 ) ) ;
#19631 = CARTESIAN_POINT ( 'NONE',  ( -20.75514604977248112, 13.67500000273118133, 28.56700777964554661 ) ) ;
#19632 = CARTESIAN_POINT ( 'NONE',  ( -2.162160676586882350E-15, 10.87500000273118417, -35.31076352940722529 ) ) ;
#19633 = CARTESIAN_POINT ( 'NONE',  ( -20.47846945139902175, 10.00038166759064140, -20.53372385742072481 ) ) ;
#19634 = ADVANCED_FACE ( 'NONE', ( #16443 ), #26895, .T. ) ;
#19635 = CARTESIAN_POINT ( 'NONE',  ( -28.01184896238290278, 52.67708333333333570, 7.505752307973363457 ) ) ;
#19636 = CARTESIAN_POINT ( 'NONE',  ( 7.570916362186213000, 16.39999999999999858, -23.30088464923126423 ) ) ;
#19637 = CARTESIAN_POINT ( 'NONE',  ( 13.91746825000000065, 78.27500000273117564, 4.522059556121115875 ) ) ;
#19638 = CARTESIAN_POINT ( 'NONE',  ( 20.08610463437158344, 46.70000000000000284, 27.64615127144129403 ) ) ;
#19639 = SURFACE_STYLE_USAGE ( .BOTH. , #9156 ) ;
#19640 = CARTESIAN_POINT ( 'NONE',  ( 27.16883889988623935, 54.32500000273118701, -19.73931689729374384 ) ) ;
#19641 = CARTESIAN_POINT ( 'NONE',  ( -23.41746824999999887, 3.624999997268813168, -2.867812753649727150E-15 ) ) ;
#19642 = EDGE_CURVE ( 'NONE', #7457, #20157, #3554, .T. ) ;
#19643 = ORIENTED_EDGE ( 'NONE', *, *, #21344, .F. ) ;
#19644 = CARTESIAN_POINT ( 'NONE',  ( 27.16883889988624290, 62.17500000273119554, 19.73931689729373673 ) ) ;
#19645 = CARTESIAN_POINT ( 'NONE',  ( -1.778240108872766143E-15, 43.50000000000000000, -32.49999999999999289 ) ) ;
#19646 = CARTESIAN_POINT ( 'NONE',  ( 14.47279130897151589, 10.32499999726881335, 19.92008829642072953 ) ) ;
#19647 = CARTESIAN_POINT ( 'NONE',  ( -13.94119854578936923, 30.76861083425731280, -24.22776226481241224 ) ) ;
#19648 = VERTEX_POINT ( 'NONE', #14195 ) ;
#19649 = CARTESIAN_POINT ( 'NONE',  ( 33.58253175000000113, 28.22500000273119269, -10.91162601494193751 ) ) ;
#19650 = CARTESIAN_POINT ( 'NONE',  ( 15.14183272437242422, 6.300000000000004263, -20.84094480462497856 ) ) ;
#19651 = ORIENTED_EDGE ( 'NONE', *, *, #16090, .T. ) ;
#19652 = CARTESIAN_POINT ( 'NONE',  ( -28.01184896238304134, 56.40104166666666430, -7.505752307972844761 ) ) ;
#19653 = CARTESIAN_POINT ( 'NONE',  ( -10.37757302488623701, 57.77500000273119696, 31.93888565452638417 ) ) ;
#19654 = CARTESIAN_POINT ( 'NONE',  ( 32.50000000000000711, 69.40000000546237402, 10.55989012756945122 ) ) ;
#19655 = CARTESIAN_POINT ( 'NONE',  ( -27.16883889988624290, 76.92500000273119554, -19.73931689729374028 ) ) ;
#19656 = CARTESIAN_POINT ( 'NONE',  ( 28.01184896238290278, 33.77083333333333570, -7.505752307973347470 ) ) ;
#19657 = CARTESIAN_POINT ( 'NONE',  ( -24.50000000000000000, 3.000000000000002665, -3.000384657911015469E-15 ) ) ;
#19658 = CYLINDRICAL_SURFACE ( 'NONE', #13877, 32.50000000000000000 ) ;
#19659 = CARTESIAN_POINT ( 'NONE',  ( 27.16883889988624290, 15.92500000273117067, 19.73931689729373673 ) ) ;
#19660 = CARTESIAN_POINT ( 'NONE',  ( -4.300734207923759378, 74.47500000273119269, -13.23629886949340495 ) ) ;
#19661 = CARTESIAN_POINT ( 'NONE',  ( -0.04044903255044120238, 45.36680583240934794, -30.02300923189239867 ) ) ;
#19662 = CARTESIAN_POINT ( 'NONE',  ( -4.300734207923755825, 71.77500000273117564, 13.23629886949340673 ) ) ;
#19663 = CARTESIAN_POINT ( 'NONE',  ( 15.01150461594596486, 60.84114583333332860, -26.00068869287367690 ) ) ;
#19664 = CARTESIAN_POINT ( 'NONE',  ( 3.445340210940985210E-14, 9.249999994537636994, 24.50000000000000000 ) ) ;
#19665 = CARTESIAN_POINT ( 'NONE',  ( -24.50000000000001066, 4.849999994537633974, 7.960532557706201828 ) ) ;
#19666 = CARTESIAN_POINT ( 'NONE',  ( 9.270509831248423538, 75.55000000546239391, -12.75976212528059861 ) ) ;
#19667 = CARTESIAN_POINT ( 'NONE',  ( 13.97622843553633665, 13.86197916666666430, 24.20753774853730889 ) ) ;
#19668 = CARTESIAN_POINT ( 'NONE',  ( 6.486482029760649416E-15, 35.62500000273119127, 35.31076352940723240 ) ) ;
#19669 = CARTESIAN_POINT ( 'NONE',  ( -8.960552108402742093E-16, 72.37500000273115575, -14.63369212191046387 ) ) ;
#19670 = CARTESIAN_POINT ( 'NONE',  ( 6.486482029760649416E-15, 49.87500000273119838, 35.31076352940723240 ) ) ;
#19671 = CARTESIAN_POINT ( 'NONE',  ( 20.75514604977249178, 28.07500000273119412, 28.56700777964553950 ) ) ;
#19672 = CARTESIAN_POINT ( 'NONE',  ( 19.94128806827436406, 16.99999999999997868, 12.49245821715489946 ) ) ;
#19673 = CARTESIAN_POINT ( 'NONE',  ( -19.09188309203694445, 36.06250000000000000, -19.09188309203661049 ) ) ;
#19674 = CARTESIAN_POINT ( 'NONE',  ( -10.04305231718579172, 17.60000000000000497, -30.90933677959248982 ) ) ;
#19675 = LINE ( 'NONE', #22411, #4144 ) ;
#19676 = CARTESIAN_POINT ( 'NONE',  ( -20.08610463437157989, 63.69999999999998863, -27.64615127144129758 ) ) ;
#19677 = CARTESIAN_POINT ( 'NONE',  ( 18.94512977948575738, 12.42499999726881477, 13.76444248337723408 ) ) ;
#19678 = CARTESIAN_POINT ( 'NONE',  ( -20.53372385742107653, 24.31211833240934794, -20.47846945139867003 ) ) ;
#19679 = CARTESIAN_POINT ( 'NONE',  ( -18.94512977948575738, 1.924999997268805885, -13.76444248337723231 ) ) ;
#19680 = CARTESIAN_POINT ( 'NONE',  ( 7.025853678916867295, 33.19232666574268364, 26.06988505166722803 ) ) ;
#19681 = CARTESIAN_POINT ( 'NONE',  ( 27.16883889988623935, 78.57500000273120122, -19.73931689729374384 ) ) ;
#19682 = CARTESIAN_POINT ( 'NONE',  ( 33.58253175000000113, 14.12500000273120193, -4.112674001490185761E-15 ) ) ;
#19683 = CARTESIAN_POINT ( 'NONE',  ( 23.41746825000000243, 5.224999997268802154, -7.608796670333727974 ) ) ;
#19684 = CARTESIAN_POINT ( 'NONE',  ( -13.94119854578936923, 10.14361083425730925, -24.22776226481241224 ) ) ;
#19685 = ORIENTED_EDGE ( 'NONE', *, *, #23429, .F. ) ;
#19686 = CARTESIAN_POINT ( 'NONE',  ( -20.75514604977248112, 47.42500000273118843, 28.56700777964554661 ) ) ;
#19687 = CARTESIAN_POINT ( 'NONE',  ( -33.58253175000000113, 21.37500000273119483, 0.000000000000000000 ) ) ;
#19688 = VERTEX_POINT ( 'NONE', #32535 ) ;
#19689 = CARTESIAN_POINT ( 'NONE',  ( 20.50609665441005092, 20.59374999999999645, 20.50609665440969209 ) ) ;
#19690 = CARTESIAN_POINT ( 'NONE',  ( 15.04653450569292872, 27.90402750092397355, -25.98046417659857710 ) ) ;
#19691 = DIRECTION ( 'NONE',  ( 0.000000000000000000, 1.000000000000000000, 0.000000000000000000 ) ) ;
#19692 = CARTESIAN_POINT ( 'NONE',  ( 7.570916362186207671, 15.34999999453762243, 23.30088464923126779 ) ) ;
#19693 = CARTESIAN_POINT ( 'NONE',  ( -4.523095164977116484E-15, 6.124999997268802510, 24.62258325217400312 ) ) ;
#19694 = CARTESIAN_POINT ( 'NONE',  ( -33.58253175000000113, 21.47500000273119980, 10.91162601494193929 ) ) ;
#19695 = CARTESIAN_POINT ( 'NONE',  ( 6.277390505771533514E-15, 25.00000000546238255, 34.17252228774368916 ) ) ;
#19696 = SHAPE_REPRESENTATION ( 'bellows suction cup', ( #1376 ), #231 ) ;
#19697 = CARTESIAN_POINT ( 'NONE',  ( -20.08610463437156923, 74.30000000000001137, 27.64615127144130113 ) ) ;
#19698 = CARTESIAN_POINT ( 'NONE',  ( 3.980102097228898626E-15, 80.00000000000001421, 32.50000000000000000 ) ) ;
#19699 = LINE ( 'NONE', #9381, #30171 ) ;
#19700 = CARTESIAN_POINT ( 'NONE',  ( -7.543491769121417612, 53.54204833425730925, 28.00173670424549499 ) ) ;
#19701 = CARTESIAN_POINT ( 'NONE',  ( 33.58253175000000823, 36.27500000273119696, 10.91162601494192863 ) ) ;
#19702 = CARTESIAN_POINT ( 'NONE',  ( 6.486482029760648627E-15, 55.62500000273119838, 35.31076352940722529 ) ) ;
#19703 = CARTESIAN_POINT ( 'NONE',  ( -7.505752307973343918, 29.47395833333332860, -28.01184896238290989 ) ) ;
#19704 = CARTESIAN_POINT ( 'NONE',  ( 7.236395654485755280, 12.72499999726881015, 22.27133577429736988 ) ) ;
#19705 = CARTESIAN_POINT ( 'NONE',  ( -32.50000000000000000, 17.89999999999998437, -10.55989012756945478 ) ) ;
#19706 = CARTESIAN_POINT ( 'NONE',  ( -1.778240108872766143E-15, 51.50000000000000711, -32.49999999999999289 ) ) ;
#19707 = CARTESIAN_POINT ( 'NONE',  ( 24.22776226481265383, 39.63763916574268364, 13.94119854578893580 ) ) ;
#19708 = CARTESIAN_POINT ( 'NONE',  ( -10.37757302488624411, 56.72500000273117138, -31.93888565452638417 ) ) ;
#19709 = CARTESIAN_POINT ( 'NONE',  ( 20.75514604977249178, 50.07500000273120122, 28.56700777964553950 ) ) ;
#19710 = CARTESIAN_POINT ( 'NONE',  ( 7.236395654485760609, 13.02499999726880375, -22.27133577429736633 ) ) ;
#19711 = DIRECTION ( 'NONE',  ( 0.000000000000000000, 0.000000000000000000, 1.000000000000000000 ) ) ;
#19712 = CARTESIAN_POINT ( 'NONE',  ( -10.04305231718579172, 5.599999999999994316, -30.90933677959248982 ) ) ;
#19713 = CARTESIAN_POINT ( 'NONE',  ( 24.22776226481241224, 52.25298583425730925, -13.94119854578936923 ) ) ;
#19714 = CARTESIAN_POINT ( 'NONE',  ( -11.85439961466680359, 16.99999999999997868, -20.79774841451609291 ) ) ;
#19715 = CARTESIAN_POINT ( 'NONE',  ( -7.347880794884122694E-16, -16.99999999999999645, 0.000000000000000000 ) ) ;
#19716 = CARTESIAN_POINT ( 'NONE',  ( -20.75514604977248823, 18.82500000273119767, -28.56700777964554305 ) ) ;
#19717 = LINE ( 'NONE', #30164, #32996 ) ;
#19718 = CARTESIAN_POINT ( 'NONE',  ( 5.147494310547535257, 55.94874572391554324, -32.49999999999996447 ) ) ;
#19719 = CARTESIAN_POINT ( 'NONE',  ( 20.08610463437157279, 41.80000000546237260, -27.64615127144129758 ) ) ;
#19720 = CARTESIAN_POINT ( 'NONE',  ( 20.47846945139867003, 66.42149333240935505, -20.53372385742107653 ) ) ;
#19721 = CARTESIAN_POINT ( 'NONE',  ( 26.29305231718579350, 45.30000000546237260, 19.10302069950537529 ) ) ;
#19722 = EDGE_CURVE ( 'NONE', #6266, #33508, #30709, .T. ) ;
#19723 = CARTESIAN_POINT ( 'NONE',  ( 32.50000000000000000, 35.00000000000000000, -3.980102097228898626E-15 ) ) ;
#19724 = CARTESIAN_POINT ( 'NONE',  ( -33.58253175000000113, 35.22500000273120691, 10.91162601494193929 ) ) ;
#19725 = CARTESIAN_POINT ( 'NONE',  ( -24.20753774853756823, 25.60677083333332149, -13.97622843553588723 ) ) ;
#19726 = EDGE_CURVE ( 'NONE', #28806, #9414, #8568, .T. ) ;
#19727 = ORIENTED_EDGE ( 'NONE', *, *, #21954, .F. ) ;
#19728 =( REPRESENTATION_RELATIONSHIP ('NONE','NONE', #5873, #8075 ) REPRESENTATION_RELATIONSHIP_WITH_TRANSFORMATION ( #21075 )SHAPE_REPRESENTATION_RELATIONSHIP( ) );
#19729 = CARTESIAN_POINT ( 'NONE',  ( 33.58253175000000823, 78.02500000273118985, 10.91162601494192863 ) ) ;
#19730 = CARTESIAN_POINT ( 'NONE',  ( 26.00068869287340334, 43.94010416666665719, -15.01150461594642316 ) ) ;
#19731 = DIRECTION ( 'NONE',  ( -0.000000000000000000, 1.000000000000000000, -0.000000000000000000 ) ) ;
#19732 = ORIENTED_EDGE ( 'NONE', *, *, #20285, .F. ) ;
#19733 = CARTESIAN_POINT ( 'NONE',  ( -25.98046417659859486, 51.10715250092397355, -15.04653450569291628 ) ) ;
#19734 = CARTESIAN_POINT ( 'NONE',  ( 32.50000000000000000, 11.60000000546238397, -10.55989012756945833 ) ) ;
#19735 = CARTESIAN_POINT ( 'NONE',  ( 28.01184896238304134, 61.55729166666666430, 7.505752307972846538 ) ) ;
#19736 = DIRECTION ( 'NONE',  ( -0.000000000000000000, -1.000000000000000000, -0.000000000000000000 ) ) ;
#19737 = CARTESIAN_POINT ( 'NONE',  ( -33.58253175000000113, 41.37500000273119838, 0.000000000000000000 ) ) ;
#19738 = CARTESIAN_POINT ( 'NONE',  ( -20.08610463437156923, 46.80000000546235839, 27.64615127144130113 ) ) ;
#19739 = CARTESIAN_POINT ( 'NONE',  ( -13.91746824999999532, 75.27500000273118985, -4.522059556121115875 ) ) ;
#19740 = CARTESIAN_POINT ( 'NONE',  ( -33.58253175000000113, 27.22500000273119269, 10.91162601494193929 ) ) ;
#19741 = CARTESIAN_POINT ( 'NONE',  ( 32.50000000000000000, 31.60000000546237686, -10.55989012756945833 ) ) ;
#19742 = CARTESIAN_POINT ( 'NONE',  ( -33.58253175000000113, 53.47500000273117848, 10.91162601494193929 ) ) ;
#19743 = CARTESIAN_POINT ( 'NONE',  ( 6.277390505771533514E-15, 34.49999999999998579, 34.17252228774368916 ) ) ;
#19744 = CARTESIAN_POINT ( 'NONE',  ( 20.08610463437158344, 36.70000000000000995, 27.64615127144129403 ) ) ;
#19745 = CARTESIAN_POINT ( 'NONE',  ( -14.47279130897152122, 11.92499999726882010, 19.92008829642072243 ) ) ;
#19746 = CARTESIAN_POINT ( 'NONE',  ( -33.58253175000000113, 73.12500000273119838, 0.000000000000000000 ) ) ;
#19747 = CARTESIAN_POINT ( 'NONE',  ( 26.29305231718578995, 13.19999999999998863, -19.10302069950538240 ) ) ;
#19748 = CARTESIAN_POINT ( 'NONE',  ( 8.601468415847516980, 80.67500000273118133, -11.83890561707634603 ) ) ;
#19749 = CARTESIAN_POINT ( 'NONE',  ( -10.37757302488623701, 63.77500000273117564, 31.93888565452638417 ) ) ;
#19750 = CARTESIAN_POINT ( 'NONE',  ( -15.00000000000000000, 76.15000000546238823, -4.873795443493594171 ) ) ;
#19751 = CARTESIAN_POINT ( 'NONE',  ( 5.779280353836490358E-15, 55.00000000546238965, 32.49999999999999289 ) ) ;
#19752 = CARTESIAN_POINT ( 'NONE',  ( 19.82091636218621389, 5.949999994537630066, -14.40073868116559197 ) ) ;
#19753 = CARTESIAN_POINT ( 'NONE',  ( 19.11951029504763611, 21.17225666759064850, -19.06425588902591173 ) ) ;
#19754 = CARTESIAN_POINT ( 'NONE',  ( -12.13525491562420910, 74.45000000546237118, 8.816778784387098611 ) ) ;
#19755 = CARTESIAN_POINT ( 'NONE',  ( -27.16883889988624290, 38.92500000273117422, -19.73931689729374028 ) ) ;
#19756 = CARTESIAN_POINT ( 'NONE',  ( 20.75514604977249178, 6.075000002731190563, 28.56700777964553950 ) ) ;
#19757 = CARTESIAN_POINT ( 'NONE',  ( -33.58253175000000113, 53.47500000273117848, 10.91162601494193929 ) ) ;
#19758 = CARTESIAN_POINT ( 'NONE',  ( 2.584737979205442066E-13, 55.39843749999999289, 27.95245687107223276 ) ) ;
#19759 = CARTESIAN_POINT ( 'NONE',  ( 28.02196122052045268, 38.64621500092395934, -7.468012846824774620 ) ) ;
#19760 = CARTESIAN_POINT ( 'NONE',  ( 7.468012846824281681, 42.07253499907601935, -28.02196122052058058 ) ) ;
#19761 = CARTESIAN_POINT ( 'NONE',  ( 6.277390505771533514E-15, 65.00000000546236834, 34.17252228774368916 ) ) ;
#19762 = CARTESIAN_POINT ( 'NONE',  ( 13.91746824999999887, 71.87500000273122680, -1.704398294459741270E-15 ) ) ;
#19763 = CARTESIAN_POINT ( 'NONE',  ( 19.11951029504797006, 53.53086833240935505, 19.06425588902558133 ) ) ;
#19764 = CARTESIAN_POINT ( 'NONE',  ( -26.29305231718579350, 53.79999999999999716, -19.10302069950537884 ) ) ;
#19765 = CARTESIAN_POINT ( 'NONE',  ( -19.82091636218621389, 4.949999994537629178, 14.40073868116558842 ) ) ;
#19766 = VERTEX_POINT ( 'NONE', #30638 ) ;
#19767 = CARTESIAN_POINT ( 'NONE',  ( 33.58253175000000113, 40.47500000273118559, -10.91162601494193751 ) ) ;
#19768 = CARTESIAN_POINT ( 'NONE',  ( -18.94512977948575738, 3.924999997268807661, -13.76444248337723231 ) ) ;
#19769 = CARTESIAN_POINT ( 'NONE',  ( -32.50000000000000000, 28.60000000546238397, 10.55989012756946366 ) ) ;
#19770 = EDGE_LOOP ( 'NONE', ( #17068, #8835 ) ) ;
#19771 = CARTESIAN_POINT ( 'NONE',  ( 26.00068869287367335, 34.20052083333332860, 15.01150461594596308 ) ) ;
#19772 = ORIENTED_EDGE ( 'NONE', *, *, #28858, .T. ) ;
#19773 = CARTESIAN_POINT ( 'NONE',  ( 5.779280353836490358E-15, 26.50000000000000711, 32.49999999999999289 ) ) ;
#19774 = CIRCLE ( 'NONE', #24173, 32.63512777199724724 ) ;
#19775 = CARTESIAN_POINT ( 'NONE',  ( 20.75514604977249178, 47.82500000273117990, 28.56700777964553950 ) ) ;
#19776 = CARTESIAN_POINT ( 'NONE',  ( -20.50609665441004736, 56.68749999999998579, -20.50609665440969565 ) ) ;
#19777 = CARTESIAN_POINT ( 'NONE',  ( 10.04305231718579705, 13.10000000546238041, 30.90933677959248982 ) ) ;
#19778 = CARTESIAN_POINT ( 'NONE',  ( -9.270509831248423538, 77.70000000000001705, -12.75976212528059861 ) ) ;
#19779 = CARTESIAN_POINT ( 'NONE',  ( -23.41746825000000243, 16.22499999726880304, 7.608796670333725309 ) ) ;
#19780 = CARTESIAN_POINT ( 'NONE',  ( 20.08610463437157279, 55.29999999999999716, -27.64615127144129758 ) ) ;
#19781 = CARTESIAN_POINT ( 'NONE',  ( 33.58253175000000113, 14.47500000273118737, -10.91162601494193751 ) ) ;
#19782 = DIRECTION ( 'NONE',  ( 0.000000000000000000, 1.000000000000000000, 0.000000000000000000 ) ) ;
#19783 = CARTESIAN_POINT ( 'NONE',  ( -6.950374756619247307, 23.16628499907601579, 26.09010956794245217 ) ) ;
#19784 = CARTESIAN_POINT ( 'NONE',  ( 2.688165632520823219E-15, 73.37500000273118417, 14.63369212191046387 ) ) ;
#19785 = DIRECTION ( 'NONE',  ( 0.000000000000000000, 0.000000000000000000, 1.000000000000000000 ) ) ;
#19786 = FACE_OUTER_BOUND ( 'NONE', #8910, .T. ) ;
#19787 = CARTESIAN_POINT ( 'NONE',  ( 10.37757302488624056, 78.77500000273117564, -31.93888565452638417 ) ) ;
#19788 = ORIENTED_EDGE ( 'NONE', *, *, #29081, .T. ) ;
#19789 = CARTESIAN_POINT ( 'NONE',  ( 7.236395654485755280, 4.724999997268803043, 22.27133577429736988 ) ) ;
#19790 = CARTESIAN_POINT ( 'NONE',  ( 13.91746824999999887, 71.87500000273119838, -1.704398294459741270E-15 ) ) ;
#19791 = VECTOR ( 'NONE', #10301, 1000.000000000000000 ) ;
#19792 = CARTESIAN_POINT ( 'NONE',  ( -6.988114217767819270, 45.22916666666665719, 26.07999730980490583 ) ) ;
#19793 = CARTESIAN_POINT ( 'NONE',  ( 6.486482029760649416E-15, 67.62500000273119838, 35.31076352940723240 ) ) ;
#19794 = CARTESIAN_POINT ( 'NONE',  ( -27.16883889988624290, 25.17500000273119198, -19.73931689729374028 ) ) ;
#19795 = CARTESIAN_POINT ( 'NONE',  ( 10.37757302488624056, 14.77500000273117209, -31.93888565452638417 ) ) ;
#19796 = CARTESIAN_POINT ( 'NONE',  ( 33.58253175000000113, 8.375000002731169957, -4.112674001490185761E-15 ) ) ;
#19797 = CARTESIAN_POINT ( 'NONE',  ( 28.02196122052045268, 14.58371500092397710, -7.468012846824774620 ) ) ;
#19798 = CARTESIAN_POINT ( 'NONE',  ( 28.01184896238304134, 51.24479166666666430, 7.505752307972846538 ) ) ;
#19799 = CARTESIAN_POINT ( 'NONE',  ( 4.300734207923757602, 72.77500000273118985, -13.23629886949340673 ) ) ;
#19800 = CARTESIAN_POINT ( 'NONE',  ( -10.04305231718578462, 48.39999999999998437, 30.90933677959249337 ) ) ;
#19801 = VECTOR ( 'NONE', #12658, 1000.000000000000000 ) ;
#19802 = AXIS2_PLACEMENT_3D ( 'NONE', #7105, #25305, #30092 ) ;
#19803 = CARTESIAN_POINT ( 'NONE',  ( 6.001560367445586717E-15, 3.249999994537631665, 24.50000000000000000 ) ) ;
#19804 = CARTESIAN_POINT ( 'NONE',  ( -33.58253175000000113, 49.12500000273117706, 0.000000000000000000 ) ) ;
#19805 = CARTESIAN_POINT ( 'NONE',  ( 7.236395654485760609, 5.024999997268825069, -22.27133577429736633 ) ) ;
#19806 = VERTEX_POINT ( 'NONE', #30466 ) ;
#19807 = CARTESIAN_POINT ( 'NONE',  ( -20.75514604977248112, 59.67500000273118133, 28.56700777964554661 ) ) ;
#19808 = CARTESIAN_POINT ( 'NONE',  ( 5.779280353836490358E-15, 2.500000000000005329, 32.49999999999999289 ) ) ;
#19809 = CARTESIAN_POINT ( 'NONE',  ( 23.41746825000000243, 10.52499999726880731, 7.608796670333735079 ) ) ;
#19810 = CARTESIAN_POINT ( 'NONE',  ( -14.01125832528285109, 36.49777750092397355, 24.18731323226248264 ) ) ;
#19811 = ORIENTED_EDGE ( 'NONE', *, *, #5178, .F. ) ;
#19812 = CARTESIAN_POINT ( 'NONE',  ( -20.75514604977248112, 33.42500000273120264, 28.56700777964554661 ) ) ;
#19813 = CARTESIAN_POINT ( 'NONE',  ( -32.50000000000000000, 34.50000000546238255, 0.000000000000000000 ) ) ;
#19814 = ORIENTED_EDGE ( 'NONE', *, *, #18037, .T. ) ;
#19815 = CARTESIAN_POINT ( 'NONE',  ( -30.02300923189239512, 59.69531250000000711, 2.654126918244515359E-13 ) ) ;
#19816 = CARTESIAN_POINT ( 'NONE',  ( 20.75514604977248467, 62.67500000273117422, -28.56700777964554305 ) ) ;
#19817 = CARTESIAN_POINT ( 'NONE',  ( -20.08610463437156923, 36.80000000546239391, 27.64615127144130113 ) ) ;
#19818 = CARTESIAN_POINT ( 'NONE',  ( 33.58253175000000823, 68.02500000273117564, 10.91162601494192863 ) ) ;
#19819 = CARTESIAN_POINT ( 'NONE',  ( 15.01150461594643204, 34.48697916666667140, 26.00068869287340334 ) ) ;
#19820 = CARTESIAN_POINT ( 'NONE',  ( -4.732186688966233175E-15, 11.49999999999998579, 25.76082449383753925 ) ) ;
#19821 = CARTESIAN_POINT ( 'NONE',  ( 10.37757302488624056, 4.775000002731177418, -31.93888565452638417 ) ) ;
#19822 = CARTESIAN_POINT ( 'NONE',  ( -10.37757302488623701, 7.525000002731207616, 31.93888565452638417 ) ) ;
#19823 = CARTESIAN_POINT ( 'NONE',  ( 0.000000000000000000, 122.0000000000000000, 0.000000000000000000 ) ) ;
#19824 = CARTESIAN_POINT ( 'NONE',  ( -30.02300923189239867, 41.06993083240934794, 0.04044903255044988294 ) ) ;
#19825 = CARTESIAN_POINT ( 'NONE',  ( 2.897257156509938333E-15, 78.49999999999998579, 15.77193336357400710 ) ) ;
#19826 = CARTESIAN_POINT ( 'NONE',  ( -28.01184896238304134, 56.40104166666666430, -7.505752307972844761 ) ) ;
#19827 = DIRECTION ( 'NONE',  ( -1.000000000000000000, 0.000000000000000000, 0.000000000000000000 ) ) ;
#19828 = CARTESIAN_POINT ( 'NONE',  ( 15.14183272437242245, 8.049999994537621717, -20.84094480462497856 ) ) ;
#19829 = CARTESIAN_POINT ( 'NONE',  ( -9.657523855033125146E-16, 79.75000000546236834, -15.77193336357400710 ) ) ;
#19830 = CARTESIAN_POINT ( 'NONE',  ( -19.11951029504797006, 68.99961833240934084, -19.06425588902558133 ) ) ;
#19831 = CARTESIAN_POINT ( 'NONE',  ( 27.16883889988623935, 40.32500000273120122, -19.73931689729374384 ) ) ;
#19832 = CARTESIAN_POINT ( 'NONE',  ( -13.91746824999999532, 72.97500000273120691, 4.522059556121122093 ) ) ;
#19833 = CARTESIAN_POINT ( 'NONE',  ( -33.58253175000000113, 43.27500000273117564, -10.91162601494193218 ) ) ;
#19834 = CARTESIAN_POINT ( 'NONE',  ( -20.75514604977248823, 31.07500000273118701, -28.56700777964554305 ) ) ;
#19835 = DIRECTION ( 'NONE',  ( -1.000000000000000000, -1.224646799147353454E-16, 0.000000000000000000 ) ) ;
#19836 = CARTESIAN_POINT ( 'NONE',  ( 0.000000000000000000, 70.00000000000000000, 0.000000000000000000 ) ) ;
#19837 = CARTESIAN_POINT ( 'NONE',  ( 5.779280353836490358E-15, 27.00000000546237544, 32.49999999999999289 ) ) ;
#19838 = CARTESIAN_POINT ( 'NONE',  ( 10.04305231718579705, 64.60000000000000853, 30.90933677959248982 ) ) ;
#19839 = CARTESIAN_POINT ( 'NONE',  ( 7.236395654485760609, 9.024999997268800200, -22.27133577429736633 ) ) ;
#19840 = CARTESIAN_POINT ( 'NONE',  ( -28.00173670424535644, 23.73920166574268364, 7.543491769121936308 ) ) ;
#19841 = CARTESIAN_POINT ( 'NONE',  ( 18.94512977948576093, 5.324999997268820451, -13.76444248337722875 ) ) ;
#19842 = CARTESIAN_POINT ( 'NONE',  ( 27.95245687107223276, 35.91368083240935505, -0.04044903255042905932 ) ) ;
#19843 = ADVANCED_FACE ( 'NONE', ( #17450 ), #2673, .T. ) ;
#19844 = DIRECTION ( 'NONE',  ( 0.000000000000000000, 0.000000000000000000, -1.000000000000000000 ) ) ;
#19845 = CARTESIAN_POINT ( 'NONE',  ( -27.16883889988624290, 12.92500000273116889, -19.73931689729374028 ) ) ;
#19846 = CARTESIAN_POINT ( 'NONE',  ( 18.94512977948575738, 14.92499999726881654, 13.76444248337723408 ) ) ;
#19847 = CARTESIAN_POINT ( 'NONE',  ( -6.988114217767819270, 65.85416666666665719, 26.07999730980490583 ) ) ;
#19848 = ORIENTED_EDGE ( 'NONE', *, *, #8117, .T. ) ;
#19849 = CARTESIAN_POINT ( 'NONE',  ( 33.58253175000000113, 50.22500000273118559, -10.91162601494193751 ) ) ;
#19850 = CARTESIAN_POINT ( 'NONE',  ( -20.75514604977248823, 23.07500000273117635, -28.56700777964554305 ) ) ;
#19851 = VERTEX_POINT ( 'NONE', #23916 ) ;
#19852 = CARTESIAN_POINT ( 'NONE',  ( 20.50609665441005092, 37.78124999999999289, 20.50609665440969209 ) ) ;
#19853 = CARTESIAN_POINT ( 'NONE',  ( -20.53372385742071771, 29.76600666759063429, 20.47846945139902530 ) ) ;
#19854 = CARTESIAN_POINT ( 'NONE',  ( -1.756012107511856980E-14, 2.500000000000005773, -24.50000000000000000 ) ) ;
#19855 = CARTESIAN_POINT ( 'NONE',  ( -24.50000000000001066, 14.84999999453764019, 7.960532557706201828 ) ) ;
#19856 = ADVANCED_FACE ( 'NONE', ( #388 ), #8954, .T. ) ;
#19857 = CARTESIAN_POINT ( 'NONE',  ( 14.47279130897151767, 8.924999997268800556, -19.92008829642072598 ) ) ;
#19858 = CARTESIAN_POINT ( 'NONE',  ( -27.16883889988624290, 25.17500000273117777, -19.73931689729374028 ) ) ;
#19859 = CARTESIAN_POINT ( 'NONE',  ( -10.04305231718579172, 24.10000000546236265, -30.90933677959248982 ) ) ;
#19860 = AXIS2_PLACEMENT_3D ( 'NONE', #27775, #11817, #32738 ) ;
#19861 = CARTESIAN_POINT ( 'NONE',  ( -26.29305231718578995, 70.19999999999998863, 19.10302069950538595 ) ) ;
#19862 = CARTESIAN_POINT ( 'NONE',  ( -32.50000000000000000, 6.600000005462382191, 10.55989012756946366 ) ) ;
#19863 = CARTESIAN_POINT ( 'NONE',  ( -14.09332452378496470, 74.00000000000002842, 4.636822204800125746 ) ) ;
#19864 = CARTESIAN_POINT ( 'NONE',  ( 7.468012846824777284, 56.69309000092396644, 28.02196122052045268 ) ) ;
#19865 = CARTESIAN_POINT ( 'NONE',  ( -27.16883889988624290, 35.17500000273118843, -19.73931689729374028 ) ) ;
#19866 = CARTESIAN_POINT ( 'NONE',  ( 20.75514604977249178, 55.82500000273118701, 28.56700777964553950 ) ) ;
#19867 = CARTESIAN_POINT ( 'NONE',  ( 26.00068869287367690, 27.32552083333333215, 15.01150461594596486 ) ) ;
#19868 =( LENGTH_UNIT ( ) NAMED_UNIT ( * ) SI_UNIT ( .MILLI., .METRE. ) );
#19869 = CIRCLE ( 'NONE', #27535, 15.00000000000000000 ) ;
#19870 = CARTESIAN_POINT ( 'NONE',  ( 23.41746824999999887, 13.12499999726882116, 0.000000000000000000 ) ) ;
#19871 = CARTESIAN_POINT ( 'NONE',  ( -26.29305231718579350, 13.79999999999997939, -19.10302069950537884 ) ) ;
#19872 = CARTESIAN_POINT ( 'NONE',  ( 15.14183272437241889, 17.69999999999999218, 20.84094480462498211 ) ) ;
#19873 = CARTESIAN_POINT ( 'NONE',  ( -24.22776226481266448, 44.79388916574269075, -13.94119854578892514 ) ) ;
#19874 = CARTESIAN_POINT ( 'NONE',  ( -20.75514604977248823, 56.82500000273117990, -28.56700777964554305 ) ) ;
#19875 = CARTESIAN_POINT ( 'NONE',  ( 27.16883889988623935, 48.57500000273118701, -19.73931689729374384 ) ) ;
#19876 = CARTESIAN_POINT ( 'NONE',  ( 26.29305231718579350, 44.80000000000000426, 19.10302069950537529 ) ) ;
#19877 = CARTESIAN_POINT ( 'NONE',  ( 20.08610463437158344, 67.20000000546235697, 27.64615127144129403 ) ) ;
#19878 = CARTESIAN_POINT ( 'NONE',  ( -10.04305231718578462, 6.400000000000016342, 30.90933677959249337 ) ) ;
#19879 = CARTESIAN_POINT ( 'NONE',  ( -7.025853678916393008, 46.66704833425730925, 26.06988505166735592 ) ) ;
#19880 = CARTESIAN_POINT ( 'NONE',  ( -17.34916400531743363, 16.99999999999998579, -16.72523852671361766 ) ) ;
#19881 = LINE ( 'NONE', #30334, #7818 ) ;
#19882 = CARTESIAN_POINT ( 'NONE',  ( -10.37757302488624411, 20.72500000273118204, -31.93888565452638417 ) ) ;
#19883 = DIRECTION ( 'NONE',  ( -1.000000000000000000, -1.224646799147353454E-16, 0.000000000000000000 ) ) ;
#19884 = CARTESIAN_POINT ( 'NONE',  ( -4.223320258572821363E-15, 78.75000000546236834, 15.00000000000000355 ) ) ;
#19885 = CARTESIAN_POINT ( 'NONE',  ( 0.000000000000000000, 80.00000000000001421, -32.50000000000000000 ) ) ;
#19886 = CARTESIAN_POINT ( 'NONE',  ( 25.98046417659831775, 66.56472249907604066, -15.04653450569338879 ) ) ;
#19887 = CARTESIAN_POINT ( 'NONE',  ( -10.04305231718579172, 42.10000000546236265, -30.90933677959248982 ) ) ;
#19888 = CARTESIAN_POINT ( 'NONE',  ( -20.08610463437157989, 60.20000000546237828, -27.64615127144129758 ) ) ;
#19890 = CARTESIAN_POINT ( 'NONE',  ( -27.16883889988623935, 29.32500000273119412, 19.73931689729374739 ) ) ;
#19889 = CIRCLE ( 'NONE', #3455, 31.91025403784435710 ) ;
#19891 = CARTESIAN_POINT ( 'NONE',  ( -2.162160676586881955E-15, 64.87500000273119838, -35.31076352940723240 ) ) ;
#19892 = CARTESIAN_POINT ( 'NONE',  ( -13.97622843553588901, 38.49739583333332860, 24.20753774853756823 ) ) ;
#19893 = ORIENTED_EDGE ( 'NONE', *, *, #8508, .T. ) ;
#19894 = AXIS2_PLACEMENT_3D ( 'NONE', #12789, #33725, #7469 ) ;
#19895 = CARTESIAN_POINT ( 'NONE',  ( -10.37757302488624411, 70.72500000273117848, -31.93888565452638417 ) ) ;
#19896 = CARTESIAN_POINT ( 'NONE',  ( -2.584737979205441561E-13, 39.92968750000000000, -30.02300923189239512 ) ) ;
#19897 =( BOUNDED_CURVE ( )  B_SPLINE_CURVE ( 2, ( #15577, #23631, #21398, #10757, #10587, #7834, #13508, #5092, #8008, #3035, #21064, #29270, #31678 ),
 .UNSPECIFIED., .F., .T. ) 
 B_SPLINE_CURVE_WITH_KNOTS ( ( 3, 2, 2, 2, 2, 2, 3 ),
 ( 0.6474358974358974672, 0.6487179487179487447, 0.6512820512820512997, 0.6538461538461538547, 0.6564102564102564097, 0.6589743589743589647, 0.6602564102564102422 ),
 .UNSPECIFIED. ) 
 CURVE ( )  GEOMETRIC_REPRESENTATION_ITEM ( )  RATIONAL_B_SPLINE_CURVE ( ( 0.9755282581475768211, 0.9755282581475768211, 1.000000000000000000, 0.9510565162951535312, 1.000000000000000000, 0.9510565162951535312, 1.000000000000000000, 0.9510565162951535312, 1.000000000000000000, 0.9510565162951535312, 1.000000000000000000, 0.9755282581475768211, 0.9755282581475768211 ) ) 
 REPRESENTATION_ITEM ( '' )  );
#19898 = DIRECTION ( 'NONE',  ( -0.7069718413157914938, -0.01953538259431466736, 0.7069718413158002646 ) ) ;
#19899 = VERTEX_POINT ( 'NONE', #30047 ) ;
#19900 = CARTESIAN_POINT ( 'NONE',  ( 28.00173670424549499, 59.55767333425731636, 7.543491769121417612 ) ) ;
#19901 = CARTESIAN_POINT ( 'NONE',  ( -6.950374756619716266, 58.41184000092398065, -26.09010956794232428 ) ) ;
#19902 = CARTESIAN_POINT ( 'NONE',  ( -26.29305231718579350, 8.300000005462369046, -19.10302069950537884 ) ) ;
#19903 = CARTESIAN_POINT ( 'NONE',  ( -20.50609665440969209, 66.14062500000000000, 20.50609665441005092 ) ) ;
#19904 = CARTESIAN_POINT ( 'NONE',  ( -32.50000000000000000, 64.50000000546238255, 0.000000000000000000 ) ) ;
#19905 = CARTESIAN_POINT ( 'NONE',  ( -27.16883889988624290, 41.17500000273119554, -19.73931689729374028 ) ) ;
#19906 = CARTESIAN_POINT ( 'NONE',  ( -20.08610463437156923, 42.80000000546236549, 27.64615127144130113 ) ) ;
#19907 = CARTESIAN_POINT ( 'NONE',  ( 4.300734207923761154, 71.97500000273122112, 13.23629886949340495 ) ) ;
#19908 = CARTESIAN_POINT ( 'NONE',  ( 10.37757302488624056, 32.52500000273117564, -31.93888565452638417 ) ) ;
#19909 = CARTESIAN_POINT ( 'NONE',  ( -10.04305231718578462, 24.40000000000000568, 30.90933677959249337 ) ) ;
#19910 = CARTESIAN_POINT ( 'NONE',  ( -10.37757302488624411, 54.97500000273119980, -31.93888565452638417 ) ) ;
#19911 =( NAMED_UNIT ( * ) SI_UNIT ( $, .STERADIAN. ) SOLID_ANGLE_UNIT ( ) );
#19912 = CARTESIAN_POINT ( 'NONE',  ( -32.50000000000000000, 38.09999999999999432, 10.55989012756946366 ) ) ;
#19913 = CARTESIAN_POINT ( 'NONE',  ( -26.29305231718579350, 31.79999999999999361, -19.10302069950537884 ) ) ;
#19914 = CARTESIAN_POINT ( 'NONE',  ( -19.82091636218621389, 1.200000000000006617, 14.40073868116558842 ) ) ;
#19915 = EDGE_CURVE ( 'NONE', #5805, #28550, #41, .T. ) ;
#19916 = CARTESIAN_POINT ( 'NONE',  ( -20.75514604977248823, 78.82500000273120122, -28.56700777964554305 ) ) ;
#19917 = DIRECTION ( 'NONE',  ( 0.000000000000000000, 0.000000000000000000, 1.000000000000000000 ) ) ;
#19918 = CARTESIAN_POINT ( 'NONE',  ( -8.601468415847515203, 77.67500000273122396, 11.83890561707634959 ) ) ;
#19919 = CARTESIAN_POINT ( 'NONE',  ( -10.37757302488624411, 68.97500000273117848, -31.93888565452638417 ) ) ;
#19920 = CARTESIAN_POINT ( 'NONE',  ( -15.00000000000000000, 78.35000000546239107, 4.873795443493597723 ) ) ;
#19921 = ADVANCED_FACE ( 'NONE', ( #24737 ), #6716, .F. ) ;
#19922 = VECTOR ( 'NONE', #28665, 1000.000000000000000 ) ;
#19923 = ORIENTED_EDGE ( 'NONE', *, *, #755, .T. ) ;
#19924 = CARTESIAN_POINT ( 'NONE',  ( -19.82091636218621034, 12.54999999453762527, -14.40073868116559552 ) ) ;
#19925 = CARTESIAN_POINT ( 'NONE',  ( 19.06425588902592239, 18.59413166759064140, 19.11951029504763611 ) ) ;
#19926 = LINE ( 'NONE', #4300, #11858 ) ;
#19927 = CARTESIAN_POINT ( 'NONE',  ( 10.37757302488624056, 38.52500000273119696, -31.93888565452638417 ) ) ;
#19928 = CARTESIAN_POINT ( 'NONE',  ( 10.37757302488624056, 2.775000002731189852, -31.93888565452638417 ) ) ;
#19929 = CARTESIAN_POINT ( 'NONE',  ( -33.58253175000000113, 53.27500000273118275, -10.91162601494193041 ) ) ;
#19930 = CARTESIAN_POINT ( 'NONE',  ( 20.47846945139902530, 46.09413166759064495, 20.53372385742071771 ) ) ;
#19931 = CARTESIAN_POINT ( 'NONE',  ( -20.53372385742107653, 34.62461833240934794, -20.47846945139867003 ) ) ;
#19932 = CARTESIAN_POINT ( 'NONE',  ( 32.50000000000000000, 61.60000000546236976, -10.55989012756945833 ) ) ;
#19933 = CARTESIAN_POINT ( 'NONE',  ( -11.25946833292375793, 71.07500000273120122, 8.180482586598737171 ) ) ;
#19934 = CARTESIAN_POINT ( 'NONE',  ( -24.22776226481266448, 61.98138916574268364, -13.94119854578892514 ) ) ;
#19935 = CARTESIAN_POINT ( 'NONE',  ( -15.31642273298460744, -59.03347138510255832, 0.000000000000000000 ) ) ;
#19936 = CARTESIAN_POINT ( 'NONE',  ( -10.04305231718579172, 74.10000000546237686, -30.90933677959248982 ) ) ;
#19937 = CARTESIAN_POINT ( 'NONE',  ( 7.505752307972854531, 12.57291666666666252, -28.01184896238303423 ) ) ;
#19938 = CARTESIAN_POINT ( 'NONE',  ( -33.58253175000000113, 39.27500000273118275, -10.91162601494193218 ) ) ;
#19939 = CARTESIAN_POINT ( 'NONE',  ( -7.236395654485757944, 1.724999997268800156, -22.27133577429736988 ) ) ;
#19940 = VERTEX_POINT ( 'NONE', #6883 ) ;
#19941 = AXIS2_PLACEMENT_3D ( 'NONE', #23315, #18172, #20752 ) ;
#19942 = CARTESIAN_POINT ( 'NONE',  ( 20.08610463437157279, 27.80000000546238326, -27.64615127144129758 ) ) ;
#19943 = ORIENTED_EDGE ( 'NONE', *, *, #9844, .T. ) ;
#19944 = VECTOR ( 'NONE', #9481, 1000.000000000000000 ) ;
#19945 = CARTESIAN_POINT ( 'NONE',  ( -26.00068869287340334, 31.90885416666666430, 15.01150461594643382 ) ) ;
#19946 = CARTESIAN_POINT ( 'NONE',  ( -32.50000000000000000, 62.40000000546235981, -10.55989012756945478 ) ) ;
#19947 = VERTEX_POINT ( 'NONE', #14618 ) ;
#19948 = CARTESIAN_POINT ( 'NONE',  ( -32.50000000000000000, 74.50000000546236834, 0.000000000000000000 ) ) ;
#19949 = CARTESIAN_POINT ( 'NONE',  ( 20.75514604977249178, 45.82500000273118701, 28.56700777964553950 ) ) ;
#19950 = CARTESIAN_POINT ( 'NONE',  ( 5.147494310547434893, 55.05125428700924317, 32.49999999999999289 ) ) ;
#19951 = CARTESIAN_POINT ( 'NONE',  ( -1.778240108872766143E-15, 47.49999999999999289, -32.49999999999999289 ) ) ;
#19952 = CARTESIAN_POINT ( 'NONE',  ( 10.04305231718578817, 9.900000005462372243, -30.90933677959249337 ) ) ;
#19953 = CARTESIAN_POINT ( 'NONE',  ( -29.51723652120143981, 66.96161537668497488, -16.50702486923799128 ) ) ;
#19954 = CARTESIAN_POINT ( 'NONE',  ( 7.236395654485755280, 14.72499999726881192, 22.27133577429736988 ) ) ;
#19955 = CARTESIAN_POINT ( 'NONE',  ( 32.50000000000000000, 53.09999999999998721, -10.55989012756945833 ) ) ;
#19956 = EDGE_CURVE ( 'NONE', #2905, #15118, #32787, .T. ) ;
#19957 = CARTESIAN_POINT ( 'NONE',  ( -7.236395654485757944, 1.224999997268799712, -22.27133577429736988 ) ) ;
#19958 = CARTESIAN_POINT ( 'NONE',  ( 10.37757302488624056, 18.77500000273118985, -31.93888565452638417 ) ) ;
#19959 = CARTESIAN_POINT ( 'NONE',  ( -32.50000000000000000, 74.00000000000001421, 0.000000000000000000 ) ) ;
#19960 = CARTESIAN_POINT ( 'NONE',  ( -0.04044903255042732459, 28.17930583240935860, -27.95245687107223986 ) ) ;
#19961 = CARTESIAN_POINT ( 'NONE',  ( 4.300734207923761154, 75.47500000273119269, 13.23629886949340495 ) ) ;
#19962 = CYLINDRICAL_SURFACE ( 'NONE', #14045, 24.50000000000000000 ) ;
#19963 = CARTESIAN_POINT ( 'NONE',  ( -32.50000000000000000, 43.90000000000001279, -10.55989012756945300 ) ) ;
#19964 = EDGE_CURVE ( 'NONE', #22660, #3077, #30557, .T. ) ;
#19965 = CARTESIAN_POINT ( 'NONE',  ( -2.162160676586881955E-15, 78.87500000273118417, -35.31076352940723240 ) ) ;
#19966 = ORIENTED_EDGE ( 'NONE', *, *, #19034, .T. ) ;
#19967 = CARTESIAN_POINT ( 'NONE',  ( -18.94512977948575738, 3.924999997268807661, -13.76444248337723231 ) ) ;
#19968 = LINE ( 'NONE', #30414, #11789 ) ;
#19969 = CARTESIAN_POINT ( 'NONE',  ( -26.07999730980477437, 49.23958333333332860, 6.988114217768305103 ) ) ;
#19970 = CARTESIAN_POINT ( 'NONE',  ( -20.75514604977248823, 62.82500000273119412, -28.56700777964554305 ) ) ;
#19971 = CARTESIAN_POINT ( 'NONE',  ( 6.486482029760649416E-15, 25.87500000273117351, 35.31076352940723240 ) ) ;
#19972 = CARTESIAN_POINT ( 'NONE',  ( 33.58253175000000113, 8.375000002731184168, -4.112674001490185761E-15 ) ) ;
#19973 = CYLINDRICAL_SURFACE ( 'NONE', #22078, 32.50000000000000000 ) ;
#19974 = CARTESIAN_POINT ( 'NONE',  ( -20.53372385742071771, 16.01600666759064140, 20.47846945139902530 ) ) ;
#19975 = CARTESIAN_POINT ( 'NONE',  ( -7.505752307972844761, 58.97916666666666430, 28.01184896238304134 ) ) ;
#19976 = CARTESIAN_POINT ( 'NONE',  ( 10.37757302488624767, 7.725000002731172266, 31.93888565452638417 ) ) ;
#19977 = CARTESIAN_POINT ( 'NONE',  ( 5.147494310547426899, 69.44874571845315359, -32.50000000000000000 ) ) ;
#19978 = CARTESIAN_POINT ( 'NONE',  ( 10.04305231718579705, 44.60000000000001563, 30.90933677959248982 ) ) ;
#19979 = CARTESIAN_POINT ( 'NONE',  ( -33.58253175000000113, 53.02500000273118985, -10.91162601494193041 ) ) ;
#19980 = CARTESIAN_POINT ( 'NONE',  ( 7.236395654485755280, 2.224999997268800378, 22.27133577429736988 ) ) ;
#19981 = CARTESIAN_POINT ( 'NONE',  ( -24.20753774853756823, 66.85677083333332860, -13.97622843553588723 ) ) ;
#19982 = ORIENTED_EDGE ( 'NONE', *, *, #27320, .T. ) ;
#19983 = CARTESIAN_POINT ( 'NONE',  ( -33.58253175000000113, 61.47500000273117848, 10.91162601494193929 ) ) ;
#19984 = CARTESIAN_POINT ( 'NONE',  ( 5.779280353836490358E-15, 16.50000000000000000, 32.49999999999999289 ) ) ;
#19985 = CARTESIAN_POINT ( 'NONE',  ( 1.507698388325705758E-15, 11.12499999726881761, -24.62258325217400312 ) ) ;
#19986 = CARTESIAN_POINT ( 'NONE',  ( 19.06425588902592239, 32.34413166759064495, 19.11951029504763611 ) ) ;
#19987 = ORIENTED_EDGE ( 'NONE', *, *, #15988, .F. ) ;
#19988 = CARTESIAN_POINT ( 'NONE',  ( 33.58253175000000113, 32.12500000273120548, -4.112674001490185761E-15 ) ) ;
#19989 = CARTESIAN_POINT ( 'NONE',  ( -10.04305231718579172, 34.10000000546236976, -30.90933677959248982 ) ) ;
#19990 = AXIS2_PLACEMENT_3D ( 'NONE', #6653, #25183, #17134 ) ;
#19991 = ORIENTED_EDGE ( 'NONE', *, *, #21409, .T. ) ;
#19992 = CARTESIAN_POINT ( 'NONE',  ( -20.50609665441004736, 60.12500000000000000, -20.50609665440969565 ) ) ;
#19993 = CARTESIAN_POINT ( 'NONE',  ( -2.375766604868041476, 76.44874571845316780, 14.99999999999999822 ) ) ;
#19994 = CARTESIAN_POINT ( 'NONE',  ( -10.37757302488623701, 67.52500000273120406, 31.93888565452638417 ) ) ;
#19995 = CARTESIAN_POINT ( 'NONE',  ( 20.50609665440969565, 40.35937499999999289, -20.50609665441004736 ) ) ;
#19996 = CARTESIAN_POINT ( 'NONE',  ( -7.570916362186215665, 11.39999999999999325, 23.30088464923126423 ) ) ;
#19997 = CARTESIAN_POINT ( 'NONE',  ( -10.37757302488623701, 5.775000002731179194, 31.93888565452638417 ) ) ;
#19998 = CARTESIAN_POINT ( 'NONE',  ( -10.37757302488624411, 12.72500000273119092, -31.93888565452638417 ) ) ;
#19999 =( BOUNDED_CURVE ( )  B_SPLINE_CURVE ( 2, ( #18580, #24057, #26290, #13244, #18746, #10843, #28855, #7589, #7924, #2779, #525, #21152, #359 ),
 .UNSPECIFIED., .F., .T. ) 
 B_SPLINE_CURVE_WITH_KNOTS ( ( 3, 2, 2, 2, 2, 2, 3 ),
 ( 0.3141025641025640969, 0.3153846153846153744, 0.3179487179487179294, 0.3205128205128205399, 0.3230769230769230949, 0.3256410256410256499, 0.3269230769230769273 ),
 .UNSPECIFIED. ) 
 CURVE ( )  GEOMETRIC_REPRESENTATION_ITEM ( )  RATIONAL_B_SPLINE_CURVE ( ( 0.9755282581475768211, 0.9755282581475768211, 1.000000000000000000, 0.9510565162951535312, 1.000000000000000000, 0.9510565162951535312, 1.000000000000000000, 0.9510565162951535312, 1.000000000000000000, 0.9510565162951535312, 1.000000000000000000, 0.9755282581475768211, 0.9755282581475768211 ) ) 
 REPRESENTATION_ITEM ( '' )  );
#20000 = CARTESIAN_POINT ( 'NONE',  ( -13.91746824999999532, 70.97500000273117848, 4.522059556121122093 ) ) ;
#20001 = CARTESIAN_POINT ( 'NONE',  ( -25.98046417659831420, 54.53347249907601935, 15.04653450569339945 ) ) ;
#20002 = CARTESIAN_POINT ( 'NONE',  ( -12.13525491562420910, 72.19999999999998863, 8.816778784387098611 ) ) ;
#20003 = CARTESIAN_POINT ( 'NONE',  ( -26.00068869287368756, 56.54427083333332860, -15.01150461594595775 ) ) ;
#20004 = CARTESIAN_POINT ( 'NONE',  ( -19.82091636218621034, 14.54999999453762705, -14.40073868116559552 ) ) ;
#20005 = CARTESIAN_POINT ( 'NONE',  ( 32.50000000000000000, 61.60000000546236265, -10.55989012756945833 ) ) ;
#20006 = CARTESIAN_POINT ( 'NONE',  ( 24.50000000000000355, 5.849999994537631309, -7.960532557706203605 ) ) ;
#20007 = CARTESIAN_POINT ( 'NONE',  ( 2.897257156509938333E-15, 74.75000000546235412, 15.77193336357400710 ) ) ;
#20008 = CARTESIAN_POINT ( 'NONE',  ( -19.09188309203660694, 21.45312499999999645, 19.09188309203694800 ) ) ;
#20009 = CARTESIAN_POINT ( 'NONE',  ( -33.58253175000000113, 37.02500000273117564, -10.91162601494193218 ) ) ;
#20010 = CARTESIAN_POINT ( 'NONE',  ( 27.16883889988623935, 76.32500000273120122, -19.73931689729374384 ) ) ;
#20011 = CARTESIAN_POINT ( 'NONE',  ( 33.58253175000000823, 40.27500000273118985, 10.91162601494192863 ) ) ;
#20012 = CARTESIAN_POINT ( 'NONE',  ( 10.37757302488624056, 24.77500000273119696, -31.93888565452638417 ) ) ;
#20013 = DIRECTION ( 'NONE',  ( -1.224646799147353454E-16, 1.000000000000000000, -0.000000000000000000 ) ) ;
#20014 = CARTESIAN_POINT ( 'NONE',  ( -5.147494310547430452, 8.051254287009218302, -32.49999999999999289 ) ) ;
#20015 = PRESENTATION_LAYER_ASSIGNMENT (  '', '', ( #26044 ) ) ;
#20016 = CARTESIAN_POINT ( 'NONE',  ( 10.04305231718578817, 33.39999999999998437, -30.90933677959249337 ) ) ;
#20017 = CARTESIAN_POINT ( 'NONE',  ( 26.29305231718578995, 65.20000000000001705, -19.10302069950538240 ) ) ;
#20018 = CARTESIAN_POINT ( 'NONE',  ( -14.47279130897151767, 9.324999997268816898, -19.92008829642072598 ) ) ;
#20019 = CARTESIAN_POINT ( 'NONE',  ( -20.53372385742107653, 27.74961833240935505, -20.47846945139867003 ) ) ;
#20020 = CARTESIAN_POINT ( 'NONE',  ( 23.41746824999999887, 1.124999997268810725, 0.000000000000000000 ) ) ;
#20021 = CARTESIAN_POINT ( 'NONE',  ( 26.06988505166722803, 39.20795166574269075, -7.025853678916862854 ) ) ;
#20022 = FILL_AREA_STYLE ('',( #3890 ) ) ;
#20023 = CARTESIAN_POINT ( 'NONE',  ( -2.162160676586882350E-15, 10.62500000273119483, -35.31076352940722529 ) ) ;
#20024 = CARTESIAN_POINT ( 'NONE',  ( 23.41746825000000243, 13.22499999726881192, -7.608796670333727974 ) ) ;
#20025 = CARTESIAN_POINT ( 'NONE',  ( 19.09188309203694800, 61.84374999999998579, 19.09188309203660694 ) ) ;
#20026 = ORIENTED_EDGE ( 'NONE', *, *, #7791, .T. ) ;
#20027 = CARTESIAN_POINT ( 'NONE',  ( -33.58253175000000113, 47.12500000273119127, 0.000000000000000000 ) ) ;
#20028 = CARTESIAN_POINT ( 'NONE',  ( 33.58253175000000113, 24.47500000273118914, -10.91162601494193751 ) ) ;
#20029 = VERTEX_POINT ( 'NONE', #19935 ) ;
#20030 = CARTESIAN_POINT ( 'NONE',  ( -28.01184896238304134, 35.77604166666666430, -7.505752307972844761 ) ) ;
#20031 = CARTESIAN_POINT ( 'NONE',  ( 14.97647472619947351, 29.04986083425730570, 26.02091320914850314 ) ) ;
#20032 = CARTESIAN_POINT ( 'NONE',  ( 3.445340210940985210E-14, 9.249999994537636994, 24.50000000000000000 ) ) ;
#20033 = CARTESIAN_POINT ( 'NONE',  ( -7.570916362186215665, 15.14999999453761603, 23.30088464923126423 ) ) ;
#20034 = CARTESIAN_POINT ( 'NONE',  ( 7.236395654485755280, 10.22499999726880837, 22.27133577429736988 ) ) ;
#20035 = CARTESIAN_POINT ( 'NONE',  ( 6.486482029760649416E-15, 21.87500000273118062, 35.31076352940723240 ) ) ;
#20036 = MECHANICAL_DESIGN_GEOMETRIC_PRESENTATION_REPRESENTATION (  '', ( #5249 ), #9618 ) ;
#20037 = CARTESIAN_POINT ( 'NONE',  ( 10.04305231718579705, 25.10000000546236265, 30.90933677959248982 ) ) ;
#20038 = CARTESIAN_POINT ( 'NONE',  ( 26.29305231718579350, 66.79999999999999716, 19.10302069950537529 ) ) ;
#20039 = CARTESIAN_POINT ( 'NONE',  ( 10.04305231718579705, 47.10000000546238397, 30.90933677959248982 ) ) ;
#20040 = CARTESIAN_POINT ( 'NONE',  ( -5.609029516820829286, 74.00000000000004263, 13.21632355367902711 ) ) ;
#20041 = CARTESIAN_POINT ( 'NONE',  ( -26.02091320914849959, 64.28423583425730214, 14.97647472619947528 ) ) ;
#20042 = CARTESIAN_POINT ( 'NONE',  ( 6.486482029760649416E-15, 37.87500000273117706, 35.31076352940723240 ) ) ;
#20043 = CYLINDRICAL_SURFACE ( 'NONE', #5394, 32.50000000000000000 ) ;
#20044 = CARTESIAN_POINT ( 'NONE',  ( 30.02300923189239867, 30.47656250000000355, -2.619432448724978208E-13 ) ) ;
#20045 = SURFACE_SIDE_STYLE ('',( #12488 ) ) ;
#20046 = CARTESIAN_POINT ( 'NONE',  ( -23.41746825000000598, 14.22499999726880660, 7.608796670333726198 ) ) ;
#20047 = CARTESIAN_POINT ( 'NONE',  ( 32.50000000000000000, 17.10000000000001208, -10.55989012756945833 ) ) ;
#20048 = CARTESIAN_POINT ( 'NONE',  ( 19.11951029504797006, 39.78086833240934794, 19.06425588902558133 ) ) ;
#20049 = CARTESIAN_POINT ( 'NONE',  ( -10.37757302488623701, 57.52500000273119696, 31.93888565452638417 ) ) ;
#20050 = COLOUR_RGB ( '', 0.31764706, 0.68627451, 0.89019608) ;
#20051 = CARTESIAN_POINT ( 'NONE',  ( 33.58253175000000113, 60.47500000273118559, -10.91162601494193751 ) ) ;
#20052 = CARTESIAN_POINT ( 'NONE',  ( 10.37757302488624767, 49.97500000273119269, 31.93888565452638417 ) ) ;
#20053 = CARTESIAN_POINT ( 'NONE',  ( 5.779280353836490358E-15, 44.49999999999999289, 32.49999999999999289 ) ) ;
#20054 = ADVANCED_FACE ( 'NONE', ( #22006 ), #1212, .F. ) ;
#20055 = DIRECTION ( 'NONE',  ( 0.000000000000000000, 1.000000000000000000, 0.000000000000000000 ) ) ;
#20056 = CARTESIAN_POINT ( 'NONE',  ( -12.11607355459419821, -70.99969134886156041, 2.663817581893346643E-15 ) ) ;
#20057 = CARTESIAN_POINT ( 'NONE',  ( 0.04044903254993986036, 44.80506916759064495, -27.95245687107223986 ) ) ;
#20058 = CARTESIAN_POINT ( 'NONE',  ( 20.08610463437157279, 63.80000000546237970, -27.64615127144129758 ) ) ;
#20059 = CARTESIAN_POINT ( 'NONE',  ( -32.52223864317537050, 52.00000000000001421, 1.355835680407736499 ) ) ;
#20060 = CARTESIAN_POINT ( 'NONE',  ( -10.37757302488624411, 24.72500000273118559, -31.93888565452638417 ) ) ;
#20061 = LINE ( 'NONE', #27269, #12194 ) ;
#20062 = CARTESIAN_POINT ( 'NONE',  ( 0.000000000000000000, -10.99999999999999645, 0.000000000000000000 ) ) ;
#20063 = EDGE_CURVE ( 'NONE', #33963, #30034, #8366, .T. ) ;
#20064 = CARTESIAN_POINT ( 'NONE',  ( -1.756012107511856980E-14, 4.249999994537631665, -24.50000000000000000 ) ) ;
#20065 = CARTESIAN_POINT ( 'NONE',  ( 25.98046417659831775, 63.12722249907601224, -15.04653450569338879 ) ) ;
#20066 = CARTESIAN_POINT ( 'NONE',  ( -20.08610463437156923, 40.80000000546237260, 27.64615127144130113 ) ) ;
#20067 = CARTESIAN_POINT ( 'NONE',  ( -26.29305231718578995, 60.70000000546238539, 19.10302069950538595 ) ) ;
#20068 = CARTESIAN_POINT ( 'NONE',  ( -20.75514604977248112, 35.42500000273119554, 28.56700777964554661 ) ) ;
#20069 = CARTESIAN_POINT ( 'NONE',  ( 20.75514604977249178, 66.07500000273118701, 28.56700777964553950 ) ) ;
#20070 = CARTESIAN_POINT ( 'NONE',  ( 6.988114217767829928, 36.63541666666666430, -26.07999730980489872 ) ) ;
#20071 = ORIENTED_EDGE ( 'NONE', *, *, #17349, .F. ) ;
#20072 = EDGE_CURVE ( 'NONE', #4440, #871, #1724, .T. ) ;
#20073 = CARTESIAN_POINT ( 'NONE',  ( 20.75514604977249178, 69.82500000273118701, 28.56700777964553950 ) ) ;
#20074 = CARTESIAN_POINT ( 'NONE',  ( 15.01150461594596308, 36.77864583333332860, -26.00068869287367335 ) ) ;
#20075 = CARTESIAN_POINT ( 'NONE',  ( -26.29305231718578995, 16.70000000546237473, 19.10302069950538595 ) ) ;
#20076 = ORIENTED_EDGE ( 'NONE', *, *, #2221, .T. ) ;
#20077 = CARTESIAN_POINT ( 'NONE',  ( 20.53372385742072481, 58.98475666759065206, -20.47846945139902175 ) ) ;
#20078 = CARTESIAN_POINT ( 'NONE',  ( 26.06988505166735592, 56.12017333425732346, 7.025853678916393896 ) ) ;
#20079 = VECTOR ( 'NONE', #12404, 1000.000000000000000 ) ;
#20080 = CARTESIAN_POINT ( 'NONE',  ( -27.16883889988623935, 13.32500000273119412, 19.73931689729374739 ) ) ;
#20081 = CARTESIAN_POINT ( 'NONE',  ( 20.47846945139867003, 18.29649333240935150, -20.53372385742107653 ) ) ;
#20082 = CARTESIAN_POINT ( 'NONE',  ( -32.50000000000000000, 45.99999999999998579, 0.000000000000000000 ) ) ;
#20083 = CARTESIAN_POINT ( 'NONE',  ( -20.75514604977248823, 43.07500000273118701, -28.56700777964554305 ) ) ;
#20084 = CARTESIAN_POINT ( 'NONE',  ( 6.277390505771533514E-15, 47.00000000546238965, 34.17252228774368916 ) ) ;
#20085 = CARTESIAN_POINT ( 'NONE',  ( -4.635254915624211769, 81.60000000000000853, -14.26584774442730286 ) ) ;
#20086 = CARTESIAN_POINT ( 'NONE',  ( 33.58253175000000113, 26.22500000273119625, -10.91162601494193751 ) ) ;
#20087 = DIRECTION ( 'NONE',  ( 0.000000000000000000, 0.000000000000000000, 1.000000000000000000 ) ) ;
#20088 = CARTESIAN_POINT ( 'NONE',  ( 27.16883889988623935, 58.57500000273119412, -19.73931689729374384 ) ) ;
#20089 = CARTESIAN_POINT ( 'NONE',  ( 26.29305231718578995, 33.19999999999999574, -19.10302069950538240 ) ) ;
#20090 = CARTESIAN_POINT ( 'NONE',  ( 32.50000000000000711, 30.89999999999998437, 10.55989012756945122 ) ) ;
#20091 = CARTESIAN_POINT ( 'NONE',  ( 1.507698388325705758E-15, 17.12499999726880517, -24.62258325217400312 ) ) ;
#20092 = CARTESIAN_POINT ( 'NONE',  ( 6.486482029760649416E-15, 75.62500000273121259, 35.31076352940723240 ) ) ;
#20093 = DIRECTION ( 'NONE',  ( -0.7071067811865467956, 0.7071067811865483499, 0.000000000000000000 ) ) ;
#20094 = CARTESIAN_POINT ( 'NONE',  ( -32.50000000000000000, 20.60000000546237686, 10.55989012756946366 ) ) ;
#20095 = CARTESIAN_POINT ( 'NONE',  ( 27.16883889988623935, 66.57500000273120122, -19.73931689729374384 ) ) ;
#20096 = CARTESIAN_POINT ( 'NONE',  ( -12.13525491562421088, 78.05000000546242234, -8.816778784387096835 ) ) ;
#20097 = ORIENTED_EDGE ( 'NONE', *, *, #29070, .T. ) ;
#20098 = CARTESIAN_POINT ( 'NONE',  ( 33.58253175000000113, 16.22500000273118914, -10.91162601494193751 ) ) ;
#20099 = CARTESIAN_POINT ( 'NONE',  ( 1.577395562988744260E-15, 8.249999994537613901, -25.76082449383753925 ) ) ;
#20100 = CARTESIAN_POINT ( 'NONE',  ( -14.01125832528285109, 19.31027750092397710, 24.18731323226248264 ) ) ;
#20101 = CARTESIAN_POINT ( 'NONE',  ( 3.445340210940985210E-14, 7.249999994537621895, 24.50000000000000000 ) ) ;
#20102 = CARTESIAN_POINT ( 'NONE',  ( -33.58253175000000113, 43.22500000273118559, 10.91162601494193929 ) ) ;
#20103 = CARTESIAN_POINT ( 'NONE',  ( -27.16883889988623935, 5.575000002731187010, 19.73931689729374739 ) ) ;
#20104 = CARTESIAN_POINT ( 'NONE',  ( 33.58253175000000113, 58.47500000273119269, -10.91162601494193574 ) ) ;
#20105 = CARTESIAN_POINT ( 'NONE',  ( 28.00173670424549499, 49.24517333425730925, 7.543491769121417612 ) ) ;
#20106 = CIRCLE ( 'NONE', #8048, 32.50000000000000000 ) ;
#20107 = CARTESIAN_POINT ( 'NONE',  ( -0.04044903255044120238, 35.05430583240935505, -30.02300923189239867 ) ) ;
#20108 = CARTESIAN_POINT ( 'NONE',  ( 32.50000000000000000, 61.50000000546239676, -3.980102097228898626E-15 ) ) ;
#20109 = CARTESIAN_POINT ( 'NONE',  ( -8.601468415847518756, 74.57500000273120122, -11.83890561707634781 ) ) ;
#20110 =( BOUNDED_CURVE ( )  B_SPLINE_CURVE ( 2, ( #11095, #18992, #18491, #18825, #19156, #440, #29436, #2694, #28934, #603, #268, #13154, #3204 ),
 .UNSPECIFIED., .F., .T. ) 
 B_SPLINE_CURVE_WITH_KNOTS ( ( 3, 2, 2, 2, 2, 2, 3 ),
 ( 0.8525641025641025328, 0.8538461538461538103, 0.8564102564102563653, 0.8589743589743589203, 0.8615384615384615863, 0.8641025641025641413, 0.8653846153846154188 ),
 .UNSPECIFIED. ) 
 CURVE ( )  GEOMETRIC_REPRESENTATION_ITEM ( )  RATIONAL_B_SPLINE_CURVE ( ( 0.9755282581475768211, 0.9755282581475768211, 1.000000000000000000, 0.9510565162951535312, 1.000000000000000000, 0.9510565162951535312, 1.000000000000000000, 0.9510565162951535312, 1.000000000000000000, 0.9510565162951535312, 1.000000000000000000, 0.9755282581475768211, 0.9755282581475768211 ) ) 
 REPRESENTATION_ITEM ( '' )  );
#20111 = CARTESIAN_POINT ( 'NONE',  ( 14.01125832528330051, 60.54909749907603356, 24.18731323226221974 ) ) ;
#20112 = DIRECTION ( 'NONE',  ( -0.000000000000000000, -1.000000000000000000, -0.000000000000000000 ) ) ;
#20113 = CARTESIAN_POINT ( 'NONE',  ( 26.29305231718578995, 75.70000000546239960, -19.10302069950538240 ) ) ;
#20114 = CARTESIAN_POINT ( 'NONE',  ( 26.00068869287367335, 13.57552083333332682, 15.01150461594596308 ) ) ;
#20115 = EDGE_CURVE ( 'NONE', #23284, #19851, #27996, .T. ) ;
#20116 = CARTESIAN_POINT ( 'NONE',  ( 20.75514604977248467, 38.67500000273117422, -28.56700777964554305 ) ) ;
#20117 = CARTESIAN_POINT ( 'NONE',  ( -23.41746825000000243, 8.224999997268822582, 7.608796670333725309 ) ) ;
#20118 = ORIENTED_EDGE ( 'NONE', *, *, #30881, .F. ) ;
#20119 = CARTESIAN_POINT ( 'NONE',  ( -20.75514604977248823, 77.07500000273117280, -28.56700777964554305 ) ) ;
#20120 = CARTESIAN_POINT ( 'NONE',  ( 32.50000000000000000, 31.50000000546236834, -3.980102097228898626E-15 ) ) ;
#20121 = ORIENTED_EDGE ( 'NONE', *, *, #18277, .F. ) ;
#20122 = CARTESIAN_POINT ( 'NONE',  ( 26.00068869287367335, 37.63802083333331439, 15.01150461594596308 ) ) ;
#20123 = CARTESIAN_POINT ( 'NONE',  ( -10.04305231718578462, 64.90000000546235981, 30.90933677959249337 ) ) ;
#20124 = ORIENTED_EDGE ( 'NONE', *, *, #18935, .T. ) ;
#20125 = CARTESIAN_POINT ( 'NONE',  ( -32.50000000000000000, 74.60000000546234844, 10.55989012756946366 ) ) ;
#20126 = CARTESIAN_POINT ( 'NONE',  ( -33.58253175000000113, 51.12500000273117706, 0.000000000000000000 ) ) ;
#20127 = CARTESIAN_POINT ( 'NONE',  ( 9.270509831248421762, 73.55000000546237970, -12.75976212528059861 ) ) ;
#20128 = CARTESIAN_POINT ( 'NONE',  ( 26.29305231718579350, 5.300000005462379704, 19.10302069950537529 ) ) ;
#20129 = CARTESIAN_POINT ( 'NONE',  ( -20.08610463437156923, 8.300000000000000711, 27.64615127144130113 ) ) ;
#20130 = CARTESIAN_POINT ( 'NONE',  ( 7.505752307972854531, 12.57291666666666252, -28.01184896238303423 ) ) ;
#20131 = CARTESIAN_POINT ( 'NONE',  ( -32.50000000000000000, 52.10000000000001563, 10.55989012756946366 ) ) ;
#20132 = CARTESIAN_POINT ( 'NONE',  ( -32.50000000000000000, 14.09999999999999076, 10.55989012756946366 ) ) ;
#20133 = CARTESIAN_POINT ( 'NONE',  ( -20.75514604977248823, 19.07500000273118701, -28.56700777964554305 ) ) ;
#20134 = DIRECTION ( 'NONE',  ( 0.000000000000000000, 0.000000000000000000, -1.000000000000000000 ) ) ;
#20135 = CARTESIAN_POINT ( 'NONE',  ( 27.95245687107223276, 25.60118083240935860, -0.04044903255042905932 ) ) ;
#20136 = CARTESIAN_POINT ( 'NONE',  ( 8.601468415847516980, 76.67500000273116711, -11.83890561707634781 ) ) ;
#20137 = DIRECTION ( 'NONE',  ( 0.000000000000000000, 0.000000000000000000, 1.000000000000000000 ) ) ;
#20138 = CARTESIAN_POINT ( 'NONE',  ( 26.29305231718578995, 53.70000000546237828, -19.10302069950538240 ) ) ;
#20139 = CIRCLE ( 'NONE', #13012, 9.000000000000001776 ) ;
#20140 = CARTESIAN_POINT ( 'NONE',  ( 6.277390505771533514E-15, 4.500000000000003553, 34.17252228774368916 ) ) ;
#20141 = ORIENTED_EDGE ( 'NONE', *, *, #31700, .F. ) ;
#20142 = CARTESIAN_POINT ( 'NONE',  ( 23.41746825000000243, 15.02499999726881086, 7.608796670333735079 ) ) ;
#20143 = CARTESIAN_POINT ( 'NONE',  ( -13.91746824999999887, 70.87500000273119838, 0.000000000000000000 ) ) ;
#20144 = CARTESIAN_POINT ( 'NONE',  ( 24.20753774853756113, 51.38802083333332149, 13.97622843553589789 ) ) ;
#20145 = CARTESIAN_POINT ( 'NONE',  ( -27.16883889988624290, 62.92500000273119554, -19.73931689729374028 ) ) ;
#20146 = CARTESIAN_POINT ( 'NONE',  ( -20.75514604977248112, 23.67500000273118843, 28.56700777964554661 ) ) ;
#20147 = CARTESIAN_POINT ( 'NONE',  ( 33.58253175000000113, 12.37500000273118772, -4.112674001490185761E-15 ) ) ;
#20148 = DIRECTION ( 'NONE',  ( -0.000000000000000000, -1.000000000000000000, -0.000000000000000000 ) ) ;
#20149 = CARTESIAN_POINT ( 'NONE',  ( -7.468012846824771955, 17.16184000092397000, -28.02196122052045624 ) ) ;
#20150 = CARTESIAN_POINT ( 'NONE',  ( 15.01150461594643204, 65.42447916666667140, 26.00068869287340334 ) ) ;
#20151 = CARTESIAN_POINT ( 'NONE',  ( 26.29305231718579350, 77.30000000546237970, 19.10302069950537529 ) ) ;
#20152 = CARTESIAN_POINT ( 'NONE',  ( 5.779280353836490358E-15, 68.49999999999998579, 32.49999999999999289 ) ) ;
#20153 = CARTESIAN_POINT ( 'NONE',  ( -20.08610463437157989, 43.69999999999998863, -27.64615127144129758 ) ) ;
#20154 = CARTESIAN_POINT ( 'NONE',  ( -33.58253175000000113, 47.12500000273117706, 0.000000000000000000 ) ) ;
#20155 = CARTESIAN_POINT ( 'NONE',  ( 14.47279130897151589, 2.324999997268805796, 19.92008829642072953 ) ) ;
#20156 = CARTESIAN_POINT ( 'NONE',  ( 32.50000000000000000, 21.50000000546237189, -3.980102097228898626E-15 ) ) ;
#20157 = VERTEX_POINT ( 'NONE', #14959 ) ;
#20158 = ADVANCED_FACE ( 'NONE', ( #1045 ), #11525, .T. ) ;
#20159 = CARTESIAN_POINT ( 'NONE',  ( -33.58253175000000113, 61.37500000273120548, 0.000000000000000000 ) ) ;
#20160 = CARTESIAN_POINT ( 'NONE',  ( 26.29305231718578995, 43.20000000000001705, -19.10302069950538240 ) ) ;
#20161 = CARTESIAN_POINT ( 'NONE',  ( -14.47279130897151589, 13.32499999726880624, -19.92008829642072598 ) ) ;
#20162 = CARTESIAN_POINT ( 'NONE',  ( 24.18731323226247554, 28.76340250092398065, 14.01125832528285997 ) ) ;
#20163 = EDGE_CURVE ( 'NONE', #14665, #9893, #245, .T. ) ;
#20164 = ORIENTED_EDGE ( 'NONE', *, *, #31033, .F. ) ;
#20165 = CARTESIAN_POINT ( 'NONE',  ( -33.58253175000000113, 33.22500000273117138, 10.91162601494193929 ) ) ;
#20166 = CARTESIAN_POINT ( 'NONE',  ( -13.91746824999999887, 81.12500000273121259, 0.000000000000000000 ) ) ;
#20167 = ORIENTED_EDGE ( 'NONE', *, *, #32298, .F. ) ;
#20168 = CARTESIAN_POINT ( 'NONE',  ( -1.778240108872766143E-15, 36.00000000546238255, -32.49999999999999289 ) ) ;
#20169 = CARTESIAN_POINT ( 'NONE',  ( -10.37757302488623701, 69.52500000273120406, 31.93888565452638417 ) ) ;
#20170 = CARTESIAN_POINT ( 'NONE',  ( -2.584737979205441561E-13, 43.36718749999999289, -30.02300923189239512 ) ) ;
#20171 = CARTESIAN_POINT ( 'NONE',  ( 15.14183272437242245, 10.29999999999999361, -20.84094480462497856 ) ) ;
#20172 = CARTESIAN_POINT ( 'NONE',  ( 7.236395654485760609, 1.524999997268822183, -22.27133577429736633 ) ) ;
#20173 = CARTESIAN_POINT ( 'NONE',  ( -33.58253175000000113, 13.22500000273119802, 10.91162601494193929 ) ) ;
#20174 = CARTESIAN_POINT ( 'NONE',  ( 28.02196122052058413, 56.68190999907602645, 7.468012846824272799 ) ) ;
#20175 = CARTESIAN_POINT ( 'NONE',  ( 9.270509831248425314, 74.70000000000000284, 12.75976212528059683 ) ) ;
#20176 = CARTESIAN_POINT ( 'NONE',  ( 26.00068869287341045, 54.25260416666666430, -15.01150461594642493 ) ) ;
#20177 = CARTESIAN_POINT ( 'NONE',  ( 10.04305231718579705, 19.10000000546238752, 30.90933677959248982 ) ) ;
#20178 = CARTESIAN_POINT ( 'NONE',  ( -4.635254915624208216, 74.65000000546240244, 14.26584774442730463 ) ) ;
#20179 = CARTESIAN_POINT ( 'NONE',  ( -7.570916362186215665, 15.14999999453761603, 23.30088464923126423 ) ) ;
#20180 = CARTESIAN_POINT ( 'NONE',  ( -15.00000000000000000, 74.35000000546237686, 4.873795443493597723 ) ) ;
#20181 = CARTESIAN_POINT ( 'NONE',  ( 27.95245687107222921, 23.60156250000000000, -2.463307335887066074E-13 ) ) ;
#20182 = CARTESIAN_POINT ( 'NONE',  ( 6.486482029760649416E-15, 39.62500000273117706, 35.31076352940723240 ) ) ;
#20183 = CARTESIAN_POINT ( 'NONE',  ( -11.25946833292375793, 71.07500000273120122, 8.180482586598737171 ) ) ;
#20184 = CARTESIAN_POINT ( 'NONE',  ( -33.58253175000000113, 45.47500000273119980, 10.91162601494193929 ) ) ;
#20185 = CARTESIAN_POINT ( 'NONE',  ( -10.37757302488623701, 21.77500000273119340, 31.93888565452638417 ) ) ;
#20186 = CARTESIAN_POINT ( 'NONE',  ( 20.08610463437157279, 41.30000000000000426, -27.64615127144129758 ) ) ;
#20187 = APPLICATION_CONTEXT ( 'automotive_design' ) ;
#20188 = CARTESIAN_POINT ( 'NONE',  ( 15.14183272437242422, 2.299999999999985612, -20.84094480462497856 ) ) ;
#20189 = VECTOR ( 'NONE', #5627, 1000.000000000000000 ) ;
#20190 = CARTESIAN_POINT ( 'NONE',  ( 26.29305231718578995, 33.20000000000000995, -19.10302069950538240 ) ) ;
#20191 = CARTESIAN_POINT ( 'NONE',  ( -2.092463501923844636E-15, 57.49999999999999289, -34.17252228774368916 ) ) ;
#20192 = CARTESIAN_POINT ( 'NONE',  ( -14.47279130897152299, 9.924999997268827201, 19.92008829642072243 ) ) ;
#20193 = CARTESIAN_POINT ( 'NONE',  ( -27.16883889988623935, 65.32500000273117280, 19.73931689729374739 ) ) ;
#20194 = CARTESIAN_POINT ( 'NONE',  ( -4.635254915624208216, 78.39999999999996305, 14.26584774442730463 ) ) ;
#20195 = CARTESIAN_POINT ( 'NONE',  ( 27.95245687107223276, 39.35118083240935505, -0.04044903255042905932 ) ) ;
#20196 = CARTESIAN_POINT ( 'NONE',  ( -33.58253175000000113, 79.27500000273118985, -10.91162601494193218 ) ) ;
#20197 = CARTESIAN_POINT ( 'NONE',  ( -33.58253175000000113, 15.02500000273119873, -10.91162601494193041 ) ) ;
#20198 = CARTESIAN_POINT ( 'NONE',  ( 7.236395654485760609, 11.52499999726880375, -22.27133577429736633 ) ) ;
#20199 = CARTESIAN_POINT ( 'NONE',  ( 2.584737979205441561E-13, 65.71093749999997158, 27.95245687107222921 ) ) ;
#20200 = EDGE_LOOP ( 'NONE', ( #16868, #13411, #26195, #28972 ) ) ;
#20201 = CARTESIAN_POINT ( 'NONE',  ( -20.75514604977248823, 52.82500000273116569, -28.56700777964554305 ) ) ;
#20202 = CARTESIAN_POINT ( 'NONE',  ( -33.58253175000000113, 23.47500000273119269, 10.91162601494193929 ) ) ;
#20203 = EDGE_CURVE ( 'NONE', #18278, #10457, #28673, .T. ) ;
#20204 = ADVANCED_FACE ( 'NONE', ( #15653 ), #23024, .T. ) ;
#20205 =( BOUNDED_CURVE ( )  B_SPLINE_CURVE ( 2, ( #24772, #1250, #9153, #30552, #17530, #14954, #1898, #29165, #5502, #24038, #8234, #18557, #20796, #163, #2594, #10653, #21303, #2419, #15982, #18388, #10483, #28497, #29001, #18222, #10823, #31907, #3104, #2930, #7732, #13222, #26438, #20961, #18728, #10992, #507, #28668, #13400, #28834, #21131, #15813, #31573, #23870, #5161, #23697, #338, #31411, #5673, #21465, #8402, #15646, #31743, #5332, #8071, #26268, #16153, #2756, #33823, #23362, #26606, #12886, #13575, #25925, #13057, #18890, #4990, #15472, #10317, #31240, #26097, #23530, #7904 ),
 .UNSPECIFIED., .F., .T. ) 
 B_SPLINE_CURVE_WITH_KNOTS ( ( 3, 2, 2, 2, 2, 2, 2, 2, 2, 2, 2, 2, 2, 2, 2, 2, 2, 2, 2, 2, 2, 2, 2, 2, 2, 2, 2, 2, 2, 2, 2, 2, 2, 2, 2, 3 ),
 ( 0.000000000000000000, 0.02000000000000000042, 0.04000000000000000083, 0.05999999999999999778, 0.08000000000000000167, 0.1000000000000000056, 0.1199999999999999956, 0.1400000000000000133, 0.1600000000000000033, 0.1799999999999999933, 0.2000000000000000111, 0.2200000000000000289, 0.2399999999999999911, 0.2600000000000000089, 0.2800000000000000266, 0.2999999999999999889, 0.3200000000000000067, 0.3400000000000000244, 0.3599999999999999867, 0.3800000000000000044, 0.4000000000000000222, 0.4200000000000000400, 0.4400000000000000577, 0.4600000000000000755, 0.4799999999999999822, 0.5000000000000000000, 0.5200000000000000178, 0.5400000000000000355, 0.5600000000000000533, 0.5799999999999999600, 0.5999999999999999778, 0.6199999999999999956, 0.6400000000000000133, 0.6600000000000000311, 0.6800000000000000488, 0.6875575298689673431 ),
 .UNSPECIFIED. ) 
 CURVE ( )  GEOMETRIC_REPRESENTATION_ITEM ( )  RATIONAL_B_SPLINE_CURVE ( ( 1.000000000000000000, 0.9510565162951535312, 1.000000000000000000, 0.9510565162951535312, 1.000000000000000000, 0.9510565162951535312, 1.000000000000000000, 0.9510565162951535312, 1.000000000000000000, 0.9510565162951535312, 1.000000000000000000, 0.9510565162951535312, 1.000000000000000000, 0.9510565162951535312, 1.000000000000000000, 0.9510565162951535312, 1.000000000000000000, 0.9510565162951535312, 1.000000000000000000, 0.9510565162951535312, 1.000000000000000000, 0.9510565162951535312, 1.000000000000000000, 0.9510565162951535312, 1.000000000000000000, 0.9510565162951535312, 1.000000000000000000, 0.9510565162951535312, 1.000000000000000000, 0.9510565162951535312, 1.000000000000000000, 0.9510565162951535312, 1.000000000000000000, 0.9510565162951535312, 1.000000000000000000, 0.9510565162951535312, 1.000000000000000000, 0.9510565162951535312, 1.000000000000000000, 0.9510565162951535312, 1.000000000000000000, 0.9510565162951535312, 1.000000000000000000, 0.9510565162951535312, 1.000000000000000000, 0.9510565162951535312, 1.000000000000000000, 0.9510565162951535312, 1.000000000000000000, 0.9510565162951535312, 1.000000000000000000, 0.9510565162951535312, 1.000000000000000000, 0.9510565162951535312, 1.000000000000000000, 0.9510565162951535312, 1.000000000000000000, 0.9510565162951535312, 1.000000000000000000, 0.9510565162951535312, 1.000000000000000000, 0.9510565162951535312, 1.000000000000000000, 0.9510565162951535312, 1.000000000000000000, 0.9510565162951535312, 1.000000000000000000, 0.9510565162951535312, 1.000000000000000000, 0.9815054080004653736, 0.9769881591460154446 ) ) 
 REPRESENTATION_ITEM ( '' )  );
#20206 = VERTEX_POINT ( 'NONE', #25598 ) ;
#20207 = CARTESIAN_POINT ( 'NONE',  ( -20.50609665440969209, 31.76562499999999289, 20.50609665441005092 ) ) ;
#20208 = CARTESIAN_POINT ( 'NONE',  ( -14.97647472619946285, 34.20611083425730925, -26.02091320914851025 ) ) ;
#20209 = FACE_OUTER_BOUND ( 'NONE', #5300, .T. ) ;
#20210 = CYLINDRICAL_SURFACE ( 'NONE', #11271, 15.00000000000000000 ) ;
#20211 = CARTESIAN_POINT ( 'NONE',  ( 7.236395654485755280, 6.724999997268804819, 22.27133577429736988 ) ) ;
#20212 = CARTESIAN_POINT ( 'NONE',  ( -4.523095164977116484E-15, 10.12499999726881938, 24.62258325217400312 ) ) ;
#20213 = CARTESIAN_POINT ( 'NONE',  ( -10.37757302488624411, 18.97500000273119625, -31.93888565452638417 ) ) ;
#20214 = CARTESIAN_POINT ( 'NONE',  ( -32.50000000000000000, 24.50000000546237544, 0.000000000000000000 ) ) ;
#20215 = CARTESIAN_POINT ( 'NONE',  ( -32.50000000000000000, 68.09999999999995168, 10.55989012756946366 ) ) ;
#20216 = CARTESIAN_POINT ( 'NONE',  ( 7.570916362186213000, 12.14999999453764090, -23.30088464923126423 ) ) ;
#20217 = CARTESIAN_POINT ( 'NONE',  ( -10.57675453070074312, 74.00000000000000000, 10.05591069532431625 ) ) ;
#20218 = CARTESIAN_POINT ( 'NONE',  ( 7.543491769121427382, 62.13579833425730925, -28.00173670424548433 ) ) ;
#20219 = CARTESIAN_POINT ( 'NONE',  ( -10.37757302488624411, 30.97500000273117848, -31.93888565452638417 ) ) ;
#20220 = DIRECTION ( 'NONE',  ( -0.000000000000000000, -1.000000000000000000, -0.000000000000000000 ) ) ;
#20221 = CARTESIAN_POINT ( 'NONE',  ( 15.01150461594643382, 34.48697916666666430, 26.00068869287340334 ) ) ;
#20222 = DIRECTION ( 'NONE',  ( 1.000000000000000000, 0.000000000000000000, 0.000000000000000000 ) ) ;
#20223 = CARTESIAN_POINT ( 'NONE',  ( 3.778760231354629433E-15, 0.5000000000000067724, -24.50000000000000355 ) ) ;
#20224 = CARTESIAN_POINT ( 'NONE',  ( 32.50000000000000000, 9.000000000000007105, -3.980102097228898626E-15 ) ) ;
#20225 = CARTESIAN_POINT ( 'NONE',  ( -4.405589869732278832E-13, 9.000000005462366559, 32.50000000000000000 ) ) ;
#20226 = CARTESIAN_POINT ( 'NONE',  ( -0.04044903255042732459, 48.80430583240936215, -27.95245687107223986 ) ) ;
#20227 = CARTESIAN_POINT ( 'NONE',  ( 33.58253175000000823, 58.02500000273117564, 10.91162601494192863 ) ) ;
#20228 = CARTESIAN_POINT ( 'NONE',  ( -2.162160676586881955E-15, 62.87500000273120548, -35.31076352940723240 ) ) ;
#20229 = CARTESIAN_POINT ( 'NONE',  ( -33.58253175000000113, 39.27500000273118275, -10.91162601494193041 ) ) ;
#20230 = CARTESIAN_POINT ( 'NONE',  ( 23.41746824999999887, 16.72499999726881725, -7.608796670333727974 ) ) ;
#20231 = CARTESIAN_POINT ( 'NONE',  ( 23.09401076758502569, 96.00000000000002842, -6.857326241137392698E-15 ) ) ;
#20232 = CARTESIAN_POINT ( 'NONE',  ( -20.08610463437156923, 6.300000000000004263, 27.64615127144130113 ) ) ;
#20233 = CARTESIAN_POINT ( 'NONE',  ( -27.95245687107223986, 43.94569416759065206, -0.04044903254993292840 ) ) ;
#20234 = CARTESIAN_POINT ( 'NONE',  ( -12.70562935223222034, 16.99999999999998934, -20.31534774774085150 ) ) ;
#20235 = CARTESIAN_POINT ( 'NONE',  ( -20.08610463437156923, 28.30000000000000782, 27.64615127144130113 ) ) ;
#20236 = CARTESIAN_POINT ( 'NONE',  ( 33.58253175000000823, 22.02500000273117919, 10.91162601494192863 ) ) ;
#20237 = CARTESIAN_POINT ( 'NONE',  ( 20.08610463437158344, 66.69999999999998863, 27.64615127144129403 ) ) ;
#20238 = CARTESIAN_POINT ( 'NONE',  ( -12.13525491562421088, 78.05000000546242234, -8.816778784387096835 ) ) ;
#20239 = CARTESIAN_POINT ( 'NONE',  ( 0.000000000000000000, 80.00000000000001421, 0.000000000000000000 ) ) ;
#20240 = CARTESIAN_POINT ( 'NONE',  ( -25.98046417659831420, 68.28347249907602645, 15.04653450569339945 ) ) ;
#20241 = CARTESIAN_POINT ( 'NONE',  ( 10.04305231718578817, 39.90000000546238823, -30.90933677959249337 ) ) ;
#20242 = CARTESIAN_POINT ( 'NONE',  ( 33.58253175000000823, 30.02500000273118985, 10.91162601494192685 ) ) ;
#20243 = CARTESIAN_POINT ( 'NONE',  ( 33.58253175000000113, 64.37500000273119838, -4.112674001490185761E-15 ) ) ;
#20244 = CARTESIAN_POINT ( 'NONE',  ( 13.97622843553633665, 34.48697916666667140, 24.20753774853730889 ) ) ;
#20245 = ORIENTED_EDGE ( 'NONE', *, *, #20115, .F. ) ;
#20246 = CARTESIAN_POINT ( 'NONE',  ( 33.58253175000000113, 70.22500000273120691, -10.91162601494193751 ) ) ;
#20247 = CARTESIAN_POINT ( 'NONE',  ( 30.02300923189239512, 37.35156249999997868, -2.619432448724977703E-13 ) ) ;
#20248 = CARTESIAN_POINT ( 'NONE',  ( -4.000000000000003553, 0.000000000000000000, 0.000000000000000000 ) ) ;
#20249 = ORIENTED_EDGE ( 'NONE', *, *, #4371, .F. ) ;
#20250 = CARTESIAN_POINT ( 'NONE',  ( 28.02196122052045268, 55.83371500092398065, -7.468012846824774620 ) ) ;
#20251 = CARTESIAN_POINT ( 'NONE',  ( -24.18731323226248264, 57.98215250092397355, -14.01125832528284931 ) ) ;
#20252 = CARTESIAN_POINT ( 'NONE',  ( 27.16883889988623935, 12.32500000273119234, -19.73931689729374384 ) ) ;
#20253 = CARTESIAN_POINT ( 'NONE',  ( -7.468012846824272799, 16.29128499907601579, 28.02196122052058413 ) ) ;
#20254 = LINE ( 'NONE', #30697, #32726 ) ;
#20255 = CARTESIAN_POINT ( 'NONE',  ( -27.16883889988624290, 39.17500000273118843, -19.73931689729374028 ) ) ;
#20256 = CARTESIAN_POINT ( 'NONE',  ( -2.092463501923844636E-15, 46.00000000546238965, -34.17252228774368916 ) ) ;
#20257 = CARTESIAN_POINT ( 'NONE',  ( -4.635254915624211769, 79.60000000000000853, -14.26584774442730286 ) ) ;
#20258 = CARTESIAN_POINT ( 'NONE',  ( 27.16883889988623935, 26.32500000273119056, -19.73931689729374384 ) ) ;
#20259 = CARTESIAN_POINT ( 'NONE',  ( 15.14183272437242067, 13.44999999453762385, 20.84094480462498211 ) ) ;
#20260 = CARTESIAN_POINT ( 'NONE',  ( 20.75514604977249178, 56.07500000273117990, 28.56700777964553950 ) ) ;
#20261 = CARTESIAN_POINT ( 'NONE',  ( 32.50000000000000711, 26.89999999999999147, 10.55989012756945122 ) ) ;
#20262 = CARTESIAN_POINT ( 'NONE',  ( -32.50000000000000000, 30.10000000000000853, 10.55989012756946366 ) ) ;
#20263 = CARTESIAN_POINT ( 'NONE',  ( -23.41746824999999887, 15.62499999726882294, -2.867812753649727150E-15 ) ) ;
#20264 = CARTESIAN_POINT ( 'NONE',  ( -20.75514604977248823, 76.82500000273120122, -28.56700777964554305 ) ) ;
#20265 = CARTESIAN_POINT ( 'NONE',  ( 5.204170427930421283E-15, -70.99969134886156041, 0.000000000000000000 ) ) ;
#20266 = CARTESIAN_POINT ( 'NONE',  ( 33.58253175000000823, 62.27500000273118985, 10.91162601494192685 ) ) ;
#20267 = CARTESIAN_POINT ( 'NONE',  ( -12.13525491562421088, 76.05000000546240813, -8.816778784387096835 ) ) ;
#20268 = DIRECTION ( 'NONE',  ( 0.000000000000000000, -0.000000000000000000, -1.000000000000000000 ) ) ;
#20269 = CARTESIAN_POINT ( 'NONE',  ( -27.16883889988623935, 19.32500000273118701, 19.73931689729374739 ) ) ;
#20270 = CARTESIAN_POINT ( 'NONE',  ( -15.14183272437242600, 13.04999999453763770, 20.84094480462497856 ) ) ;
#20271 = CARTESIAN_POINT ( 'NONE',  ( 6.950374756619721595, 22.31809000092397000, 26.09010956794232428 ) ) ;
#20272 = CARTESIAN_POINT ( 'NONE',  ( -15.00000000000000000, 74.25000000546239676, 0.000000000000000000 ) ) ;
#20273 = CARTESIAN_POINT ( 'NONE',  ( 10.37757302488624767, 39.72500000273119980, 31.93888565452638417 ) ) ;
#20274 = CARTESIAN_POINT ( 'NONE',  ( 20.75514604977248467, 4.675000002731191096, -28.56700777964554305 ) ) ;
#20275 = CARTESIAN_POINT ( 'NONE',  ( -2.162160676586882350E-15, 54.87500000273119838, -35.31076352940722529 ) ) ;
#20276 = CARTESIAN_POINT ( 'NONE',  ( -15.04653450569291984, 50.24777750092398065, 25.98046417659859486 ) ) ;
#20277 = CARTESIAN_POINT ( 'NONE',  ( 5.779280353836490358E-15, 3.000000005462374109, 32.49999999999999289 ) ) ;
#20278 = CARTESIAN_POINT ( 'NONE',  ( -0.04044903255044120238, 38.49180583240935505, -30.02300923189239867 ) ) ;
#20279 = CARTESIAN_POINT ( 'NONE',  ( 10.04305231718578817, 61.90000000546237402, -30.90933677959249337 ) ) ;
#20280 = CARTESIAN_POINT ( 'NONE',  ( 11.25946833292375793, 73.67500000273119554, 8.180482586598731842 ) ) ;
#20281 = CARTESIAN_POINT ( 'NONE',  ( 0.04044903255044120238, 67.71055583240935505, 27.95245687107223276 ) ) ;
#20282 = CARTESIAN_POINT ( 'NONE',  ( 24.50000000000000000, 0.000000000000000000, 0.000000000000000000 ) ) ;
#20283 = CARTESIAN_POINT ( 'NONE',  ( -10.04305231718579172, 76.10000000546237686, -30.90933677959248982 ) ) ;
#20284 = CARTESIAN_POINT ( 'NONE',  ( -1.137977401836464321E-14, 52.00000000000000711, 46.18802153517007270 ) ) ;
#20285 = EDGE_CURVE ( 'NONE', #15702, #14454, #14284, .T. ) ;
#20286 = CARTESIAN_POINT ( 'NONE',  ( 33.58253175000000823, 36.27500000273119696, 10.91162601494192863 ) ) ;
#20287 = CARTESIAN_POINT ( 'NONE',  ( 7.236395654485760609, 9.524999997268828622, -22.27133577429736633 ) ) ;
#20288 = ORIENTED_EDGE ( 'NONE', *, *, #18079, .F. ) ;
#20289 = CARTESIAN_POINT ( 'NONE',  ( 33.58253175000000823, 74.27500000273117564, 10.91162601494192863 ) ) ;
#20290 = CARTESIAN_POINT ( 'NONE',  ( -26.29305231718578995, 20.70000000546238894, 19.10302069950538595 ) ) ;
#20291 = CARTESIAN_POINT ( 'NONE',  ( -15.01150461594642138, 43.08072916666666430, -26.00068869287340334 ) ) ;
#20292 = CARTESIAN_POINT ( 'NONE',  ( 32.50000000000000000, 65.60000000546237686, -10.55989012756945833 ) ) ;
#20293 = ORIENTED_EDGE ( 'NONE', *, *, #2822, .T. ) ;
#20294 = DIRECTION ( 'NONE',  ( -1.000000000000000000, -1.416100796715761110E-16, 0.000000000000000000 ) ) ;
#20295 = CARTESIAN_POINT ( 'NONE',  ( 6.486482029760649416E-15, 49.62500000273117706, 35.31076352940723240 ) ) ;
#20296 = CARTESIAN_POINT ( 'NONE',  ( 18.94512977948575738, 16.42499999726882010, 13.76444248337723408 ) ) ;
#20297 = CARTESIAN_POINT ( 'NONE',  ( -26.29305231718578995, 4.700000005462390718, 19.10302069950538595 ) ) ;
#20298 = CARTESIAN_POINT ( 'NONE',  ( 0.000000000000000000, 0.000000000000000000, -32.50000000000000000 ) ) ;
#20299 = CARTESIAN_POINT ( 'NONE',  ( 2.740863092043355209E-13, 14.14843749999999467, 30.02300923189239867 ) ) ;
#20300 = CARTESIAN_POINT ( 'NONE',  ( -20.08610463437156923, 52.30000000000001137, 27.64615127144130113 ) ) ;
#20301 = CARTESIAN_POINT ( 'NONE',  ( -10.04305231718579172, 13.60000000000000142, -30.90933677959248982 ) ) ;
#20302 = CARTESIAN_POINT ( 'NONE',  ( -33.58253175000000113, 15.37500000273117706, 0.000000000000000000 ) ) ;
#20303 = CARTESIAN_POINT ( 'NONE',  ( 7.025853678916867295, 26.31732666574268364, 26.06988505166722803 ) ) ;
#20304 = CARTESIAN_POINT ( 'NONE',  ( -4.300734207923755825, 77.77500000273118985, 13.23629886949340673 ) ) ;
#20305 = CARTESIAN_POINT ( 'NONE',  ( 12.13525491562420910, 75.45000000546237118, -8.816778784387098611 ) ) ;
#20306 = CARTESIAN_POINT ( 'NONE',  ( -20.08610463437157989, 43.69999999999998863, -27.64615127144129758 ) ) ;
#20307 =( BOUNDED_CURVE ( )  B_SPLINE_CURVE ( 2, ( #3058, #29457, #3718, #24158, #8194, #24644, #11118, #13859, #11603, #8529, #21586, #22085, #18685 ),
 .UNSPECIFIED., .F., .T. ) 
 B_SPLINE_CURVE_WITH_KNOTS ( ( 3, 2, 2, 2, 2, 2, 3 ),
 ( 0.5277777777777777901, 0.5333333333333333259, 0.5444444444444443976, 0.5555555555555555802, 0.5666666666666666519, 0.5777777777777777235, 0.5833333333333333703 ),
 .UNSPECIFIED. ) 
 CURVE ( )  GEOMETRIC_REPRESENTATION_ITEM ( )  RATIONAL_B_SPLINE_CURVE ( ( 0.9755282581475768211, 0.9755282581475768211, 1.000000000000000000, 0.9510565162951535312, 1.000000000000000000, 0.9510565162951535312, 1.000000000000000000, 0.9510565162951535312, 1.000000000000000000, 0.9510565162951535312, 1.000000000000000000, 0.9755282581475765991, 0.9755282581475768211 ) ) 
 REPRESENTATION_ITEM ( '' )  );
#20308 = CARTESIAN_POINT ( 'NONE',  ( 10.04305231718578817, 5.400000000000002132, -30.90933677959249337 ) ) ;
#20309 = ORIENTED_EDGE ( 'NONE', *, *, #10417, .F. ) ;
#20310 = CARTESIAN_POINT ( 'NONE',  ( -7.236395654485763274, 12.52499999726880375, 22.27133577429736633 ) ) ;
#20311 = CARTESIAN_POINT ( 'NONE',  ( -7.236395654485757944, 3.224999997268801266, -22.27133577429736988 ) ) ;
#20312 = CARTESIAN_POINT ( 'NONE',  ( 6.988114217767829928, 46.94791666666666430, -26.07999730980489872 ) ) ;
#20313 =( BOUNDED_CURVE ( )  B_SPLINE_CURVE ( 2, ( #19458, #29563, #8476, #27344, #16717, #19622, #24928, #27171, #22362, #18963, #29407, #3334, #13805 ),
 .UNSPECIFIED., .F., .T. ) 
 B_SPLINE_CURVE_WITH_KNOTS ( ( 3, 2, 2, 2, 2, 2, 3 ),
 ( 0.6346153846153845812, 0.6358974358974358587, 0.6384615384615384137, 0.6410256410256410797, 0.6435897435897436347, 0.6461538461538461897, 0.6474358974358974672 ),
 .UNSPECIFIED. ) 
 CURVE ( )  GEOMETRIC_REPRESENTATION_ITEM ( )  RATIONAL_B_SPLINE_CURVE ( ( 0.9755282581475768211, 0.9755282581475768211, 1.000000000000000000, 0.9510565162951535312, 1.000000000000000000, 0.9510565162951535312, 1.000000000000000000, 0.9510565162951535312, 1.000000000000000000, 0.9510565162951535312, 1.000000000000000000, 0.9755282581475768211, 0.9755282581475768211 ) ) 
 REPRESENTATION_ITEM ( '' )  );
#20314 = CARTESIAN_POINT ( 'NONE',  ( 33.58253175000000823, 60.02500000273116854, 10.91162601494192863 ) ) ;
#20315 = CARTESIAN_POINT ( 'NONE',  ( 27.16883889988624290, 26.17500000273119554, 19.73931689729373673 ) ) ;
#20316 = CARTESIAN_POINT ( 'NONE',  ( 20.75514604977249178, 10.07500000273119234, 28.56700777964553950 ) ) ;
#20317 = CARTESIAN_POINT ( 'NONE',  ( 24.20753774853731244, 30.19010416666665719, -13.97622843553633132 ) ) ;
#20318 = CARTESIAN_POINT ( 'NONE',  ( -27.16883889988624290, 5.175000002731189319, -19.73931689729374028 ) ) ;
#20319 = CARTESIAN_POINT ( 'NONE',  ( 28.00173670424549499, 25.18267333425730214, 7.543491769121417612 ) ) ;
#20320 = CARTESIAN_POINT ( 'NONE',  ( -7.505752307973343918, 60.41145833333332149, -28.01184896238290989 ) ) ;
#20321 = CARTESIAN_POINT ( 'NONE',  ( -2.092463501923844636E-15, 78.00000000546238255, -34.17252228774368916 ) ) ;
#20322 = CARTESIAN_POINT ( 'NONE',  ( 20.08610463437157279, 3.299999999999982947, -27.64615127144129758 ) ) ;
#20323 = CARTESIAN_POINT ( 'NONE',  ( -26.29305231718579350, 39.79999999999999005, -19.10302069950537884 ) ) ;
#20324 = CARTESIAN_POINT ( 'NONE',  ( 27.16883889988623935, 42.32500000273120833, -19.73931689729374384 ) ) ;
#20325 = CARTESIAN_POINT ( 'NONE',  ( 18.94512977948576093, 10.82499999726882578, -13.76444248337722875 ) ) ;
#20326 = DIRECTION ( 'NONE',  ( 0.000000000000000000, -1.000000000000000000, 0.000000000000000000 ) ) ;
#20327 = ORIENTED_EDGE ( 'NONE', *, *, #14116, .T. ) ;
#20328 = CARTESIAN_POINT ( 'NONE',  ( 10.37757302488624767, 53.97500000273118559, 31.93888565452638417 ) ) ;
#20329 = FACE_OUTER_BOUND ( 'NONE', #1950, .T. ) ;
#20330 = CARTESIAN_POINT ( 'NONE',  ( -19.06425588902591173, 34.06288166759063785, -19.11951029504763611 ) ) ;
#20331 = CARTESIAN_POINT ( 'NONE',  ( 20.75514604977248467, 78.67500000273116711, -28.56700777964554305 ) ) ;
#20332 = ORIENTED_EDGE ( 'NONE', *, *, #30392, .T. ) ;
#20333 = CARTESIAN_POINT ( 'NONE',  ( -33.58253175000000113, 29.22500000273118914, 10.91162601494193929 ) ) ;
#20334 = CARTESIAN_POINT ( 'NONE',  ( -20.50609665441004736, 15.43749999999999645, -20.50609665440969565 ) ) ;
#20335 = VERTEX_POINT ( 'NONE', #33655 ) ;
#20336 = CARTESIAN_POINT ( 'NONE',  ( 0.000000000000000000, 0.000000000000000000, 0.000000000000000000 ) ) ;
#20337 = CARTESIAN_POINT ( 'NONE',  ( 10.37757302488624767, 65.72500000273117848, 31.93888565452638417 ) ) ;
#20338 = CARTESIAN_POINT ( 'NONE',  ( -2.584737979205441561E-13, 36.49218750000000000, -30.02300923189239512 ) ) ;
#20339 = CARTESIAN_POINT ( 'NONE',  ( -4.732186688966233175E-15, 13.50000000000001066, 25.76082449383753925 ) ) ;
#20340 = CARTESIAN_POINT ( 'NONE',  ( -23.41746825000000243, 4.224999997268803931, 7.608796670333725309 ) ) ;
#20341 = CARTESIAN_POINT ( 'NONE',  ( -10.37757302488624411, 10.72500000273118914, -31.93888565452638417 ) ) ;
#20342 = DIRECTION ( 'NONE',  ( -1.224646799147353454E-16, 1.000000000000000000, -0.000000000000000000 ) ) ;
#20343 = CARTESIAN_POINT ( 'NONE',  ( 7.468012846824281681, 48.94753499907601935, -28.02196122052058058 ) ) ;
#20344 = CARTESIAN_POINT ( 'NONE',  ( -4.635254915624208216, 74.40000000000001990, 14.26584774442730463 ) ) ;
#20345 = CARTESIAN_POINT ( 'NONE',  ( 20.50609665441005092, 65.28125000000000000, 20.50609665440969209 ) ) ;
#20346 = CARTESIAN_POINT ( 'NONE',  ( -3.880418787951142701, 15.19874571299077282, 24.49999999999999645 ) ) ;
#20347 = CARTESIAN_POINT ( 'NONE',  ( 32.50000000000000711, 61.40000000546236691, 10.55989012756945122 ) ) ;
#20348 = CARTESIAN_POINT ( 'NONE',  ( -7.570916362186215665, 11.14999999453761248, 23.30088464923126423 ) ) ;
#20349 = CARTESIAN_POINT ( 'NONE',  ( 15.00000000000000000, 79.35000000546239107, -4.873795443493596835 ) ) ;
#20350 = CARTESIAN_POINT ( 'NONE',  ( -26.07999730980477437, 25.17708333333332860, 6.988114217768305103 ) ) ;
#20351 = EDGE_CURVE ( 'NONE', #20335, #33960, #6156, .T. ) ;
#20352 = CARTESIAN_POINT ( 'NONE',  ( -33.58253175000000113, 31.12500000273119127, 0.000000000000000000 ) ) ;
#20353 = CARTESIAN_POINT ( 'NONE',  ( 9.270509831248421762, 75.30000000000001137, -12.75976212528059861 ) ) ;
#20354 = AXIS2_PLACEMENT_3D ( 'NONE', #26546, #27674, #29604 ) ;
#20355 = CONICAL_SURFACE ( 'NONE', #24201, 12.11000150615021909, 0.2617993877991545149 ) ;
#20356 = CARTESIAN_POINT ( 'NONE',  ( -20.75514604977248112, 45.67500000273119554, 28.56700777964554661 ) ) ;
#20357 = CARTESIAN_POINT ( 'NONE',  ( -33.58253175000000113, 23.47500000273119269, 10.91162601494193929 ) ) ;
#20358 = ADVANCED_FACE ( 'NONE', ( #33828 ), #10788, .F. ) ;
#20359 = CARTESIAN_POINT ( 'NONE',  ( 33.58253175000000113, 78.22500000273117848, -10.91162601494193574 ) ) ;
#20360 = CARTESIAN_POINT ( 'NONE',  ( -10.04305231718578462, 26.90000000546238823, 30.90933677959249337 ) ) ;
#20361 = CARTESIAN_POINT ( 'NONE',  ( -10.04305231718578462, 62.39999999999999858, 30.90933677959249337 ) ) ;
#20362 = CARTESIAN_POINT ( 'NONE',  ( 23.41746824999999887, 18.62499999726882649, 0.000000000000000000 ) ) ;
#20363 = CARTESIAN_POINT ( 'NONE',  ( -10.37757302488623701, 67.52500000273120406, 31.93888565452638417 ) ) ;
#20364 = CARTESIAN_POINT ( 'NONE',  ( -23.41746824999999887, 2.124999997268811391, -2.867812753649727150E-15 ) ) ;
#20365 = CARTESIAN_POINT ( 'NONE',  ( -13.94119854578892514, 43.93451416574269075, 24.22776226481266448 ) ) ;
#20366 = CARTESIAN_POINT ( 'NONE',  ( -10.37757302488623701, 77.77500000273117564, 31.93888565452638417 ) ) ;
#20367 = CARTESIAN_POINT ( 'NONE',  ( 33.58253175000000823, 4.025000002731196957, 10.91162601494192685 ) ) ;
#20368 = CARTESIAN_POINT ( 'NONE',  ( 23.41746824999999887, 13.12499999726882116, 0.000000000000000000 ) ) ;
#20369 = CARTESIAN_POINT ( 'NONE',  ( -24.20753774853730889, 66.28385416666662877, 13.97622843553633842 ) ) ;
#20370 = ORIENTED_EDGE ( 'NONE', *, *, #25524, .T. ) ;
#20371 = CARTESIAN_POINT ( 'NONE',  ( 33.58253175000000823, 48.02500000273119696, 10.91162601494192863 ) ) ;
#20372 = CARTESIAN_POINT ( 'NONE',  ( 27.16883889988623935, 20.57500000273120122, -19.73931689729374384 ) ) ;
#20373 = ORIENTED_EDGE ( 'NONE', *, *, #12596, .T. ) ;
#20374 = CARTESIAN_POINT ( 'NONE',  ( 20.50609665441005092, 34.34374999999999289, 20.50609665440969209 ) ) ;
#20375 = CARTESIAN_POINT ( 'NONE',  ( 25.98046417659858420, 32.20090250092397355, 15.04653450569292872 ) ) ;
#20376 = CARTESIAN_POINT ( 'NONE',  ( -1.778240108872766143E-15, 62.00000000546238255, -32.49999999999999289 ) ) ;
#20377 = DIRECTION ( 'NONE',  ( -0.000000000000000000, -1.000000000000000000, -0.000000000000000000 ) ) ;
#20378 = CARTESIAN_POINT ( 'NONE',  ( -14.47279130897151589, 3.824999997268816454, -19.92008829642072598 ) ) ;
#20379 = CARTESIAN_POINT ( 'NONE',  ( 14.47279130897151589, 14.32499999726880624, 19.92008829642072953 ) ) ;
#20380 = CARTESIAN_POINT ( 'NONE',  ( -10.37757302488624411, 16.97500000273119269, -31.93888565452638417 ) ) ;
#20381 = CARTESIAN_POINT ( 'NONE',  ( 10.04305231718578817, 23.90000000546238468, -30.90933677959249337 ) ) ;
#20382 = CARTESIAN_POINT ( 'NONE',  ( -32.50000000000000000, 67.89999999999996305, -10.55989012756945478 ) ) ;
#20383 = FACE_BOUND ( 'NONE', #16348, .T. ) ;
#20384 = DIRECTION ( 'NONE',  ( -1.000000000000000000, 0.000000000000000000, 0.000000000000000000 ) ) ;
#20385 = CARTESIAN_POINT ( 'NONE',  ( -15.01150461594642138, 15.58072916666666607, -26.00068869287340334 ) ) ;
#20386 = CARTESIAN_POINT ( 'NONE',  ( 20.75514604977248467, 32.67500000273118843, -28.56700777964554305 ) ) ;
#20387 = CARTESIAN_POINT ( 'NONE',  ( -2.165007332552593587E-13, 45.00000000546237544, 32.50000000000000000 ) ) ;
#20388 = CARTESIAN_POINT ( 'NONE',  ( -20.50609665441004736, 36.06250000000000000, -20.50609665440969565 ) ) ;
#20389 = DIRECTION ( 'NONE',  ( 1.000000000000000000, 0.000000000000000000, 0.000000000000000000 ) ) ;
#20390 = CARTESIAN_POINT ( 'NONE',  ( -18.94512977948575738, 13.92499999726881654, -13.76444248337723231 ) ) ;
#20391 = CARTESIAN_POINT ( 'NONE',  ( 20.08610463437158344, 10.70000000000001172, 27.64615127144129403 ) ) ;
#20392 = CARTESIAN_POINT ( 'NONE',  ( -15.14183272437242600, 15.30000000000001137, 20.84094480462497856 ) ) ;
#20393 = EDGE_CURVE ( 'NONE', #17459, #32333, #28353, .T. ) ;
#20394 = CARTESIAN_POINT ( 'NONE',  ( -19.11951029504797006, 55.24961833240936926, -19.06425588902558133 ) ) ;
#20395 = CARTESIAN_POINT ( 'NONE',  ( -2.162160676586881955E-15, 50.62500000273118417, -35.31076352940723240 ) ) ;
#20396 = CARTESIAN_POINT ( 'NONE',  ( 20.75514604977248467, 62.67500000273117422, -28.56700777964554305 ) ) ;
#20397 = CARTESIAN_POINT ( 'NONE',  ( -27.16883889988624290, 39.17500000273118843, -19.73931689729374028 ) ) ;
#20398 = CARTESIAN_POINT ( 'NONE',  ( 23.41746824999999887, 14.72499999726882081, -7.608796670333727974 ) ) ;
#20399 = CARTESIAN_POINT ( 'NONE',  ( 6.988114217768294445, 14.00520833333333215, 26.07999730980477437 ) ) ;
#20400 = CARTESIAN_POINT ( 'NONE',  ( -22.54140686924021963, 16.99999999999999645, -9.059062350126763974 ) ) ;
#20401 = CARTESIAN_POINT ( 'NONE',  ( -10.04305231718579172, 27.60000000000001208, -30.90933677959248982 ) ) ;
#20402 = CARTESIAN_POINT ( 'NONE',  ( 27.16883889988624290, 19.92500000273118843, 19.73931689729373673 ) ) ;
#20403 = DIRECTION ( 'NONE',  ( 0.000000000000000000, -1.000000000000000000, 0.000000000000000000 ) ) ;
#20404 = CARTESIAN_POINT ( 'NONE',  ( 26.29305231718579350, 52.79999999999999716, 19.10302069950537529 ) ) ;
#20405 = LINE ( 'NONE', #7177, #11111 ) ;
#20406 = CARTESIAN_POINT ( 'NONE',  ( 15.04653450569339945, 67.42409749907601224, 25.98046417659831775 ) ) ;
#20407 = CARTESIAN_POINT ( 'NONE',  ( 32.50000000000000711, 43.40000000546238113, 10.55989012756945122 ) ) ;
#20408 =( BOUNDED_CURVE ( )  B_SPLINE_CURVE ( 2, ( #20101, #12711, #6873, #28157, #4643, #25064, #22490, #30203, #25586, #6704, #12193, #32941, #9440 ),
 .UNSPECIFIED., .F., .F. ) 
 B_SPLINE_CURVE_WITH_KNOTS ( ( 3, 2, 2, 2, 2, 2, 3 ),
 ( 0.3055555555555555802, 0.3111111111111111160, 0.3222222222222222432, 0.3333333333333333148, 0.3444444444444444420, 0.3555555555555555691, 0.3611111111111111049 ),
 .UNSPECIFIED. ) 
 CURVE ( )  GEOMETRIC_REPRESENTATION_ITEM ( )  RATIONAL_B_SPLINE_CURVE ( ( 0.9755282581475767101, 0.9755282581475768211, 1.000000000000000000, 0.9510565162951535312, 1.000000000000000000, 0.9510565162951535312, 1.000000000000000000, 0.9510565162951535312, 1.000000000000000000, 0.9510565162951535312, 1.000000000000000000, 0.9755282581475768211, 0.9755282581475768211 ) ) 
 REPRESENTATION_ITEM ( '' )  );
#20409 = CARTESIAN_POINT ( 'NONE',  ( 5.779280353836490358E-15, 61.00000000546238255, 32.49999999999999289 ) ) ;
#20410 = CARTESIAN_POINT ( 'NONE',  ( -20.75514604977248112, 25.42500000273119198, 28.56700777964554661 ) ) ;
#20411 = CARTESIAN_POINT ( 'NONE',  ( 13.97622843553589966, 33.34114583333332860, -24.20753774853756113 ) ) ;
#20412 = ORIENTED_EDGE ( 'NONE', *, *, #7128, .T. ) ;
#20413 = CARTESIAN_POINT ( 'NONE',  ( -20.75514604977248112, 69.42500000273116711, 28.56700777964554661 ) ) ;
#20414 = CARTESIAN_POINT ( 'NONE',  ( -28.01184896238290278, 42.36458333333332860, 7.505752307973363457 ) ) ;
#20415 = CARTESIAN_POINT ( 'NONE',  ( -10.04305231718579172, 16.10000000546238397, -30.90933677959248982 ) ) ;
#20416 = ORIENTED_EDGE ( 'NONE', *, *, #10557, .T. ) ;
#20417 = CARTESIAN_POINT ( 'NONE',  ( 30.02300923189239867, 62.85194416759064495, 0.04044903254992252006 ) ) ;
#20418 = CARTESIAN_POINT ( 'NONE',  ( -6.950374756619716266, 61.84934000092397355, -26.09010956794232428 ) ) ;
#20419 = AXIS2_PLACEMENT_3D ( 'NONE', #8655, #26852, #29577 ) ;
#20420 = EDGE_LOOP ( 'NONE', ( #13585, #6721, #22222, #28211 ) ) ;
#20421 = CARTESIAN_POINT ( 'NONE',  ( 20.75514604977249178, 9.825000002731188786, 28.56700777964553950 ) ) ;
#20422 = CARTESIAN_POINT ( 'NONE',  ( -26.00068869287340334, 66.28385416666662877, 15.01150461594643382 ) ) ;
#20423 = FACE_OUTER_BOUND ( 'NONE', #19770, .T. ) ;
#20424 = CARTESIAN_POINT ( 'NONE',  ( 10.37757302488624767, 37.97500000273118559, 31.93888565452638417 ) ) ;
#20425 = CARTESIAN_POINT ( 'NONE',  ( 6.277390505771533514E-15, 41.00000000546236123, 34.17252228774368916 ) ) ;
#20426 = CARTESIAN_POINT ( 'NONE',  ( -12.13525491562421088, 77.80000000000003979, -8.816778784387096835 ) ) ;
#20427 = CARTESIAN_POINT ( 'NONE',  ( 33.58253175000000113, 24.12500000273118417, -4.112674001490185761E-15 ) ) ;
#20428 = CARTESIAN_POINT ( 'NONE',  ( 26.29305231718578995, 31.70000000546238539, -19.10302069950538240 ) ) ;
#20429 = CARTESIAN_POINT ( 'NONE',  ( 10.37757302488624056, 46.77500000273118985, -31.93888565452638417 ) ) ;
#20430 =( NAMED_UNIT ( * ) SI_UNIT ( $, .STERADIAN. ) SOLID_ANGLE_UNIT ( ) );
#20431 = CARTESIAN_POINT ( 'NONE',  ( 20.08610463437158344, 28.69999999999999574, 27.64615127144129403 ) ) ;
#20432 = CARTESIAN_POINT ( 'NONE',  ( -32.50000000000000000, 25.99999999999999645, 0.000000000000000000 ) ) ;
#20433 = CARTESIAN_POINT ( 'NONE',  ( 19.82091636218621389, 0.2000000000000057288, -14.40073868116559197 ) ) ;
#20434 = CARTESIAN_POINT ( 'NONE',  ( 6.486482029760649416E-15, 73.62500000273118417, 35.31076352940723240 ) ) ;
#20435 = CARTESIAN_POINT ( 'NONE',  ( -1.353501352685664516, 67.00000000000001421, 32.52334280248232545 ) ) ;
#20436 = CARTESIAN_POINT ( 'NONE',  ( -7.570916362186215665, 15.39999999999999680, 23.30088464923126423 ) ) ;
#20437 = CARTESIAN_POINT ( 'NONE',  ( 33.58253175000000113, 58.37500000273118417, -4.112674001490185761E-15 ) ) ;
#20438 = CARTESIAN_POINT ( 'NONE',  ( -12.13525491562421088, 74.05000000546240813, -8.816778784387096835 ) ) ;
#20439 = CARTESIAN_POINT ( 'NONE',  ( -5.147494310547423346, 40.94874572391552903, 32.50000000000000000 ) ) ;
#20440 = CARTESIAN_POINT ( 'NONE',  ( -10.37757302488624411, 20.72500000273119625, -31.93888565452638417 ) ) ;
#20441 = CARTESIAN_POINT ( 'NONE',  ( -15.14183272437241889, 8.449999994537634507, -20.84094480462497856 ) ) ;
#20442 = CARTESIAN_POINT ( 'NONE',  ( 24.22776226481241224, 24.75298583425730925, -13.94119854578936923 ) ) ;
#20443 = LINE ( 'NONE', #1715, #5307 ) ;
#20444 = VECTOR ( 'NONE', #9751, 1000.000000000000000 ) ;
#20445 = CARTESIAN_POINT ( 'NONE',  ( 10.37757302488624056, 40.52500000273119696, -31.93888565452638417 ) ) ;
#20446 = CARTESIAN_POINT ( 'NONE',  ( 0.000000000000000000, 52.00000000000000711, 0.000000000000000000 ) ) ;
#20447 = CARTESIAN_POINT ( 'NONE',  ( 27.16883889988624290, 56.17500000273119554, 19.73931689729373673 ) ) ;
#20448 = CARTESIAN_POINT ( 'NONE',  ( -28.02196122052045268, 43.80246500092398776, 7.468012846824790607 ) ) ;
#20449 = CARTESIAN_POINT ( 'NONE',  ( 7.313012447739250820E-14, 15.50000000000000178, 24.50000000000000000 ) ) ;
#20450 = CARTESIAN_POINT ( 'NONE',  ( -7.543491769121917656, 34.91107666574267654, -28.00173670424536354 ) ) ;
#20451 = CARTESIAN_POINT ( 'NONE',  ( 32.50000000000000711, 63.40000000546236691, 10.55989012756945122 ) ) ;
#20452 = CARTESIAN_POINT ( 'NONE',  ( 8.601468415847520532, 75.57500000273117280, 11.83890561707634781 ) ) ;
#20453 = CARTESIAN_POINT ( 'NONE',  ( 5.147494310547434893, 62.55125428154684641, 32.49999999999999289 ) ) ;
#20454 = CARTESIAN_POINT ( 'NONE',  ( 27.95245687107223276, 66.85118083240935505, -0.04044903255042905932 ) ) ;
#20455 = CARTESIAN_POINT ( 'NONE',  ( -18.94512977948576093, 2.324999997268817342, 13.76444248337722698 ) ) ;
#20456 = CARTESIAN_POINT ( 'NONE',  ( -26.29305231718578995, 72.70000000546239960, 19.10302069950538595 ) ) ;
#20457 = CARTESIAN_POINT ( 'NONE',  ( 12.13525491562420910, 79.19999999999998863, -8.816778784387098611 ) ) ;
#20458 = CARTESIAN_POINT ( 'NONE',  ( 27.16883889988623935, 34.57500000273118701, -19.73931689729374384 ) ) ;
#20459 = CARTESIAN_POINT ( 'NONE',  ( -14.47279130897151767, 7.824999997268806240, -19.92008829642072598 ) ) ;
#20460 = ORIENTED_EDGE ( 'NONE', *, *, #24249, .F. ) ;
#20461 = CARTESIAN_POINT ( 'NONE',  ( 20.75514604977248467, 76.67500000273116711, -28.56700777964554305 ) ) ;
#20462 = CARTESIAN_POINT ( 'NONE',  ( 20.08610463437157279, 21.80000000546236549, -27.64615127144129758 ) ) ;
#20463 = CARTESIAN_POINT ( 'NONE',  ( 7.505752307973351023, 41.50520833333333570, 28.01184896238290278 ) ) ;
#20464 = CARTESIAN_POINT ( 'NONE',  ( -33.58253175000000113, 57.37500000273118417, 0.000000000000000000 ) ) ;
#20465 = CARTESIAN_POINT ( 'NONE',  ( 6.277390505771533514E-15, 61.00000000546237544, 34.17252228774368916 ) ) ;
#20466 = ORIENTED_EDGE ( 'NONE', *, *, #32022, .T. ) ;
#20467 = CARTESIAN_POINT ( 'NONE',  ( -1.756012107511856980E-14, 6.249999994537623671, -24.50000000000000000 ) ) ;
#20468 = CARTESIAN_POINT ( 'NONE',  ( 27.16883889988623935, 44.32500000273117990, -19.73931689729374384 ) ) ;
#20469 = CARTESIAN_POINT ( 'NONE',  ( -23.41746824999999887, 15.62499999726882294, -2.867812753649727150E-15 ) ) ;
#20470 = CARTESIAN_POINT ( 'NONE',  ( -27.16883889988624290, 67.17500000273119554, -19.73931689729374028 ) ) ;
#20471 = CARTESIAN_POINT ( 'NONE',  ( 32.50000000000000000, 3.600000005462360431, -10.55989012756945833 ) ) ;
#20472 = CIRCLE ( 'NONE', #5672, 10.18398033115917656 ) ;
#20473 = CARTESIAN_POINT ( 'NONE',  ( -27.16883889988623935, 63.32500000273120833, 19.73931689729374739 ) ) ;
#20474 = CARTESIAN_POINT ( 'NONE',  ( 23.41746824999999887, 19.02499999726880375, 7.608796670333735079 ) ) ;
#20475 = CARTESIAN_POINT ( 'NONE',  ( 10.04305231718578817, 49.39999999999999858, -30.90933677959249337 ) ) ;
#20476 = CARTESIAN_POINT ( 'NONE',  ( 0.000000000000000000, 80.00000000000001421, 0.000000000000000000 ) ) ;
#20477 = CARTESIAN_POINT ( 'NONE',  ( 33.58253175000000113, 18.47500000273117848, -10.91162601494193751 ) ) ;
#20478 = CARTESIAN_POINT ( 'NONE',  ( 5.334720326618300005E-14, 73.50000000000001421, -32.50000000000000000 ) ) ;
#20479 = CARTESIAN_POINT ( 'NONE',  ( -19.11951029504797006, 27.74961833240935505, -19.06425588902558133 ) ) ;
#20480 = CARTESIAN_POINT ( 'NONE',  ( 8.601468415847516980, 80.67500000273116711, -11.83890561707634781 ) ) ;
#20481 = CARTESIAN_POINT ( 'NONE',  ( 27.16883889988623935, 78.57500000273121543, -19.73931689729374384 ) ) ;
#20482 = CARTESIAN_POINT ( 'NONE',  ( 5.147494310547434893, 53.05125428700922185, 32.49999999999999289 ) ) ;
#20483 = CARTESIAN_POINT ( 'NONE',  ( 27.16883889988623935, 76.57500000273120122, -19.73931689729374384 ) ) ;
#20484 = ORIENTED_EDGE ( 'NONE', *, *, #20914, .T. ) ;
#20485 = CARTESIAN_POINT ( 'NONE',  ( -4.523095164977116484E-15, 12.62499999726879985, 24.62258325217400312 ) ) ;
#20486 = CARTESIAN_POINT ( 'NONE',  ( -23.41746824999999887, 3.524999997268825958, -7.608796670333730638 ) ) ;
#20487 = CARTESIAN_POINT ( 'NONE',  ( -2.428612866367529427E-13, 53.67968750000000000, -27.95245687107222921 ) ) ;
#20488 = CARTESIAN_POINT ( 'NONE',  ( 27.16883889988624290, 59.92500000273119554, 19.73931689729373673 ) ) ;
#20489 = CARTESIAN_POINT ( 'NONE',  ( 20.75514604977248467, 20.67500000273119909, -28.56700777964554305 ) ) ;
#20490 = CARTESIAN_POINT ( 'NONE',  ( 33.58253175000000823, 8.275000002731191628, 10.91162601494192863 ) ) ;
#20491 = CARTESIAN_POINT ( 'NONE',  ( -19.09188309203694445, 29.18749999999999645, -19.09188309203661049 ) ) ;
#20492 = UNCERTAINTY_MEASURE_WITH_UNIT (LENGTH_MEASURE( 1.000000000000000082E-05 ), #30879, 'distance_accuracy_value', 'NONE');
#20493 = CARTESIAN_POINT ( 'NONE',  ( 30.02300923189239867, 21.60194416759064495, 0.04044903254992252006 ) ) ;
#20494 = ADVANCED_FACE ( 'NONE', ( #4157 ), #4839, .T. ) ;
#20495 = CARTESIAN_POINT ( 'NONE',  ( -7.543491769121917656, 14.28607666574268720, -28.00173670424536354 ) ) ;
#20496 = CARTESIAN_POINT ( 'NONE',  ( -33.58253175000000113, 3.225000002731179372, 10.91162601494193929 ) ) ;
#20497 = CARTESIAN_POINT ( 'NONE',  ( -13.91746824999999887, 73.37500000273119838, 0.000000000000000000 ) ) ;
#20498 = CARTESIAN_POINT ( 'NONE',  ( 32.50000000000000000, 43.00000000000000000, -3.980102097228898626E-15 ) ) ;
#20499 = CARTESIAN_POINT ( 'NONE',  ( 33.58253175000000113, 46.22500000273119980, -10.91162601494193574 ) ) ;
#20500 = CIRCLE ( 'NONE', #22659, 33.00000000000000000 ) ;
#20501 = CARTESIAN_POINT ( 'NONE',  ( 14.47279130897151767, 10.92499999726882365, -19.92008829642072598 ) ) ;
#20502 = EDGE_CURVE ( 'NONE', #16901, #22348, #11868, .T. ) ;
#20503 = EDGE_CURVE ( 'NONE', #26581, #10540, #4866, .T. ) ;
#20504 = CARTESIAN_POINT ( 'NONE',  ( 5.779280353836490358E-15, 61.00000000546238255, 32.49999999999999289 ) ) ;
#20505 = VERTEX_POINT ( 'NONE', #23718 ) ;
#20506 = CARTESIAN_POINT ( 'NONE',  ( -10.37757302488623701, 51.77500000273120406, 31.93888565452638417 ) ) ;
#20507 = CARTESIAN_POINT ( 'NONE',  ( 2.489536152421872915E-14, 75.50000000000000000, -32.49999999999999289 ) ) ;
#20508 = CARTESIAN_POINT ( 'NONE',  ( 27.95245687107223986, 45.66444416759065916, 0.04044903254993640479 ) ) ;
#20509 = CARTESIAN_POINT ( 'NONE',  ( 20.75514604977249178, 74.07500000273120122, 28.56700777964553950 ) ) ;
#20510 = ORIENTED_EDGE ( 'NONE', *, *, #4410, .F. ) ;
#20511 = CARTESIAN_POINT ( 'NONE',  ( 33.58253175000000113, 24.12500000273119838, -4.112674001490185761E-15 ) ) ;
#20512 = CARTESIAN_POINT ( 'NONE',  ( 20.50609665440969565, 16.29687499999999645, -20.50609665441004736 ) ) ;
#20513 = ORIENTED_EDGE ( 'NONE', *, *, #16923, .T. ) ;
#20514 = DIRECTION ( 'NONE',  ( -1.224646799147353454E-16, 1.000000000000000000, -0.000000000000000000 ) ) ;
#20515 = B_SPLINE_CURVE_WITH_KNOTS ( 'NONE', 3,
 ( #1656, #30144, #3909, #25530, #6648, #2007, #12483, #25008, #22952, #9907 ),
 .UNSPECIFIED., .F., .F.,
 ( 4, 2, 2, 2, 4 ),
 ( 0.000000000000000000, 0.006590582801587962884, 0.01318116560317592577, 0.01977174840476388779, 0.02636233120635185154 ),
 .UNSPECIFIED. ) ;
#20516 = CARTESIAN_POINT ( 'NONE',  ( 33.58253175000000823, 60.02500000273116854, 10.91162601494192863 ) ) ;
#20517 = CARTESIAN_POINT ( 'NONE',  ( 20.50609665440969565, 36.92187499999999289, -20.50609665441004736 ) ) ;
#20518 =( BOUNDED_CURVE ( )  B_SPLINE_CURVE ( 2, ( #32365, #797, #31864, #16439, #27056, #13529, #8859 ),
 .UNSPECIFIED., .F., .F. ) 
 B_SPLINE_CURVE_WITH_KNOTS ( ( 3, 2, 2, 3 ),
 ( 0.000000000000000000, 0.02000000000000000042, 0.04000000000000000083, 0.05000000000000000971 ),
 .UNSPECIFIED. ) 
 CURVE ( )  GEOMETRIC_REPRESENTATION_ITEM ( )  RATIONAL_B_SPLINE_CURVE ( ( 1.000000000000000000, 0.9510565162951535312, 1.000000000000000000, 0.9510565162951535312, 1.000000000000000000, 0.9755282581475768211, 0.9755282581475768211 ) ) 
 REPRESENTATION_ITEM ( '' )  );
#20519 = CARTESIAN_POINT ( 'NONE',  ( -19.82091636218621389, 13.19999999999998863, 14.40073868116558842 ) ) ;
#20520 = CARTESIAN_POINT ( 'NONE',  ( 3.980102097228898626E-15, 80.00000000000001421, 32.50000000000000000 ) ) ;
#20521 = CARTESIAN_POINT ( 'NONE',  ( -27.16883889988624290, 8.925000002731191984, -19.73931689729374028 ) ) ;
#20522 =( BOUNDED_CURVE ( )  B_SPLINE_CURVE ( 2, ( #14857, #31152, #15204, #20353, #22923, #23441, #17780, #30627, #28408, #23270, #15379, #33379, #10230 ),
 .UNSPECIFIED., .F., .T. ) 
 B_SPLINE_CURVE_WITH_KNOTS ( ( 3, 2, 2, 2, 2, 2, 3 ),
 ( 0.6500000000000000222, 0.6600000000000000311, 0.6800000000000000488, 0.6999999999999999556, 0.7199999999999999734, 0.7399999999999999911, 0.7500000000000000000 ),
 .UNSPECIFIED. ) 
 CURVE ( )  GEOMETRIC_REPRESENTATION_ITEM ( )  RATIONAL_B_SPLINE_CURVE ( ( 0.9755282581475768211, 0.9755282581475768211, 1.000000000000000000, 0.9510565162951535312, 1.000000000000000000, 0.9510565162951535312, 1.000000000000000000, 0.9510565162951535312, 1.000000000000000000, 0.9510565162951535312, 1.000000000000000000, 0.9755282581475768211, 0.9755282581475768211 ) ) 
 REPRESENTATION_ITEM ( '' )  );
#20523 = CARTESIAN_POINT ( 'NONE',  ( 32.50000000000000000, 29.10000000000001208, -10.55989012756945833 ) ) ;
#20524 = CARTESIAN_POINT ( 'NONE',  ( -25.98046417659831420, 51.09597249907602645, 15.04653450569339945 ) ) ;
#20525 = CARTESIAN_POINT ( 'NONE',  ( 2.897257156509938333E-15, 72.50000000000001421, 15.77193336357400710 ) ) ;
#20526 = VECTOR ( 'NONE', #32894, 1000.000000000000000 ) ;
#20527 = CARTESIAN_POINT ( 'NONE',  ( 26.00068869287341045, 64.56510416666667140, -15.01150461594642493 ) ) ;
#20528 = CARTESIAN_POINT ( 'NONE',  ( 5.147494310547434893, 54.55125428154683220, 32.49999999999999289 ) ) ;
#20529 = CARTESIAN_POINT ( 'NONE',  ( 26.29305231718579350, 14.79999999999999361, 19.10302069950537529 ) ) ;
#20530 = CARTESIAN_POINT ( 'NONE',  ( -19.82091636218621389, 12.94999999453763628, 14.40073868116558842 ) ) ;
#20531 = CARTESIAN_POINT ( 'NONE',  ( 2.897257156509938333E-15, 70.75000000546236834, 15.77193336357400710 ) ) ;
#20532 = CARTESIAN_POINT ( 'NONE',  ( 6.988114217767829928, 26.32291666666666075, -26.07999730980489872 ) ) ;
#20533 = CARTESIAN_POINT ( 'NONE',  ( 27.16883889988624290, 29.92500000273118488, 19.73931689729373673 ) ) ;
#20534 = CARTESIAN_POINT ( 'NONE',  ( -33.58253175000000113, 77.22500000273117848, 10.91162601494193929 ) ) ;
#20535 = CARTESIAN_POINT ( 'NONE',  ( -27.16883889988623935, 41.57500000273119412, 19.73931689729374739 ) ) ;
#20536 = CARTESIAN_POINT ( 'NONE',  ( 27.16883889988624290, 22.17500000273120264, 19.73931689729373673 ) ) ;
#20537 = CARTESIAN_POINT ( 'NONE',  ( -12.13525491562420910, 80.19999999999998863, 8.816778784387098611 ) ) ;
#20538 = CARTESIAN_POINT ( 'NONE',  ( 33.58253175000000113, 76.22500000273119269, -10.91162601494193574 ) ) ;
#20539 = CARTESIAN_POINT ( 'NONE',  ( -10.04305231718579172, 65.59999999999999432, -30.90933677959248982 ) ) ;
#20540 = CARTESIAN_POINT ( 'NONE',  ( -2.092463501923844636E-15, 59.50000000000001421, -34.17252228774368916 ) ) ;
#20541 = CARTESIAN_POINT ( 'NONE',  ( -4.523095164977117273E-15, 16.12499999726880517, 24.62258325217400312 ) ) ;
#20542 = CARTESIAN_POINT ( 'NONE',  ( 33.58253175000000823, 64.02500000273118985, 10.91162601494192685 ) ) ;
#20543 = CARTESIAN_POINT ( 'NONE',  ( 23.41746825000000243, 11.22499999726881548, -7.608796670333727974 ) ) ;
#20544 = CARTESIAN_POINT ( 'NONE',  ( 27.16883889988624290, 76.17500000273118133, 19.73931689729373673 ) ) ;
#20545 = CARTESIAN_POINT ( 'NONE',  ( -2.162160676586882350E-15, 6.625000002731173510, -35.31076352940722529 ) ) ;
#20546 = CARTESIAN_POINT ( 'NONE',  ( -23.41746825000000598, 14.22499999726880660, 7.608796670333726198 ) ) ;
#20547 = CARTESIAN_POINT ( 'NONE',  ( -26.09010956794232428, 16.30246500092397355, 6.950374756619732253 ) ) ;
#20548 = EDGE_LOOP ( 'NONE', ( #27838, #28632, #28344, #19772, #19485, #15309, #30434, #30475, #23156, #18782, #27405, #22551 ) ) ;
#20549 = CARTESIAN_POINT ( 'NONE',  ( 20.75514604977249178, 41.82500000273119412, 28.56700777964553950 ) ) ;
#20550 = EDGE_CURVE ( 'NONE', #7704, #15702, #19999, .T. ) ;
#20551 = ORIENTED_EDGE ( 'NONE', *, *, #23429, .T. ) ;
#20552 = CARTESIAN_POINT ( 'NONE',  ( 2.740863092043355209E-13, 31.33593749999999289, 30.02300923189239512 ) ) ;
#20553 = FACE_OUTER_BOUND ( 'NONE', #12538, .T. ) ;
#20554 = CARTESIAN_POINT ( 'NONE',  ( 6.277390505771533514E-15, 3.000000005462379882, 34.17252228774368916 ) ) ;
#20555 = DIRECTION ( 'NONE',  ( -1.224646799147353207E-16, -1.499759782661857882E-32, 1.000000000000000000 ) ) ;
#20556 = CARTESIAN_POINT ( 'NONE',  ( 7.236395654485760609, 1.524999997268822183, -22.27133577429736633 ) ) ;
#20557 = CARTESIAN_POINT ( 'NONE',  ( 23.41746824999999887, 14.62499999726882294, 0.000000000000000000 ) ) ;
#20558 = PRODUCT_DEFINITION_SHAPE ( 'NONE', 'NONE',  #7646 ) ;
#20559 = CARTESIAN_POINT ( 'NONE',  ( -33.58253175000000113, 15.27500000273118985, -10.91162601494193218 ) ) ;
#20560 = CARTESIAN_POINT ( 'NONE',  ( -26.29305231718578995, 16.70000000546237473, 19.10302069950538595 ) ) ;
#20561 = CARTESIAN_POINT ( 'NONE',  ( 10.04305231718579705, 64.59999999999999432, 30.90933677959248982 ) ) ;
#20562 = CARTESIAN_POINT ( 'NONE',  ( 24.50000000000000000, 11.84999999453761710, -7.960532557706203605 ) ) ;
#20563 = DIRECTION ( 'NONE',  ( 0.000000000000000000, 0.000000000000000000, 1.000000000000000000 ) ) ;
#20564 = CARTESIAN_POINT ( 'NONE',  ( 30.02300923189239867, 62.85194416759064495, 0.04044903254992252006 ) ) ;
#20565 = CARTESIAN_POINT ( 'NONE',  ( -33.58253175000000113, 31.47500000273117493, 10.91162601494193929 ) ) ;
#20566 = CARTESIAN_POINT ( 'NONE',  ( -1.778240108872766143E-15, 44.00000000546238255, -32.49999999999999289 ) ) ;
#20567 = CARTESIAN_POINT ( 'NONE',  ( -7.505752307972844761, 41.79166666666666430, 28.01184896238304134 ) ) ;
#20568 = DIRECTION ( 'NONE',  ( 1.000000000000000000, 0.000000000000000000, 0.000000000000000000 ) ) ;
#20569 = CARTESIAN_POINT ( 'NONE',  ( -14.47279130897152122, 14.42499999726880056, 19.92008829642072243 ) ) ;
#20570 = CARTESIAN_POINT ( 'NONE',  ( 32.50000000000000000, 7.000000000000006217, -3.980102097228898626E-15 ) ) ;
#20571 = VECTOR ( 'NONE', #29005, 1000.000000000000000 ) ;
#20572 = CARTESIAN_POINT ( 'NONE',  ( 5.779280353836490358E-15, 74.50000000000001421, 32.49999999999999289 ) ) ;
#20573 = CARTESIAN_POINT ( 'NONE',  ( 14.01125832528330051, 57.11159749907603356, 24.18731323226221974 ) ) ;
#20574 = CARTESIAN_POINT ( 'NONE',  ( 20.75514604977248467, 50.42500000273118843, -28.56700777964554305 ) ) ;
#20575 = CARTESIAN_POINT ( 'NONE',  ( 33.58253175000000113, 62.47500000273118559, -10.91162601494193751 ) ) ;
#20576 = CARTESIAN_POINT ( 'NONE',  ( 6.486482029760648627E-15, 41.87500000273119127, 35.31076352940722529 ) ) ;
#20577 = DIRECTION ( 'NONE',  ( -1.000000000000000000, 0.000000000000000000, 0.000000000000000000 ) ) ;
#20578 = CARTESIAN_POINT ( 'NONE',  ( -26.07999730980477437, 14.86458333333333037, 6.988114217768305103 ) ) ;
#20579 = CARTESIAN_POINT ( 'NONE',  ( -26.29305231718579350, 61.79999999999999716, -19.10302069950537884 ) ) ;
#20580 = CARTESIAN_POINT ( 'NONE',  ( 8.327598234202002696E-15, -91.00000000000000000, 0.000000000000000000 ) ) ;
#20581 = CARTESIAN_POINT ( 'NONE',  ( 32.50000000000000711, 76.89999999999999147, 10.55989012756945122 ) ) ;
#20582 = CARTESIAN_POINT ( 'NONE',  ( -10.37757302488624411, 14.72500000273117848, -31.93888565452638417 ) ) ;
#20583 = CARTESIAN_POINT ( 'NONE',  ( 32.50000000000000711, 6.900000000000014566, 10.55989012756945122 ) ) ;
#20584 = DIRECTION ( 'NONE',  ( 0.000000000000000000, 1.000000000000000000, 0.000000000000000000 ) ) ;
#20585 = CARTESIAN_POINT ( 'NONE',  ( 24.50000000000000000, 9.749999994537628112, 0.000000000000000000 ) ) ;
#20586 = CARTESIAN_POINT ( 'NONE',  ( -19.06425588902558133, 20.01524333240935505, 19.11951029504797006 ) ) ;
#20587 = CARTESIAN_POINT ( 'NONE',  ( -26.29305231718579350, 40.30000000546237260, -19.10302069950537884 ) ) ;
#20588 = CARTESIAN_POINT ( 'NONE',  ( -32.50000000000000000, 11.90000000000000213, -10.55989012756945300 ) ) ;
#20589 = CARTESIAN_POINT ( 'NONE',  ( 20.75514604977248467, 24.42500000273119198, -28.56700777964554305 ) ) ;
#20590 = AXIS2_PLACEMENT_3D ( 'NONE', #22203, #22530, #17052 ) ;
#20591 = CARTESIAN_POINT ( 'NONE',  ( -27.95245687107222921, 35.63281249999998579, 2.498001805406602216E-13 ) ) ;
#20592 = ORIENTED_EDGE ( 'NONE', *, *, #22716, .F. ) ;
#20593 = CARTESIAN_POINT ( 'NONE',  ( 6.486482029760649416E-15, 69.62500000273118417, 35.31076352940723240 ) ) ;
#20594 = CARTESIAN_POINT ( 'NONE',  ( 7.505752307973351023, 44.94270833333332860, 28.01184896238290278 ) ) ;
#20595 = FACE_OUTER_BOUND ( 'NONE', #23206, .T. ) ;
#20596 = ORIENTED_EDGE ( 'NONE', *, *, #31314, .T. ) ;
#20597 = CARTESIAN_POINT ( 'NONE',  ( 26.02091320914851025, 59.12798583425730925, -14.97647472619946463 ) ) ;
#20598 = CARTESIAN_POINT ( 'NONE',  ( -0.04044903254992426173, 60.27381916759065206, 27.95245687107223276 ) ) ;
#20599 = ORIENTED_EDGE ( 'NONE', *, *, #3020, .T. ) ;
#20600 = CARTESIAN_POINT ( 'NONE',  ( -10.37757302488624411, 8.725000002731173154, -31.93888565452638417 ) ) ;
#20601 = ADVANCED_FACE ( 'NONE', ( #25946 ), #31593, .T. ) ;
#20602 = CARTESIAN_POINT ( 'NONE',  ( 20.47846945139867003, 14.85899333240935505, -20.53372385742107653 ) ) ;
#20603 = DIRECTION ( 'NONE',  ( -0.000000000000000000, -1.000000000000000000, -0.000000000000000000 ) ) ;
#20604 = CARTESIAN_POINT ( 'NONE',  ( 33.58253175000000113, 34.47500000273119980, -10.91162601494193751 ) ) ;
#20605 = CARTESIAN_POINT ( 'NONE',  ( -32.50000000000000000, 34.60000000546236976, 10.55989012756946366 ) ) ;
#20606 = CIRCLE ( 'NONE', #3081, 26.50000000000000355 ) ;
#20607 = CARTESIAN_POINT ( 'NONE',  ( -15.00000000000000000, 77.89999999999999147, -4.873795443493594171 ) ) ;
#20608 = LINE ( 'NONE', #28815, #13245 ) ;
#20609 = CARTESIAN_POINT ( 'NONE',  ( 6.486482029760649416E-15, 21.62500000273119483, 35.31076352940723240 ) ) ;
#20610 = CARTESIAN_POINT ( 'NONE',  ( 5.485887633599118468E-07, 52.00000000000003553, -32.49999999999999289 ) ) ;
#20611 = CARTESIAN_POINT ( 'NONE',  ( 33.58253175000000113, 48.37500000273120548, -4.112674001490185761E-15 ) ) ;
#20612 = FILL_AREA_STYLE ('',( #30360 ) ) ;
#20613 = CARTESIAN_POINT ( 'NONE',  ( -32.50000000000000000, 29.89999999999998437, -10.55989012756945478 ) ) ;
#20614 = CARTESIAN_POINT ( 'NONE',  ( -32.50000000000000000, 29.89999999999998437, -10.55989012756945478 ) ) ;
#20615 = CARTESIAN_POINT ( 'NONE',  ( 19.82091636218621034, 1.799999999999996048, 14.40073868116559730 ) ) ;
#20616 = CARTESIAN_POINT ( 'NONE',  ( 10.37757302488624767, 67.72500000273117848, 31.93888565452638417 ) ) ;
#20617 = FACE_OUTER_BOUND ( 'NONE', #10625, .T. ) ;
#20618 = CARTESIAN_POINT ( 'NONE',  ( -19.82091636218621389, 15.19999999999999218, 14.40073868116558842 ) ) ;
#20619 = CARTESIAN_POINT ( 'NONE',  ( 27.16883889988623935, 58.57500000273119412, -19.73931689729374384 ) ) ;
#20620 = CARTESIAN_POINT ( 'NONE',  ( 26.29305231718578995, 73.19999999999998863, -19.10302069950538240 ) ) ;
#20621 = CARTESIAN_POINT ( 'NONE',  ( 10.37757302488624767, 9.725000002731187365, 31.93888565452638417 ) ) ;
#20622 = CARTESIAN_POINT ( 'NONE',  ( -24.50000000000001066, 8.849999994537624204, 7.960532557706201828 ) ) ;
#20623 = CARTESIAN_POINT ( 'NONE',  ( 26.09010956794232428, 28.33371500092397355, -6.950374756619718042 ) ) ;
#20624 =( BOUNDED_CURVE ( )  B_SPLINE_CURVE ( 2, ( #17785, #82, #7988, #5418, #13140, #23613, #28413, #10569, #2152, #18474, #30984, #15209, #23096 ),
 .UNSPECIFIED., .F., .T. ) 
 B_SPLINE_CURVE_WITH_KNOTS ( ( 3, 2, 2, 2, 2, 2, 3 ),
 ( 0.4166666666666666852, 0.4222222222222222210, 0.4333333333333333481, 0.4444444444444444198, 0.4555555555555555469, 0.4666666666666666741, 0.4722222222222222099 ),
 .UNSPECIFIED. ) 
 CURVE ( )  GEOMETRIC_REPRESENTATION_ITEM ( )  RATIONAL_B_SPLINE_CURVE ( ( 0.9755282581475767101, 0.9755282581475768211, 1.000000000000000000, 0.9510565162951535312, 1.000000000000000000, 0.9510565162951535312, 1.000000000000000000, 0.9510565162951535312, 1.000000000000000000, 0.9510565162951535312, 1.000000000000000000, 0.9755282581475768211, 0.9755282581475765991 ) ) 
 REPRESENTATION_ITEM ( '' )  );
#20625 = CARTESIAN_POINT ( 'NONE',  ( -3.712076227271900841E-14, 10.24999999453763344, -24.50000000000000000 ) ) ;
#20626 = CARTESIAN_POINT ( 'NONE',  ( -27.16883889988624290, 34.92500000273117422, -19.73931689729374028 ) ) ;
#20627 = DIRECTION ( 'NONE',  ( -0.000000000000000000, -1.000000000000000000, -0.000000000000000000 ) ) ;
#20628 = CARTESIAN_POINT ( 'NONE',  ( 0.000000000000000000, 0.000000000000000000, 0.000000000000000000 ) ) ;
#20629 = CARTESIAN_POINT ( 'NONE',  ( -28.00173670424535644, 47.80170166574269786, 7.543491769121936308 ) ) ;
#20630 = CARTESIAN_POINT ( 'NONE',  ( -20.08610463437157989, 60.20000000546237828, -27.64615127144129758 ) ) ;
#20631 = CARTESIAN_POINT ( 'NONE',  ( 2.688165632520823219E-15, 79.87500000273114154, 14.63369212191046387 ) ) ;
#20632 = CARTESIAN_POINT ( 'NONE',  ( -8.891200544363830713E-16, 79.50000000000000000, -15.00000000000000000 ) ) ;
#20633 = TOROIDAL_SURFACE ( 'NONE', #29375, 30.16025403784430736, 1.500000000000010436 ) ;
#20634 = CARTESIAN_POINT ( 'NONE',  ( -6.950374756619247307, 60.97878499907603356, 26.09010956794245217 ) ) ;
#20635 = CARTESIAN_POINT ( 'NONE',  ( 32.50000000000000000, 63.60000000546238397, -10.55989012756945833 ) ) ;
#20636 = CARTESIAN_POINT ( 'NONE',  ( -2.092463501923844636E-15, 76.00000000546235412, -34.17252228774368916 ) ) ;
#20637 = DIRECTION ( 'NONE',  ( -1.000000000000000000, 0.000000000000000000, 0.000000000000000000 ) ) ;
#20638 = CARTESIAN_POINT ( 'NONE',  ( 27.16883889988624290, 36.17500000273120264, 19.73931689729373673 ) ) ;
#20639 = CARTESIAN_POINT ( 'NONE',  ( 23.41746824999999887, 9.224999997268820806, -7.608796670333727974 ) ) ;
#20640 = ORIENTED_EDGE ( 'NONE', *, *, #28233, .T. ) ;
#20641 = CARTESIAN_POINT ( 'NONE',  ( -2.162160676586881955E-15, 72.87500000273115575, -35.31076352940723240 ) ) ;
#20642 = CARTESIAN_POINT ( 'NONE',  ( 32.50000000000000000, 25.60000000546239107, -10.55989012756945833 ) ) ;
#20643 = CARTESIAN_POINT ( 'NONE',  ( 20.50609665441005092, 44.65624999999999289, 20.50609665440969209 ) ) ;
#20644 = CARTESIAN_POINT ( 'NONE',  ( -26.00068869287368756, 63.41927083333333570, -15.01150461594595775 ) ) ;
#20645 = EDGE_CURVE ( 'NONE', #22878, #17411, #22397, .T. ) ;
#20646 = CARTESIAN_POINT ( 'NONE',  ( 10.37757302488624767, 53.97500000273119980, 31.93888565452638417 ) ) ;
#20647 = EDGE_CURVE ( 'NONE', #2121, #22307, #9671, .T. ) ;
#20648 = CARTESIAN_POINT ( 'NONE',  ( -20.08610463437156923, 64.80000000546237970, 27.64615127144130113 ) ) ;
#20649 = ORIENTED_EDGE ( 'NONE', *, *, #7366, .F. ) ;
#20650 = CARTESIAN_POINT ( 'NONE',  ( -20.08610463437157989, 10.20000000546238539, -27.64615127144129758 ) ) ;
#20651 = CARTESIAN_POINT ( 'NONE',  ( 27.16883889988623935, 42.32500000273120833, -19.73931689729374384 ) ) ;
#20652 = DIRECTION ( 'NONE',  ( -0.000000000000000000, -1.000000000000000000, -0.000000000000000000 ) ) ;
#20653 = CARTESIAN_POINT ( 'NONE',  ( -33.58253175000000113, 69.47500000273116427, 10.91162601494193929 ) ) ;
#20654 = CARTESIAN_POINT ( 'NONE',  ( -20.08610463437157989, 6.200000005462364960, -27.64615127144129758 ) ) ;
#20655 = CARTESIAN_POINT ( 'NONE',  ( 20.75514604977248467, 64.42500000273116711, -28.56700777964554305 ) ) ;
#20656 = CARTESIAN_POINT ( 'NONE',  ( -15.01150461594595775, 14.43489583333332860, 26.00068869287368756 ) ) ;
#20657 = CARTESIAN_POINT ( 'NONE',  ( 20.08610463437158344, 44.69999999999998153, 27.64615127144129403 ) ) ;
#20658 = DIRECTION ( 'NONE',  ( -0.000000000000000000, -1.000000000000000000, -0.000000000000000000 ) ) ;
#20659 = CARTESIAN_POINT ( 'NONE',  ( -27.16883889988623935, 9.575000002731204773, 19.73931689729374739 ) ) ;
#20660 = CARTESIAN_POINT ( 'NONE',  ( -1.778240108872766143E-15, 6.000000005462371888, -32.49999999999999289 ) ) ;
#20661 = CARTESIAN_POINT ( 'NONE',  ( 19.11951029504797006, 32.90586833240934794, 19.06425588902558133 ) ) ;
#20662 = CARTESIAN_POINT ( 'NONE',  ( -8.601468415847518756, 79.07500000273121543, -11.83890561707634781 ) ) ;
#20663 = CARTESIAN_POINT ( 'NONE',  ( -33.58253175000000113, 79.37500000273118417, 0.000000000000000000 ) ) ;
#20664 = CYLINDRICAL_SURFACE ( 'NONE', #11181, 15.00000000000000000 ) ;
#20665 = CARTESIAN_POINT ( 'NONE',  ( -10.37757302488623701, 71.77500000273118985, 31.93888565452638417 ) ) ;
#20666 = ORIENTED_EDGE ( 'NONE', *, *, #19642, .T. ) ;
#20667 = VECTOR ( 'NONE', #2706, 1000.000000000000000 ) ;
#20668 = CARTESIAN_POINT ( 'NONE',  ( 7.236395654485760609, 11.52499999726880375, -22.27133577429736633 ) ) ;
#20669 = CARTESIAN_POINT ( 'NONE',  ( 14.47279130897151767, 2.324999997268806240, 19.92008829642072953 ) ) ;
#20670 = CARTESIAN_POINT ( 'NONE',  ( 2.584737979205441561E-13, 48.52343750000000000, 27.95245687107222921 ) ) ;
#20671 = EDGE_CURVE ( 'NONE', #21883, #5385, #23656, .T. ) ;
#20672 = CARTESIAN_POINT ( 'NONE',  ( -20.75514604977248112, 61.42500000273118133, 28.56700777964554661 ) ) ;
#20673 = CARTESIAN_POINT ( 'NONE',  ( -33.58253175000000113, 15.47500000273118381, 10.91162601494193929 ) ) ;
#20674 = CARTESIAN_POINT ( 'NONE',  ( 6.486482029760649416E-15, 1.875000002731192383, 35.31076352940723240 ) ) ;
#20675 = CARTESIAN_POINT ( 'NONE',  ( 13.97622843553589966, 33.34114583333332860, -24.20753774853756113 ) ) ;
#20676 = CARTESIAN_POINT ( 'NONE',  ( 7.543491769121427382, 24.32329833425730214, -28.00173670424548433 ) ) ;
#20677 = CARTESIAN_POINT ( 'NONE',  ( -28.01184896238290278, 66.42708333333332860, 7.505752307973363457 ) ) ;
#20678 = CARTESIAN_POINT ( 'NONE',  ( 10.37757302488624056, 4.525000002731191628, -31.93888565452638417 ) ) ;
#20679 = CARTESIAN_POINT ( 'NONE',  ( 32.87414713444668024, 52.00000000000002132, 6.322578566052129645 ) ) ;
#20680 = CARTESIAN_POINT ( 'NONE',  ( 10.04305231718578817, 39.40000000000000568, -30.90933677959249337 ) ) ;
#20681 = CARTESIAN_POINT ( 'NONE',  ( -20.75514604977248823, 46.82500000273117990, -28.56700777964554305 ) ) ;
#20682 = CARTESIAN_POINT ( 'NONE',  ( -23.41746824999999887, 7.624999997268816720, -2.867812753649727150E-15 ) ) ;
#20683 = CARTESIAN_POINT ( 'NONE',  ( -26.07999730980490583, 66.71354166666665719, -6.988114217767815717 ) ) ;
#20684 = ORIENTED_EDGE ( 'NONE', *, *, #7884, .F. ) ;
#20685 = CARTESIAN_POINT ( 'NONE',  ( -10.37757302488624411, 50.97500000273118559, -31.93888565452638417 ) ) ;
#20686 = CARTESIAN_POINT ( 'NONE',  ( 20.08610463437158344, 59.20000000546237828, 27.64615127144129403 ) ) ;
#20687 = CARTESIAN_POINT ( 'NONE',  ( 24.22776226481241224, 45.37798583425732346, -13.94119854578936923 ) ) ;
#20688 = CARTESIAN_POINT ( 'NONE',  ( 6.486482029760649416E-15, 75.87500000273119838, 35.31076352940723240 ) ) ;
#20689 = ORIENTED_EDGE ( 'NONE', *, *, #12937, .F. ) ;
#20690 = CARTESIAN_POINT ( 'NONE',  ( 33.58253175000000823, 24.02500000273117564, 10.91162601494192863 ) ) ;
#20691 = CARTESIAN_POINT ( 'NONE',  ( -30.02300923189239512, 15.00781249999999467, 2.654126918244515359E-13 ) ) ;
#20692 = EDGE_LOOP ( 'NONE', ( #1399, #28194, #6438, #14622 ) ) ;
#20693 = CARTESIAN_POINT ( 'NONE',  ( -5.147494310547322094, 57.55125428154683931, -32.50000000000003553 ) ) ;
#20694 = CARTESIAN_POINT ( 'NONE',  ( 33.58253175000000113, 64.22500000273117848, -10.91162601494193751 ) ) ;
#20695 = CARTESIAN_POINT ( 'NONE',  ( 7.505752307973351023, 41.50520833333333570, 28.01184896238290278 ) ) ;
#20696 = CARTESIAN_POINT ( 'NONE',  ( 24.50000000000000355, 15.89999999999999147, 7.960532557706212486 ) ) ;
#20697 = CARTESIAN_POINT ( 'NONE',  ( 23.41746824999999887, 5.024999997268808194, 7.608796670333735079 ) ) ;
#20698 = CARTESIAN_POINT ( 'NONE',  ( -20.75514604977248823, 6.825000002731195892, -28.56700777964554305 ) ) ;
#20699 = CARTESIAN_POINT ( 'NONE',  ( 26.29305231718579350, 28.79999999999999361, 19.10302069950537529 ) ) ;
#20700 = CARTESIAN_POINT ( 'NONE',  ( -15.04653450569338524, 55.39284749907604066, -25.98046417659831775 ) ) ;
#20701 = CARTESIAN_POINT ( 'NONE',  ( -9.270509831248423538, 79.95000000546235697, -12.75976212528059861 ) ) ;
#20702 = CARTESIAN_POINT ( 'NONE',  ( 7.505752307972854531, 64.13541666666667140, -28.01184896238303423 ) ) ;
#20703 = CARTESIAN_POINT ( 'NONE',  ( -24.50000000000000711, 14.84999999453763841, 7.960532557706201828 ) ) ;
#20704 = EDGE_CURVE ( 'NONE', #24126, #12037, #23888, .T. ) ;
#20705 = CARTESIAN_POINT ( 'NONE',  ( -20.08610463437157989, 15.69999999999999929, -27.64615127144129758 ) ) ;
#20706 = CARTESIAN_POINT ( 'NONE',  ( -24.50000000000000355, 12.64999999453762136, -7.960532557706207157 ) ) ;
#20707 = CARTESIAN_POINT ( 'NONE',  ( -15.00000000000000000, 72.25000000546238255, 0.000000000000000000 ) ) ;
#20708 = CARTESIAN_POINT ( 'NONE',  ( -26.07999730980490583, 22.02604166666666430, -6.988114217767815717 ) ) ;
#20709 = CARTESIAN_POINT ( 'NONE',  ( -20.75514604977248112, 29.42500000273118133, 28.56700777964554661 ) ) ;
#20710 = CARTESIAN_POINT ( 'NONE',  ( -4.300734207923755825, 71.27500000273117564, 13.23629886949340673 ) ) ;
#20711 = CARTESIAN_POINT ( 'NONE',  ( -27.16883889988623935, 39.57500000273118701, 19.73931689729374739 ) ) ;
#20712 = CARTESIAN_POINT ( 'NONE',  ( -33.58253175000000113, 23.37500000273118417, 0.000000000000000000 ) ) ;
#20713 = CARTESIAN_POINT ( 'NONE',  ( -5.147494310547430452, 63.55125428154684641, -32.49999999999999289 ) ) ;
#20714 = ADVANCED_FACE ( 'NONE', ( #15668, #26118 ), #13078, .T. ) ;
#20715 = CARTESIAN_POINT ( 'NONE',  ( -33.58253175000000113, 77.02500000273120406, -10.91162601494193041 ) ) ;
#20716 = CARTESIAN_POINT ( 'NONE',  ( -26.29305231718579350, 65.79999999999999716, -19.10302069950537884 ) ) ;
#20717 = CARTESIAN_POINT ( 'NONE',  ( 6.277390505771533514E-15, 58.49999999999997868, 34.17252228774368916 ) ) ;
#20718 = CARTESIAN_POINT ( 'NONE',  ( 18.94512977948576093, 14.82499999726882933, -13.76444248337722875 ) ) ;
#20719 = CARTESIAN_POINT ( 'NONE',  ( -27.16883889988624290, 66.92500000273119554, -19.73931689729374028 ) ) ;
#20720 = CARTESIAN_POINT ( 'NONE',  ( 1.507698388325705758E-15, 11.62499999726880340, -24.62258325217400312 ) ) ;
#20721 = CARTESIAN_POINT ( 'NONE',  ( 20.75514604977248467, 70.67500000273118133, -28.56700777964554305 ) ) ;
#20722 = CARTESIAN_POINT ( 'NONE',  ( 27.16883889988623935, 6.325000002731173687, -19.73931689729374384 ) ) ;
#20723 = CARTESIAN_POINT ( 'NONE',  ( 1.507698388325705758E-15, 17.62499999726881938, -24.62258325217400312 ) ) ;
#20724 = CARTESIAN_POINT ( 'NONE',  ( -7.025853678916393008, 12.29204833425730925, 26.06988505166735592 ) ) ;
#20725 =( BOUNDED_CURVE ( )  B_SPLINE_CURVE ( 2, ( #24217, #26453, #27797, #14419, #6523, #24706, #32590, #22472, #21811, #1013, #16995, #11834, #32757 ),
 .UNSPECIFIED., .F., .F. ) 
 B_SPLINE_CURVE_WITH_KNOTS ( ( 3, 2, 2, 2, 2, 2, 3 ),
 ( 0.7500000000000000000, 0.7512820512820512775, 0.7538461538461538325, 0.7564102564102563875, 0.7589743589743589425, 0.7615384615384614975, 0.7628205128205127750 ),
 .UNSPECIFIED. ) 
 CURVE ( )  GEOMETRIC_REPRESENTATION_ITEM ( )  RATIONAL_B_SPLINE_CURVE ( ( 0.9755282581475768211, 0.9755282581475768211, 1.000000000000000000, 0.9510565162951535312, 1.000000000000000000, 0.9510565162951535312, 1.000000000000000000, 0.9510565162951535312, 1.000000000000000000, 0.9510565162951535312, 1.000000000000000000, 0.9755282581475768211, 0.9755282581475768211 ) ) 
 REPRESENTATION_ITEM ( '' )  );
#20726 = ORIENTED_EDGE ( 'NONE', *, *, #4609, .T. ) ;
#20727 = CARTESIAN_POINT ( 'NONE',  ( 33.58253175000000113, 44.12500000273119127, -4.112674001490185761E-15 ) ) ;
#20728 = ORIENTED_EDGE ( 'NONE', *, *, #21220, .F. ) ;
#20729 = CARTESIAN_POINT ( 'NONE',  ( -28.01184896238290278, 42.36458333333332860, 7.505752307973363457 ) ) ;
#20730 = CARTESIAN_POINT ( 'NONE',  ( 0.000000000000000000, 102.0000000000000284, 0.000000000000000000 ) ) ;
#20731 = CARTESIAN_POINT ( 'NONE',  ( 26.29305231718578995, 5.700000005462377395, -19.10302069950538240 ) ) ;
#20732 = CARTESIAN_POINT ( 'NONE',  ( 33.58253175000000113, 78.12500000273119838, -4.112674001490185761E-15 ) ) ;
#20733 = CARTESIAN_POINT ( 'NONE',  ( -7.236395654485763274, 4.524999997268825069, 22.27133577429736633 ) ) ;
#20734 = CARTESIAN_POINT ( 'NONE',  ( 7.236395654485760609, 17.02499999726880731, -22.27133577429736633 ) ) ;
#20735 = CARTESIAN_POINT ( 'NONE',  ( 6.486482029760649416E-15, 13.87500000273117529, 35.31076352940723240 ) ) ;
#20736 = CARTESIAN_POINT ( 'NONE',  ( 10.04305231718578817, 17.90000000546238113, -30.90933677959249337 ) ) ;
#20737 = CARTESIAN_POINT ( 'NONE',  ( -26.29305231718578995, 66.19999999999997442, 19.10302069950538595 ) ) ;
#20738 = CARTESIAN_POINT ( 'NONE',  ( 7.890940483122900408E-14, 12.24999999453763166, -24.50000000000000000 ) ) ;
#20739 = CARTESIAN_POINT ( 'NONE',  ( 12.11607355459420887, -70.99969134886156041, 0.000000000000000000 ) ) ;
#20740 = CARTESIAN_POINT ( 'NONE',  ( -7.505752307972844761, 14.29166666666666430, 28.01184896238304134 ) ) ;
#20741 = CARTESIAN_POINT ( 'NONE',  ( -32.50000000000000000, 32.60000000546237686, 10.55989012756946366 ) ) ;
#20742 = CARTESIAN_POINT ( 'NONE',  ( -26.00068869287340334, 42.22135416666666430, 15.01150461594643559 ) ) ;
#20743 = PRODUCT_CONTEXT ( 'NONE', #25441, 'mechanical' ) ;
#20744 = CYLINDRICAL_SURFACE ( 'NONE', #33238, 32.50000000000000000 ) ;
#20745 = CARTESIAN_POINT ( 'NONE',  ( -18.94512977948576093, 14.32499999726882756, 13.76444248337722698 ) ) ;
#20746 = CARTESIAN_POINT ( 'NONE',  ( -32.50000000000000000, 6.099999999999981881, 10.55989012756946366 ) ) ;
#20747 = CARTESIAN_POINT ( 'NONE',  ( 5.779280353836490358E-15, 17.00000000546237899, 32.49999999999999289 ) ) ;
#20748 = CARTESIAN_POINT ( 'NONE',  ( 24.18731323226221974, 56.25222249907602645, -14.01125832528328985 ) ) ;
#20749 = CARTESIAN_POINT ( 'NONE',  ( 33.58253175000000113, 50.22500000273118559, -10.91162601494193751 ) ) ;
#20750 = CARTESIAN_POINT ( 'NONE',  ( 10.37757302488624056, 62.77500000273118985, -31.93888565452638417 ) ) ;
#20751 = CARTESIAN_POINT ( 'NONE',  ( -33.58253175000000113, 41.37500000273119838, 0.000000000000000000 ) ) ;
#20752 = DIRECTION ( 'NONE',  ( 1.000000000000000000, 0.000000000000000000, 0.000000000000000000 ) ) ;
#20753 = CARTESIAN_POINT ( 'NONE',  ( 32.50000000000000711, 15.40000000546236514, 10.55989012756945122 ) ) ;
#20754 = CARTESIAN_POINT ( 'NONE',  ( -1.778240108872766143E-15, 31.49999999999998579, -32.49999999999999289 ) ) ;
#20755 = CARTESIAN_POINT ( 'NONE',  ( -26.29305231718578995, 28.20000000000000284, 19.10302069950538595 ) ) ;
#20756 = CARTESIAN_POINT ( 'NONE',  ( -33.58253175000000113, 17.02500000273118985, -10.91162601494193218 ) ) ;
#20757 = FACE_OUTER_BOUND ( 'NONE', #11291, .T. ) ;
#20758 = DIRECTION ( 'NONE',  ( -1.000000000000000000, -1.224646799147353454E-16, 0.000000000000000000 ) ) ;
#20759 = CARTESIAN_POINT ( 'NONE',  ( 0.000000000000000000, 111.9999999999999858, 0.000000000000000000 ) ) ;
#20760 = CARTESIAN_POINT ( 'NONE',  ( -19.11951029504797006, 20.87461833240935505, -19.06425588902558133 ) ) ;
#20761 = CARTESIAN_POINT ( 'NONE',  ( 32.50000000000000000, 37.60000000546235555, -10.55989012756945833 ) ) ;
#20762 = CARTESIAN_POINT ( 'NONE',  ( 7.570916362186213000, 18.14999999453761959, -23.30088464923126423 ) ) ;
#20763 = CARTESIAN_POINT ( 'NONE',  ( -33.58253175000000113, 29.02500000273119340, -10.91162601494193041 ) ) ;
#20764 = CARTESIAN_POINT ( 'NONE',  ( -2.428612866367529427E-13, 43.36718749999999289, -27.95245687107222921 ) ) ;
#20765 = ORIENTED_EDGE ( 'NONE', *, *, #12073, .T. ) ;
#20766 = CARTESIAN_POINT ( 'NONE',  ( -33.58253175000000113, 65.02500000273118985, -10.91162601494193218 ) ) ;
#20767 = CARTESIAN_POINT ( 'NONE',  ( 28.01184896238290278, 47.52083333333332860, -7.505752307973347470 ) ) ;
#20768 = ORIENTED_EDGE ( 'NONE', *, *, #14495, .F. ) ;
#20769 = CARTESIAN_POINT ( 'NONE',  ( -20.47846945139902175, 65.00038166759063074, -20.53372385742072481 ) ) ;
#20770 = CARTESIAN_POINT ( 'NONE',  ( 30.02300923189239867, 18.16444416759064140, 0.04044903254992252006 ) ) ;
#20771 = CARTESIAN_POINT ( 'NONE',  ( 20.75514604977248467, 6.425000002731192872, -28.56700777964554305 ) ) ;
#20772 = PLANE ( 'NONE',  #10828 ) ;
#20773 = CARTESIAN_POINT ( 'NONE',  ( 6.486482029760649416E-15, 33.87500000273118417, 35.31076352940723240 ) ) ;
#20774 = CARTESIAN_POINT ( 'NONE',  ( -20.08610463437156923, 38.80000000546237260, 27.64615127144130113 ) ) ;
#20775 = CARTESIAN_POINT ( 'NONE',  ( 15.00000000000000000, 75.10000000000002274, -4.873795443493596835 ) ) ;
#20776 = CARTESIAN_POINT ( 'NONE',  ( -26.29305231718579350, 47.80000000000001137, -19.10302069950537884 ) ) ;
#20777 = CARTESIAN_POINT ( 'NONE',  ( 33.58253175000000113, 22.22500000273117493, -10.91162601494193751 ) ) ;
#20778 = CARTESIAN_POINT ( 'NONE',  ( -9.270509831248423538, 81.70000000000000284, -12.75976212528059861 ) ) ;
#20779 = CARTESIAN_POINT ( 'NONE',  ( -27.16883889988624290, 49.17500000273117422, -19.73931689729374028 ) ) ;
#20780 =( NAMED_UNIT ( * ) PLANE_ANGLE_UNIT ( ) SI_UNIT ( $, .RADIAN. ) );
#20781 = CARTESIAN_POINT ( 'NONE',  ( -20.08610463437156923, 32.29999999999999716, 27.64615127144130113 ) ) ;
#20782 = CARTESIAN_POINT ( 'NONE',  ( -26.29305231718579350, 29.79999999999999361, -19.10302069950537884 ) ) ;
#20783 = CARTESIAN_POINT ( 'NONE',  ( -19.82091636218621034, 6.800000000000000711, -14.40073868116559552 ) ) ;
#20784 = CARTESIAN_POINT ( 'NONE',  ( -2.162160676586881955E-15, 72.62500000273118417, -35.31076352940723240 ) ) ;
#20785 = CARTESIAN_POINT ( 'NONE',  ( 2.489536152421872915E-14, 77.50000000000001421, -32.49999999999999289 ) ) ;
#20786 = CARTESIAN_POINT ( 'NONE',  ( -3.880418787951104953, 15.44874571845315359, 24.50000000000000711 ) ) ;
#20787 = CARTESIAN_POINT ( 'NONE',  ( 6.486482029760648627E-15, 57.87500000273117706, 35.31076352940722529 ) ) ;
#20788 = CARTESIAN_POINT ( 'NONE',  ( -14.45873412499999944, 81.68750000136559208, 0.000000000000000000 ) ) ;
#20789 = CARTESIAN_POINT ( 'NONE',  ( -20.75514604977248823, 10.82500000273118701, -28.56700777964554305 ) ) ;
#20790 = CARTESIAN_POINT ( 'NONE',  ( -27.95245687107223986, 26.75819416759064495, -0.04044903254993292840 ) ) ;
#20791 = EDGE_CURVE ( 'NONE', #5766, #29627, #18013, .T. ) ;
#20792 = CARTESIAN_POINT ( 'NONE',  ( 15.14183272437242422, 10.04999999453761639, -20.84094480462497856 ) ) ;
#20793 = CARTESIAN_POINT ( 'NONE',  ( -20.75514604977248823, 36.82500000273117990, -28.56700777964554305 ) ) ;
#20794 = FACE_BOUND ( 'NONE', #4538, .T. ) ;
#20795 = EDGE_CURVE ( 'NONE', #4197, #32174, #17798, .T. ) ;
#20796 = CARTESIAN_POINT ( 'NONE',  ( 11.25946833292375793, 79.67500000273119554, 8.180482586598731842 ) ) ;
#20797 = CARTESIAN_POINT ( 'NONE',  ( 26.02091320914876960, 49.95013916574269786, 14.97647472619900455 ) ) ;
#20798 = CARTESIAN_POINT ( 'NONE',  ( -10.04305231718579172, 52.10000000546237686, -30.90933677959248982 ) ) ;
#20799 = CARTESIAN_POINT ( 'NONE',  ( 4.300734207923761154, 75.97500000273122112, 13.23629886949340495 ) ) ;
#20800 = CARTESIAN_POINT ( 'NONE',  ( 32.50000000000000000, 61.09999999999998721, -10.55989012756945833 ) ) ;
#20801 = CARTESIAN_POINT ( 'NONE',  ( -24.20753774853730889, 14.72135416666666607, 13.97622843553633842 ) ) ;
#20802 = CARTESIAN_POINT ( 'NONE',  ( 15.14183272437242422, 0.2999999999999904965, -20.84094480462497856 ) ) ;
#20803 = CARTESIAN_POINT ( 'NONE',  ( -32.50000000000000000, 66.40000000546238823, -10.55989012756945478 ) ) ;
#20804 = CARTESIAN_POINT ( 'NONE',  ( 7.505752307972854531, 19.44791666666666075, -28.01184896238303423 ) ) ;
#20805 = CARTESIAN_POINT ( 'NONE',  ( 33.58253175000000113, 36.47500000273119269, -10.91162601494193751 ) ) ;
#20806 = CARTESIAN_POINT ( 'NONE',  ( 18.94512977948576093, 7.324999997268822227, -13.76444248337722875 ) ) ;
#20807 = EDGE_LOOP ( 'NONE', ( #9369, #23413 ) ) ;
#20808 = CARTESIAN_POINT ( 'NONE',  ( -33.58253175000000113, 77.27500000273117564, -10.91162601494193218 ) ) ;
#20809 = CARTESIAN_POINT ( 'NONE',  ( 20.08610463437158344, 21.20000000546238894, 27.64615127144129403 ) ) ;
#20810 = CARTESIAN_POINT ( 'NONE',  ( 20.50609665440969565, 40.35937499999999289, -20.50609665441004736 ) ) ;
#20811 = CARTESIAN_POINT ( 'NONE',  ( 2.740863092043355209E-13, 62.27343749999999289, 30.02300923189239512 ) ) ;
#20812 = CARTESIAN_POINT ( 'NONE',  ( -33.58253175000000113, 55.37500000273118417, 0.000000000000000000 ) ) ;
#20813 = CARTESIAN_POINT ( 'NONE',  ( -10.04305231718578462, 58.90000000546238823, 30.90933677959249337 ) ) ;
#20814 = DIRECTION ( 'NONE',  ( 0.000000000000000000, 1.000000000000000000, 0.000000000000000000 ) ) ;
#20815 = CARTESIAN_POINT ( 'NONE',  ( -20.75514604977248823, 42.82500000273119412, -28.56700777964554305 ) ) ;
#20816 = CARTESIAN_POINT ( 'NONE',  ( 0.000000000000000000, 16.99999999999998579, -15.00000000000000000 ) ) ;
#20817 = CARTESIAN_POINT ( 'NONE',  ( -33.58253175000000113, 71.27500000273118985, -10.91162601494193218 ) ) ;
#20818 = CARTESIAN_POINT ( 'NONE',  ( -26.50000000000000000, -15.84529946162075653, 3.245314017740485765E-15 ) ) ;
#20819 = CARTESIAN_POINT ( 'NONE',  ( 10.37757302488624056, 62.52500000273118985, -31.93888565452638417 ) ) ;
#20820 = CARTESIAN_POINT ( 'NONE',  ( -20.50609665441004736, 11.99999999999999645, -20.50609665440969565 ) ) ;
#20821 = CARTESIAN_POINT ( 'NONE',  ( -10.04305231718579172, 45.60000000000000142, -30.90933677959248982 ) ) ;
#20822 = CARTESIAN_POINT ( 'NONE',  ( 14.47279130897151767, 2.924999997268815655, -19.92008829642072598 ) ) ;
#20823 =( BOUNDED_SURFACE ( )  B_SPLINE_SURFACE ( 1, 2, ( 
 ( #12844, #23318, #30853, #23487, #28791, #4773, #25547, #33948, #7344, #15251, #18175, #2193, #12668, #23136, #26228, #15601, #2549, #31366, #2027, #18347, #28115, #33783, #13180, #12501, #31199, #23658, #7690, #33428, #9925, #33603, #10101, #20581, #31026, #7523, #18007, #5117, #29459, #3391, #295, #5962, #14023, #23995, #13695, #13861, #3060, #24326, #18517, #630, #24487, #16113, #26396, #31537, #466, #16605, #19180, #5459, #10782, #800, #26565, #8031, #13532, #10949, #21259, #28963, #11282, #29126, #16276, #13355, #29618, #5629, #31704, #8360, #26734, #3227, #21425, #8196, #11120, #31866, #19018, #21760, #2889, #8531, #24160, #18848, #29296, #21588, #8697, #23830, #15940, #21091, #5794, #32203, #6121, #32034, #27058, #3551, #16440, #18687, #26892, #10611, #30122, #17271, #32367, #1467, #14357, #6464, #9191, #1630, #11943, #25154, #960, #1120, #6792, #22412, #14524, #16938, #6625, #12108, #17104, #27563, #11605, #4222, #9535, #32531, #6292, #14696, #22087, #9031, #32860, #19511, #29959, #27395, #30463, #30291, #27733, #22580, #19346, #33031, #8861, #4049, #6961, #3884, #9357, #1292, #11440, #29788, #24983, #16768, #20017, #21917, #24815, #11774, #17446, #27227, #19838, #4389, #22254, #3721, #14191, #32697, #27907, #14863, #24646, #19676, #28580, #7302, #12282, #28246, #17786, #15040, #22756, #18136, #9882, #30985, #28073, #10400, #20361, #25505, #23097, #7485, #17965, #30807, #12459, #15385, #12628, #33741, #5076, #17611, #23276, #28414, #4729, #15210, #25841, #23449, #4562, #33206, #1806, #33560, #15562, #26014, #2328, #20879, #2507, #4904, #7131, #20540, #22929, #12804, #7650, #9709, #10236, #25673, #2154, #10060, #12974, #20717, #33910, #25327, #1984, #31158, #31328, #7819, #18308, #28753, #5250, #20191, #30634, #33385, #18977, #24290, #13314, #21049, #29422, #2844, #23787, #13657, #254, #10739, #21217, #11242, #11079, #31994, #5924, #83, #16401, #13141, #21382, #21719, #8157, #24122, #16069, #26186, #10570, #5756, #31498, #21548, #2682, #31661, #29579, #16237, #8490, #23954, #761, #26855, #7990, #15899, #32164, #18475, #3351, #26525, #13821, #588, #8657, #5419, #19142, #15732, #29084, #18809, #23614, #29253, #28919, #18646, #26354, #5588, #26691, #3017, #13489, #424, #10910, #31827, #8320, #3187, #923, #29747, #9315, #22046, #27018, #8992, #32492, #6253, #3514, #32824, #24610, #11732, #8820, #25117, #1084, #16732, #3844, #22213, #32660, #11564, #27188, #30081, #27359, #14486, #19800, #32329, #4011, #9155, #19472, #29922, #6587, #4184, #19305, #13985, #16564, #14318, #30250, #6753, #17063, #1592, #17233, #19638, #21879, #1252, #3680, #27524, #22376, #24447, #24942, #6425, #16897, #24774, #27693, #1426, #14657, #6081, #14153, #11904, #12070, #22540, #32989, #9496, #19978, #11402, #28208, #9673, #17928, #12766, #7093, #25291, #28379, #20153, #30598, #33521, #17577, #28036, #4523, #33699, #20498, #7444, #4868, #4351, #15348, #17406, #17748, #10200, #14998, #10025, #22891, #6923, #14827, #25639, #1763, #30947, #30424, #25468, #27869, #25802, #23239, #2118, #12243, #31120, #1945, #12421, #22721, #33348, #7613, #12591, #33169, #9846, #20323, #2293, #30772, #7263, #20680, #4694, #15174, #23062, #17341, #21983, #27294, #22651, #29859, #27804, #3951, #4288, #12009, #19912, #16838, #22479, #30534, #6531, #30189, #30361, #19578, #6862, #1021, #17175, #7030, #32597, #8929, #14093, #17004, #33103, #1702, #32431, #3786, #14763, #9097, #24549, #30026, #27461, #14256, #11503, #25227, #11672, #32765, #6359, #12181, #22155, #24714, #24881, #9259, #19743, #14426, #1191, #27633, #1364, #1534, #9608, #19410, #25053, #6691, #11841, #22320, #4121, #20089, #14596, #32928, #3619, #9427, #27125, #7718, #18034, #2579, #20781, #31057, #33284, #12699, #15110, #23170, #33810, #14935, #28480, #30880, #22999, #25740, #18205, #4976, #28648, #17513, #17684, #23348, #15454, #7550, #33456, #33632, #5144, #10131, #20613, #28145, #31225, #26083, #25574, #22824, #15631, #4631, #2054, #25909, #12530, #9955, #20431, #13043, #12871, #10303, #23514, #1878, #33974, #25400, #2403, #10467, #7377, #20946, #17861, #27974, #12355, #31395, #9781, #4458, #20261, #28312, #30706, #7201, #4800, #15280, #2222, #13558, #8559, #8218, #18712, #24020, #24183, #16300, #18871, #824, #26590, #19043, #490, #29148, #656, #5654, #24353, #31727, #3249, #28987, #8056, #5486, #10973, #16136, #3086, #21447, #18374, #31890, #26253, #31558, #11305, #8386, #11144, #21287, #21783, #29320, #5822, #21614, #26757, #13887, #13719, #32059, #26916, #29481, #5985, #16462, #7885, #28819, #3413, #5317, #15797, #2741, #13205, #10807, #15965, #2915, #23681, #21115, #147, #10636, #18541, #26421, #13382, #23854, #320, #21203, #23435, #12961, #31146, #23772, #29071, #18119, #25828, #240, #7637, #28566, #18461, #5062, #15547, #25999, #16056, #15885, #2830, #10726, #4892, #31647, #17954, #26174, #26511, #33896, #28905, #20865, #30972, #15373, #10554, #2318, #26341, #7472, #2492, #411, #21035, #13299, #28739, #5575, #8145, #12791, #20705, #3004, #23265, #18634, #31311, #13477, #5406, #23942, #10225, #20529, #28403, #10387, #23601, #33727, #7805, #18294, #5235, #31485, #15719, #2668, #13127, #68, #7975, #31980, #909, #32149, #19289, #24596, #3175, #8806, #3499, #24274, #742, #11388, #8977, #13644, #31814, #21370, #8642, #14140, #1070, #21865, #29907, #11550, #24432, #26679, #6065, #8477, #16548, #27173, #8305, #32315, #11227, #16387, #19127, #22032, #29732, #32476, #10897, #11066, #16718, #6237, #3666, #26840, #5910, #19459, #13806, #3335, #21532, #6410, #16882, #18964, #16225, #27345, #29408, #21703, #3831, #29564, #27001, #13969, #14305, #24761, #18796, #29240, #5744, #24108, #576, #6911, #7248, #27681, #33156, #1580, #11717, #19624, #25277, #30069, #7080, #22200, #32810, #15160, #1750, #28021, #9482, #20308, #25453, #6575, #1414, #30758, #3999, #1929, #12057, #12407, #20140, #4509, #24929, #30584, #4681, #14645, #4338, #14983, #4171, #22877, #9141, #12230, #1239, #6741, #17049, #32647, #25104, #17735, #9831, #27511, #11892, #33334, #17222, #14472, #22527, #32978 ),
 ( #28193, #17564, #14812, #22363, #9303, #19965, #19787, #30236, #22704, #30411, #17392, #27856, #9659, #23565, #28366, #33858, #5198, #7600, #28869, #31608, #10684, #4854, #2629, #15508, #7768, #2454, #18255, #12920, #20483, #10012, #28701, #23048, #25960, #29, #15846, #10519, #21166, #13091, #15334, #31445, #7937, #18425, #15682, #23396, #25789, #5366, #13258, #5536, #26131, #31106, #31275, #18080, #23734, #5023, #20996, #12578, #10352, #20830, #26303, #33507, #2792, #198, #25626, #28528, #8106, #30934, #2105, #10183, #7427, #18593, #29033, #17914, #2278, #12753, #23225, #33684, #20665, #3133, #16017, #870, #16185, #21660, #16676, #16347, #26803, #32105, #32274, #24395, #26960, #8940, #704, #27132, #8604, #3298, #8767, #13763, #32439, #5869, #11350, #13606, #26639, #24072, #19087, #24233, #11190, #29526, #26471, #6029, #372, #5707, #19418, #16508, #19250, #29370, #29867, #18923, #3461, #10858, #2965, #537, #13433, #13931, #21828, #23901, #29690, #3627, #21333, #6196, #14101, #11024, #31774, #24557, #21494, #1031, #11511, #21991, #8266, #18758, #29202, #31942, #8434, #33777, #25541, #7516, #12494, #17648, #33596, #4596, #23312, #30668, #2187, #27941, #6997, #4424, #9919, #28109, #15073, #2019, #16846, #22963, #24723, #30496, #10268, #33421, #10096, #20228, #20750, #20396, #30847, #20575, #4766, #12838, #7338, #17823, #25873, #28280, #15244, #25706, #6368, #27302, #31019, #23130, #12661, #1667, #18001, #9742, #14899, #1841, #28446, #20051, #4937, #3793, #15419, #2365, #9574, #14266, #12142, #22791, #22615, #33068, #17479, #25363, #12321, #7166, #33244, #8025, #23822, #18511, #26049, #15595, #13349, #28611, #21083, #5623, #21417, #29120, #26726, #8190, #20909, #3054, #13525, #23988, #10776, #31532, #31360, #460, #18842, #11113, #288, #2712, #2883, #13173, #29288, #10605, #16107, #18169, #5453, #28957, #26558, #5111, #21253, #10942, #31193, #18680, #24153, #15934, #31860, #31697, #26390, #8353, #5788, #13689, #16269, #3221, #18340, #7852, #28785, #624, #7683, #2543, #13009, #23481, #33943, #10434, #5283, #15766, #26220, #23651, #113, #14518, #6286, #16762, #14351, #19506, #27556, #27221, #32524, #6619, #3714, #14184, #24640, #4044, #24977, #1286, #3878, #1114, #5955, #24808, #24480, #8691, #16597, #11599, #793, #27389, #1460, #19670, #29953, #24320, #29781, #22080, #3545, #11765, #21582, #17098, #11276, #9024, #11434, #6457, #32361, #16931, #8855, #16435, #26887, #22247, #19009, #21911, #32691, #9186, #30115, #32028, #8525, #21752, #29453, #3384, #13854, #32197, #19337, #19175, #29612, #6114, #27052, #14017, #954, #17606, #17439, #33554, #25324, #20356, #32855, #20184, #9704, #30803, #9351, #28068, #7296, #25836, #14858, #15034, #6787, #11938, #30458, #22407, #4555, #30628, #4899, #12277, #10054, #17265, #33201, #1979, #33025, #19833, #17781, #12103, #25499, #12623, #22750, #7125, #12454, #28239, #4724, #22924, #23091, #33380, #9876, #15205, #25669, #2148, #20535, #15380, #30979, #7479, #17960, #28409, #30286, #27728, #4216, #1799, #14690, #9530, #22574, #20011, #25149, #1625, #6955, #27901, #4383, #10563, #20711, #26007, #18803, #31492, #5583, #15726, #29247, #21042, #7982, #29078, #248, #8313, #18470, #13306, #21377, #28912, #5413, #15892, #5751, #16232, #16063, #18641, #26348, #31153, #26518, #5244, #23442, #31321, #2838, #15554, #8152, #2324, #418, #10733, #5070, #23781, #21210, #18301, #3012, #12798, #31822, #2500, #31655, #26181, #13484, #13134, #23949, #23608, #7644, #18130, #10905, #33734, #2676, #23271, #10231, #28574, #12968, #33903, #10394, #20873, #7812, #28746, #76, #27009, #16394, #29915, #14312, #6581, #8813, #32156, #32322, #8649, #24767, #6072, #1077, #13651, #916, #24439, #11557, #24116, #19296, #22039, #26686, #29571, #29740, #21539, #3182, #11234, #583, #6244, #11395, #19630, #3506, #1245, #31987, #13976, #16725, #13814, #11074, #32483, #26847, #27180, #19466, #21872, #11723, #16889, #8484, #3344, #22206, #29416, #27352, #3673, #3837, #8984, #6417, #24281, #32653, #30075, #16556, #14147, #9148, #19134, #18971, #5917, #24603, #749, #21710, #32817, #4005, #30417, #23054, #25632, #11898, #6747, #20315, #32984, #14478, #19971, #9488, #17227, #24935, #9837, #1587, #22712, #19794, #2111, #12063, #27687, #14819, #33162, #9665, #22534, #4177, #7086, #4344, #25460, #30764, #9309, #14990, #20146, #6916, #17398, #17570, #15166, #30242, #1420, #27518, #25284, #7254, #17741, #28028, #12584, #28201, #30590, #14651, #12236, #25111, #4515, #33340, #22370, #1935, #27862, #1756, #12413, #4687, #22883, #33513, #17056, #10018, #20489, #30940, #21001, #23403, #2460, #8111, #10357, #33864, #18086, #10691, #16022, #5029, #12759, #21172, #28534, #15515, #5371, #25966, #12926, #20835, #2970, #2797, #23739, #31614, #25795, #18598, #4860, #13097, #13440, #31280, #15852, #7773, #17921, #2284, #31450, #23231, #13264, #28372, #18260, #21338, #33691, #7943, #10190, #203, #15340, #28706, #7435, #18431, #29038, #15688, #26477, #5541, #20673, #7606, #23907, #31112, #378, #5204, #10864, #26308, #26137, #2634, #23570, #35, #10524, #28875, #1037, #24239, #24564, #5713, #21835, #1204, #3304, #13612, #18763, #11196, #3800, #6374, #26645, #21499, #11517, #13769, #29207, #710, #21667, #31947, #16191, #21997, #16354, #3467, #542, #16852, #26809, #8440, #29532, #13937, #24401, #32113, #18931, #32280, #19094, #6202, #32445, #24077, #29697, #877, #8611, #6035, #8773, #29874, #11030, #3139, #8271, #16514, #8946, #19424, #19256, #27309, #14272, #11357, #29377, #26966, #5876, #16682, #14107, #27139, #3633, #24729, #11685, #31779, #22838, #22667, #12370, #22169, #22333, #27988, #9622, #1717, #4135, #17189, #33298, #25066, #14610, #32778, #25416, #30721, #19756, #27477, #1894, #9272, #30205, #20103, #6707, #27647, #1547, #17699, #17527, #4475, #9798, #6544, #20274, #19591, #27819, #28159, #12023, #30549, #22492, #32613, #11854, #14950, #7216, #4645, #12196, #32943, #9444, #15125, #25588, #2068, #4302, #19928, #14777, #30374, #9110, #6875, #7045, #30039, #17355, #25242, #17017, #3966, #33119, #14439, #24894, #1380 ) ),
 .UNSPECIFIED., .F., .F., .T. ) 
 B_SPLINE_SURFACE_WITH_KNOTS ( ( 2, 2 ),
 ( 3, 2, 2, 2, 2, 2, 2, 2, 2, 2, 2, 2, 2, 2, 2, 2, 2, 2, 2, 2, 2, 2, 2, 2, 2, 2, 2, 2, 2, 2, 2, 2, 2, 2, 2, 2, 2, 2, 2, 2, 2, 2, 2, 2, 2, 2, 2, 2, 2, 2, 2, 2, 2, 2, 2, 2, 2, 2, 2, 2, 2, 2, 2, 2, 2, 2, 2, 2, 2, 2, 2, 2, 2, 2, 2, 2, 2, 2, 2, 2, 2, 2, 2, 2, 2, 2, 2, 2, 2, 2, 2, 2, 2, 2, 2, 2, 2, 2, 2, 2, 2, 2, 2, 2, 2, 2, 2, 2, 2, 2, 2, 2, 2, 2, 2, 2, 2, 2, 2, 2, 2, 2, 2, 2, 2, 2, 2, 2, 2, 2, 2, 2, 2, 2, 2, 2, 2, 2, 2, 2, 2, 2, 2, 2, 2, 2, 2, 2, 2, 2, 2, 2, 2, 2, 2, 2, 2, 2, 2, 2, 2, 2, 2, 2, 2, 2, 2, 2, 2, 2, 2, 2, 2, 2, 2, 2, 2, 2, 2, 2, 2, 2, 2, 2, 2, 2, 2, 2, 2, 2, 2, 2, 2, 2, 2, 2, 2, 2, 2, 2, 2, 2, 2, 2, 2, 2, 2, 2, 2, 2, 2, 2, 2, 2, 2, 2, 2, 2, 2, 2, 2, 2, 2, 2, 2, 2, 2, 2, 2, 2, 2, 2, 2, 2, 2, 2, 2, 2, 2, 2, 2, 2, 2, 2, 2, 2, 2, 2, 2, 2, 2, 2, 2, 2, 2, 2, 2, 2, 2, 2, 2, 2, 2, 2, 2, 2, 2, 2, 2, 2, 2, 2, 2, 2, 2, 2, 2, 2, 2, 2, 2, 2, 2, 2, 2, 2, 2, 2, 2, 2, 2, 2, 2, 2, 2, 2, 2, 2, 2, 2, 2, 2, 2, 2, 2, 2, 2, 2, 2, 2, 2, 2, 2, 2, 2, 2, 2, 2, 2, 2, 2, 2, 2, 2, 2, 2, 2, 2, 2, 2, 2, 2, 2, 2, 2, 2, 2, 2, 2, 2, 2, 2, 2, 2, 2, 2, 2, 2, 2, 2, 2, 2, 2, 2, 2, 2, 2, 2, 2, 2, 2, 2, 2, 2, 2, 2, 2, 2, 2, 2, 2, 2, 2, 2, 2, 2, 2, 2, 2, 2, 2, 2, 2, 2, 2, 2, 2, 2, 2, 2, 3 ),
 ( 0.000000000000000000, 1.000000000000000000 ),
 ( 0.000000000000000000, 0.002564102564102564100, 0.005128205128205128201, 0.007692307692307692735, 0.01025641025641025640, 0.01282051282051282007, 0.01538461538461538547, 0.01794871794871794740, 0.02051282051282051280, 0.02307692307692307820, 0.02564102564102564014, 0.02820512820512820554, 0.03076923076923077094, 0.03333333333333333287, 0.03589743589743589480, 0.03846153846153846367, 0.04102564102564102561, 0.04358974358974358754, 0.04615384615384615641, 0.04871794871794871834, 0.05128205128205128027, 0.05384615384615384914, 0.05641025641025641107, 0.05897435897435897301, 0.06153846153846154188, 0.06410256410256409687, 0.06666666666666666574, 0.06923076923076923461, 0.07179487179487178961, 0.07435897435897435848, 0.07692307692307692735, 0.07948717948717948234, 0.08205128205128205121, 0.08461538461538462008, 0.08717948717948717507, 0.08974358974358974395, 0.09230769230769231282, 0.09487179487179486781, 0.09743589743589743668, 0.1000000000000000056, 0.1025641025641025605, 0.1051282051282051294, 0.1076923076923076983, 0.1102564102564102533, 0.1128205128205128221, 0.1153846153846153910, 0.1179487179487179460, 0.1205128205128205149, 0.1230769230769230838, 0.1256410256410256387, 0.1282051282051281937, 0.1307692307692307765, 0.1333333333333333315, 0.1358974358974358865, 0.1384615384615384692, 0.1410256410256410242, 0.1435897435897435792, 0.1461538461538461620, 0.1487179487179487170, 0.1512820512820512719, 0.1538461538461538547, 0.1564102564102564097, 0.1589743589743589647, 0.1615384615384615474, 0.1641025641025641024, 0.1666666666666666574, 0.1692307692307692402, 0.1717948717948717952, 0.1743589743589743501, 0.1769230769230769329, 0.1794871794871794879, 0.1820512820512820429, 0.1846153846153846256, 0.1871794871794871806, 0.1897435897435897356, 0.1923076923076923184, 0.1948717948717948734, 0.1974358974358974284, 0.2000000000000000111, 0.2025641025641025661, 0.2051282051282051211, 0.2076923076923077038, 0.2102564102564102588, 0.2128205128205128138, 0.2153846153846153966, 0.2179487179487179516, 0.2205128205128205066, 0.2230769230769230893, 0.2256410256410256443, 0.2282051282051281993, 0.2307692307692307820, 0.2333333333333333370, 0.2358974358974358920, 0.2384615384615384748, 0.2410256410256410298, 0.2435897435897435848, 0.2461538461538461675, 0.2487179487179487225, 0.2512820512820512775, 0.2538461538461538325, 0.2564102564102563875, 0.2589743589743589980, 0.2615384615384615530, 0.2641025641025641080, 0.2666666666666666630, 0.2692307692307692180, 0.2717948717948717730, 0.2743589743589743835, 0.2769230769230769384, 0.2794871794871794934, 0.2820512820512820484, 0.2846153846153846034, 0.2871794871794871584, 0.2897435897435897689, 0.2923076923076923239, 0.2948717948717948789, 0.2974358974358974339, 0.2999999999999999889, 0.3025641025641025439, 0.3051282051282051544, 0.3076923076923077094, 0.3102564102564102644, 0.3128205128205128194, 0.3153846153846153744, 0.3179487179487179294, 0.3205128205128205399, 0.3230769230769230949, 0.3256410256410256499, 0.3282051282051282048, 0.3307692307692307598, 0.3333333333333333148, 0.3358974358974358698, 0.3384615384615384803, 0.3410256410256410353, 0.3435897435897435903, 0.3461538461538461453, 0.3487179487179487003, 0.3512820512820512553, 0.3538461538461538658, 0.3564102564102564208, 0.3589743589743589758, 0.3615384615384615308, 0.3641025641025640858, 0.3666666666666666408, 0.3692307692307692513, 0.3717948717948718063, 0.3743589743589743613, 0.3769230769230769162, 0.3794871794871794712, 0.3820512820512820262, 0.3846153846153846367, 0.3871794871794871917, 0.3897435897435897467, 0.3923076923076923017, 0.3948717948717948567, 0.3974358974358974117, 0.4000000000000000222, 0.4025641025641025772, 0.4051282051282051322, 0.4076923076923076872, 0.4102564102564102422, 0.4128205128205127972, 0.4153846153846154077, 0.4179487179487179627, 0.4205128205128205177, 0.4230769230769230727, 0.4256410256410256276, 0.4282051282051281826, 0.4307692307692307931, 0.4333333333333333481, 0.4358974358974359031, 0.4384615384615384581, 0.4410256410256410131, 0.4435897435897435681, 0.4461538461538461786, 0.4487179487179487336, 0.4512820512820512886, 0.4538461538461538436, 0.4564102564102563986, 0.4589743589743589536, 0.4615384615384615641, 0.4641025641025641191, 0.4666666666666666741, 0.4692307692307692291, 0.4717948717948717841, 0.4743589743589743390, 0.4769230769230769496, 0.4794871794871795045, 0.4820512820512820595, 0.4846153846153846145, 0.4871794871794871695, 0.4897435897435897245, 0.4923076923076923350, 0.4948717948717948900, 0.4974358974358974450, 0.5000000000000000000, 0.5025641025641025550, 0.5051282051282051100, 0.5076923076923076650, 0.5102564102564102200, 0.5128205128205127750, 0.5153846153846153300, 0.5179487179487179960, 0.5205128205128205510, 0.5230769230769231060, 0.5256410256410256610, 0.5282051282051282159, 0.5307692307692307709, 0.5333333333333333259, 0.5358974358974358809, 0.5384615384615384359, 0.5410256410256409909, 0.5435897435897435459, 0.5461538461538461009, 0.5487179487179487669, 0.5512820512820513219, 0.5538461538461538769, 0.5564102564102564319, 0.5589743589743589869, 0.5615384615384615419, 0.5641025641025640969, 0.5666666666666666519, 0.5692307692307692069, 0.5717948717948717618, 0.5743589743589743168, 0.5769230769230768718, 0.5794871794871795379, 0.5820512820512820928, 0.5846153846153846478, 0.5871794871794872028, 0.5897435897435897578, 0.5923076923076923128, 0.5948717948717948678, 0.5974358974358974228, 0.5999999999999999778, 0.6025641025641025328, 0.6051282051282050878, 0.6076923076923076428, 0.6102564102564103088, 0.6128205128205128638, 0.6153846153846154188, 0.6179487179487179738, 0.6205128205128205288, 0.6230769230769230838, 0.6256410256410256387, 0.6282051282051281937, 0.6307692307692307487, 0.6333333333333333037, 0.6358974358974358587, 0.6384615384615384137, 0.6410256410256410797, 0.6435897435897436347, 0.6461538461538461897, 0.6487179487179487447, 0.6512820512820512997, 0.6538461538461538547, 0.6564102564102564097, 0.6589743589743589647, 0.6615384615384615197, 0.6641025641025640747, 0.6666666666666666297, 0.6692307692307691847, 0.6717948717948717396, 0.6743589743589744057, 0.6769230769230769607, 0.6794871794871795156, 0.6820512820512820706, 0.6846153846153846256, 0.6871794871794871806, 0.6897435897435897356, 0.6923076923076922906, 0.6948717948717948456, 0.6974358974358974006, 0.6999999999999999556, 0.7025641025641025106, 0.7051282051282051766, 0.7076923076923077316, 0.7102564102564102866, 0.7128205128205128416, 0.7153846153846153966, 0.7179487179487179516, 0.7205128205128205066, 0.7230769230769230616, 0.7256410256410256165, 0.7282051282051281715, 0.7307692307692307265, 0.7333333333333332815, 0.7358974358974359475, 0.7384615384615385025, 0.7410256410256410575, 0.7435897435897436125, 0.7461538461538461675, 0.7487179487179487225, 0.7512820512820512775, 0.7538461538461538325, 0.7564102564102563875, 0.7589743589743589425, 0.7615384615384614975, 0.7641025641025640525, 0.7666666666666667185, 0.7692307692307692735, 0.7717948717948718285, 0.7743589743589743835, 0.7769230769230769384, 0.7794871794871794934, 0.7820512820512820484, 0.7846153846153846034, 0.7871794871794871584, 0.7897435897435897134, 0.7923076923076922684, 0.7948717948717948234, 0.7974358974358974894, 0.8000000000000000444, 0.8025641025641025994, 0.8051282051282051544, 0.8076923076923077094, 0.8102564102564102644, 0.8128205128205128194, 0.8153846153846153744, 0.8179487179487179294, 0.8205128205128204844, 0.8230769230769230393, 0.8256410256410255943, 0.8282051282051282604, 0.8307692307692308153, 0.8333333333333333703, 0.8358974358974359253, 0.8384615384615384803, 0.8410256410256410353, 0.8435897435897435903, 0.8461538461538461453, 0.8487179487179487003, 0.8512820512820512553, 0.8538461538461538103, 0.8564102564102563653, 0.8589743589743589203, 0.8615384615384615863, 0.8641025641025641413, 0.8666666666666666963, 0.8692307692307692513, 0.8717948717948718063, 0.8743589743589743613, 0.8769230769230769162, 0.8794871794871794712, 0.8820512820512820262, 0.8846153846153845812, 0.8871794871794871362, 0.8897435897435896912, 0.8923076923076923572, 0.8948717948717949122, 0.8974358974358974672, 0.9000000000000000222, 0.9025641025641025772, 0.9051282051282051322, 0.9076923076923076872, 0.9102564102564102422, 0.9128205128205127972, 0.9153846153846153522, 0.9179487179487179072, 0.9205128205128204621, 0.9230769230769231282, 0.9256410256410256832, 0.9282051282051282382, 0.9307692307692307931, 0.9333333333333333481, 0.9358974358974359031, 0.9384615384615384581, 0.9410256410256410131, 0.9435897435897435681, 0.9461538461538461231, 0.9487179487179486781, 0.9512820512820512331, 0.9538461538461538991, 0.9564102564102564541, 0.9589743589743590091, 0.9615384615384615641, 0.9641025641025641191, 0.9666666666666666741, 0.9692307692307692291, 0.9717948717948717841, 0.9743589743589743390, 0.9769230769230768940, 0.9794871794871794490, 0.9820512820512820040, 0.9846153846153846700, 0.9871794871794872250, 0.9897435897435897800, 0.9923076923076923350, 0.9948717948717948900, 0.9974358974358974450, 1.000000000000000000 ),
 .UNSPECIFIED. ) 
 GEOMETRIC_REPRESENTATION_ITEM ( )  RATIONAL_B_SPLINE_SURFACE ( (
 ( 1.000000000000000000, 0.9510565162951535312, 1.000000000000000000, 0.9510565162951535312, 1.000000000000000000, 0.9510565162951535312, 1.000000000000000000, 0.9510565162951535312, 1.000000000000000000, 0.9510565162951535312, 1.000000000000000000, 0.9510565162951535312, 1.000000000000000000, 0.9510565162951535312, 1.000000000000000000, 0.9510565162951535312, 1.000000000000000000, 0.9510565162951535312, 1.000000000000000000, 0.9510565162951535312, 1.000000000000000000, 0.9510565162951535312, 1.000000000000000000, 0.9510565162951535312, 1.000000000000000000, 0.9510565162951535312, 1.000000000000000000, 0.9510565162951535312, 1.000000000000000000, 0.9510565162951535312, 1.000000000000000000, 0.9510565162951535312, 1.000000000000000000, 0.9510565162951535312, 1.000000000000000000, 0.9510565162951535312, 1.000000000000000000, 0.9510565162951535312, 1.000000000000000000, 0.9510565162951535312, 1.000000000000000000, 0.9510565162951535312, 1.000000000000000000, 0.9510565162951535312, 1.000000000000000000, 0.9510565162951535312, 1.000000000000000000, 0.9510565162951535312, 1.000000000000000000, 0.9510565162951535312, 1.000000000000000000, 0.9510565162951535312, 1.000000000000000000, 0.9510565162951535312, 1.000000000000000000, 0.9510565162951535312, 1.000000000000000000, 0.9510565162951535312, 1.000000000000000000, 0.9510565162951535312, 1.000000000000000000, 0.9510565162951535312, 1.000000000000000000, 0.9510565162951535312, 1.000000000000000000, 0.9510565162951535312, 1.000000000000000000, 0.9510565162951535312, 1.000000000000000000, 0.9510565162951535312, 1.000000000000000000, 0.9510565162951535312, 1.000000000000000000, 0.9510565162951535312, 1.000000000000000000, 0.9510565162951535312, 1.000000000000000000, 0.9510565162951535312, 1.000000000000000000, 0.9510565162951535312, 1.000000000000000000, 0.9510565162951535312, 1.000000000000000000, 0.9510565162951535312, 1.000000000000000000, 0.9510565162951535312, 1.000000000000000000, 0.9510565162951535312, 1.000000000000000000, 0.9510565162951535312, 1.000000000000000000, 0.9510565162951535312, 1.000000000000000000, 0.9510565162951535312, 1.000000000000000000, 0.9510565162951535312, 1.000000000000000000, 0.9510565162951535312, 1.000000000000000000, 0.9510565162951535312, 1.000000000000000000, 0.9510565162951535312, 1.000000000000000000, 0.9510565162951535312, 1.000000000000000000, 0.9510565162951535312, 1.000000000000000000, 0.9510565162951535312, 1.000000000000000000, 0.9510565162951535312, 1.000000000000000000, 0.9510565162951535312, 1.000000000000000000, 0.9510565162951535312, 1.000000000000000000, 0.9510565162951535312, 1.000000000000000000, 0.9510565162951535312, 1.000000000000000000, 0.9510565162951535312, 1.000000000000000000, 0.9510565162951535312, 1.000000000000000000, 0.9510565162951535312, 1.000000000000000000, 0.9510565162951535312, 1.000000000000000000, 0.9510565162951535312, 1.000000000000000000, 0.9510565162951535312, 1.000000000000000000, 0.9510565162951535312, 1.000000000000000000, 0.9510565162951535312, 1.000000000000000000, 0.9510565162951535312, 1.000000000000000000, 0.9510565162951535312, 1.000000000000000000, 0.9510565162951535312, 1.000000000000000000, 0.9510565162951535312, 1.000000000000000000, 0.9510565162951535312, 1.000000000000000000, 0.9510565162951535312, 1.000000000000000000, 0.9510565162951535312, 1.000000000000000000, 0.9510565162951535312, 1.000000000000000000, 0.9510565162951535312, 1.000000000000000000, 0.9510565162951535312, 1.000000000000000000, 0.9510565162951535312, 1.000000000000000000, 0.9510565162951535312, 1.000000000000000000, 0.9510565162951535312, 1.000000000000000000, 0.9510565162951535312, 1.000000000000000000, 0.9510565162951535312, 1.000000000000000000, 0.9510565162951535312, 1.000000000000000000, 0.9510565162951535312, 1.000000000000000000, 0.9510565162951535312, 1.000000000000000000, 0.9510565162951535312, 1.000000000000000000, 0.9510565162951535312, 1.000000000000000000, 0.9510565162951535312, 1.000000000000000000, 0.9510565162951535312, 1.000000000000000000, 0.9510565162951535312, 1.000000000000000000, 0.9510565162951535312, 1.000000000000000000, 0.9510565162951535312, 1.000000000000000000, 0.9510565162951535312, 1.000000000000000000, 0.9510565162951535312, 1.000000000000000000, 0.9510565162951535312, 1.000000000000000000, 0.9510565162951535312, 1.000000000000000000, 0.9510565162951535312, 1.000000000000000000, 0.9510565162951535312, 1.000000000000000000, 0.9510565162951535312, 1.000000000000000000, 0.9510565162951535312, 1.000000000000000000, 0.9510565162951535312, 1.000000000000000000, 0.9510565162951535312, 1.000000000000000000, 0.9510565162951535312, 1.000000000000000000, 0.9510565162951535312, 1.000000000000000000, 0.9510565162951535312, 1.000000000000000000, 0.9510565162951535312, 1.000000000000000000, 0.9510565162951535312, 1.000000000000000000, 0.9510565162951535312, 1.000000000000000000, 0.9510565162951535312, 1.000000000000000000, 0.9510565162951535312, 1.000000000000000000, 0.9510565162951535312, 1.000000000000000000, 0.9510565162951535312, 1.000000000000000000, 0.9510565162951535312, 1.000000000000000000, 0.9510565162951535312, 1.000000000000000000, 0.9510565162951535312, 1.000000000000000000, 0.9510565162951535312, 1.000000000000000000, 0.9510565162951535312, 1.000000000000000000, 0.9510565162951535312, 1.000000000000000000, 0.9510565162951535312, 1.000000000000000000, 0.9510565162951535312, 1.000000000000000000, 0.9510565162951535312, 1.000000000000000000, 0.9510565162951535312, 1.000000000000000000, 0.9510565162951535312, 1.000000000000000000, 0.9510565162951535312, 1.000000000000000000, 0.9510565162951535312, 1.000000000000000000, 0.9510565162951535312, 1.000000000000000000, 0.9510565162951535312, 1.000000000000000000, 0.9510565162951535312, 1.000000000000000000, 0.9510565162951535312, 1.000000000000000000, 0.9510565162951535312, 1.000000000000000000, 0.9510565162951535312, 1.000000000000000000, 0.9510565162951535312, 1.000000000000000000, 0.9510565162951535312, 1.000000000000000000, 0.9510565162951535312, 1.000000000000000000, 0.9510565162951535312, 1.000000000000000000, 0.9510565162951535312, 1.000000000000000000, 0.9510565162951535312, 1.000000000000000000, 0.9510565162951535312, 1.000000000000000000, 0.9510565162951535312, 1.000000000000000000, 0.9510565162951535312, 1.000000000000000000, 0.9510565162951535312, 1.000000000000000000, 0.9510565162951535312, 1.000000000000000000, 0.9510565162951535312, 1.000000000000000000, 0.9510565162951535312, 1.000000000000000000, 0.9510565162951535312, 1.000000000000000000, 0.9510565162951535312, 1.000000000000000000, 0.9510565162951535312, 1.000000000000000000, 0.9510565162951535312, 1.000000000000000000, 0.9510565162951535312, 1.000000000000000000, 0.9510565162951535312, 1.000000000000000000, 0.9510565162951535312, 1.000000000000000000, 0.9510565162951535312, 1.000000000000000000, 0.9510565162951535312, 1.000000000000000000, 0.9510565162951535312, 1.000000000000000000, 0.9510565162951535312, 1.000000000000000000, 0.9510565162951535312, 1.000000000000000000, 0.9510565162951535312, 1.000000000000000000, 0.9510565162951535312, 1.000000000000000000, 0.9510565162951535312, 1.000000000000000000, 0.9510565162951535312, 1.000000000000000000, 0.9510565162951535312, 1.000000000000000000, 0.9510565162951535312, 1.000000000000000000, 0.9510565162951535312, 1.000000000000000000, 0.9510565162951535312, 1.000000000000000000, 0.9510565162951535312, 1.000000000000000000, 0.9510565162951535312, 1.000000000000000000, 0.9510565162951535312, 1.000000000000000000, 0.9510565162951535312, 1.000000000000000000, 0.9510565162951535312, 1.000000000000000000, 0.9510565162951535312, 1.000000000000000000, 0.9510565162951535312, 1.000000000000000000, 0.9510565162951535312, 1.000000000000000000, 0.9510565162951535312, 1.000000000000000000, 0.9510565162951535312, 1.000000000000000000, 0.9510565162951535312, 1.000000000000000000, 0.9510565162951535312, 1.000000000000000000, 0.9510565162951535312, 1.000000000000000000, 0.9510565162951535312, 1.000000000000000000, 0.9510565162951535312, 1.000000000000000000, 0.9510565162951535312, 1.000000000000000000, 0.9510565162951535312, 1.000000000000000000, 0.9510565162951535312, 1.000000000000000000, 0.9510565162951535312, 1.000000000000000000, 0.9510565162951535312, 1.000000000000000000, 0.9510565162951535312, 1.000000000000000000, 0.9510565162951535312, 1.000000000000000000, 0.9510565162951535312, 1.000000000000000000, 0.9510565162951535312, 1.000000000000000000, 0.9510565162951535312, 1.000000000000000000, 0.9510565162951535312, 1.000000000000000000, 0.9510565162951535312, 1.000000000000000000, 0.9510565162951535312, 1.000000000000000000, 0.9510565162951535312, 1.000000000000000000, 0.9510565162951535312, 1.000000000000000000, 0.9510565162951535312, 1.000000000000000000, 0.9510565162951535312, 1.000000000000000000, 0.9510565162951535312, 1.000000000000000000, 0.9510565162951535312, 1.000000000000000000, 0.9510565162951535312, 1.000000000000000000, 0.9510565162951535312, 1.000000000000000000, 0.9510565162951535312, 1.000000000000000000, 0.9510565162951535312, 1.000000000000000000, 0.9510565162951535312, 1.000000000000000000, 0.9510565162951535312, 1.000000000000000000, 0.9510565162951535312, 1.000000000000000000, 0.9510565162951535312, 1.000000000000000000, 0.9510565162951535312, 1.000000000000000000, 0.9510565162951535312, 1.000000000000000000, 0.9510565162951535312, 1.000000000000000000, 0.9510565162951535312, 1.000000000000000000, 0.9510565162951535312, 1.000000000000000000, 0.9510565162951535312, 1.000000000000000000, 0.9510565162951535312, 1.000000000000000000, 0.9510565162951535312, 1.000000000000000000, 0.9510565162951535312, 1.000000000000000000, 0.9510565162951535312, 1.000000000000000000, 0.9510565162951535312, 1.000000000000000000, 0.9510565162951535312, 1.000000000000000000, 0.9510565162951535312, 1.000000000000000000, 0.9510565162951535312, 1.000000000000000000, 0.9510565162951535312, 1.000000000000000000, 0.9510565162951535312, 1.000000000000000000, 0.9510565162951535312, 1.000000000000000000, 0.9510565162951535312, 1.000000000000000000, 0.9510565162951535312, 1.000000000000000000, 0.9510565162951535312, 1.000000000000000000, 0.9510565162951535312, 1.000000000000000000, 0.9510565162951535312, 1.000000000000000000, 0.9510565162951535312, 1.000000000000000000, 0.9510565162951535312, 1.000000000000000000, 0.9510565162951535312, 1.000000000000000000, 0.9510565162951535312, 1.000000000000000000, 0.9510565162951535312, 1.000000000000000000, 0.9510565162951535312, 1.000000000000000000, 0.9510565162951535312, 1.000000000000000000, 0.9510565162951535312, 1.000000000000000000, 0.9510565162951535312, 1.000000000000000000, 0.9510565162951535312, 1.000000000000000000, 0.9510565162951535312, 1.000000000000000000, 0.9510565162951535312, 1.000000000000000000, 0.9510565162951535312, 1.000000000000000000, 0.9510565162951535312, 1.000000000000000000, 0.9510565162951535312, 1.000000000000000000, 0.9510565162951535312, 1.000000000000000000, 0.9510565162951535312, 1.000000000000000000, 0.9510565162951535312, 1.000000000000000000, 0.9510565162951535312, 1.000000000000000000, 0.9510565162951535312, 1.000000000000000000, 0.9510565162951535312, 1.000000000000000000, 0.9510565162951535312, 1.000000000000000000, 0.9510565162951535312, 1.000000000000000000, 0.9510565162951535312, 1.000000000000000000, 0.9510565162951535312, 1.000000000000000000, 0.9510565162951535312, 1.000000000000000000, 0.9510565162951535312, 1.000000000000000000, 0.9510565162951535312, 1.000000000000000000, 0.9510565162951535312, 1.000000000000000000, 0.9510565162951535312, 1.000000000000000000, 0.9510565162951535312, 1.000000000000000000, 0.9510565162951535312, 1.000000000000000000, 0.9510565162951535312, 1.000000000000000000, 0.9510565162951535312, 1.000000000000000000, 0.9510565162951535312, 1.000000000000000000, 0.9510565162951535312, 1.000000000000000000, 0.9510565162951535312, 1.000000000000000000, 0.9510565162951535312, 1.000000000000000000, 0.9510565162951535312, 1.000000000000000000, 0.9510565162951535312, 1.000000000000000000, 0.9510565162951535312, 1.000000000000000000, 0.9510565162951535312, 1.000000000000000000, 0.9510565162951535312, 1.000000000000000000, 0.9510565162951535312, 1.000000000000000000, 0.9510565162951535312, 1.000000000000000000, 0.9510565162951535312, 1.000000000000000000, 0.9510565162951535312, 1.000000000000000000, 0.9510565162951535312, 1.000000000000000000, 0.9510565162951535312, 1.000000000000000000, 0.9510565162951535312, 1.000000000000000000, 0.9510565162951535312, 1.000000000000000000, 0.9510565162951535312, 1.000000000000000000, 0.9510565162951535312, 1.000000000000000000, 0.9510565162951535312, 1.000000000000000000, 0.9510565162951535312, 1.000000000000000000, 0.9510565162951535312, 1.000000000000000000, 0.9510565162951535312, 1.000000000000000000, 0.9510565162951535312, 1.000000000000000000, 0.9510565162951535312, 1.000000000000000000, 0.9510565162951535312, 1.000000000000000000, 0.9510565162951535312, 1.000000000000000000, 0.9510565162951535312, 1.000000000000000000, 0.9510565162951535312, 1.000000000000000000, 0.9510565162951535312, 1.000000000000000000, 0.9510565162951535312, 1.000000000000000000, 0.9510565162951535312, 1.000000000000000000, 0.9510565162951535312, 1.000000000000000000, 0.9510565162951535312, 1.000000000000000000, 0.9510565162951535312, 1.000000000000000000, 0.9510565162951535312, 1.000000000000000000, 0.9510565162951535312, 1.000000000000000000, 0.9510565162951535312, 1.000000000000000000, 0.9510565162951535312, 1.000000000000000000, 0.9510565162951535312, 1.000000000000000000, 0.9510565162951535312, 1.000000000000000000, 0.9510565162951535312, 1.000000000000000000, 0.9510565162951535312, 1.000000000000000000, 0.9510565162951535312, 1.000000000000000000, 0.9510565162951535312, 1.000000000000000000, 0.9510565162951535312, 1.000000000000000000, 0.9510565162951535312, 1.000000000000000000, 0.9510565162951535312, 1.000000000000000000, 0.9510565162951535312, 1.000000000000000000, 0.9510565162951535312, 1.000000000000000000, 0.9510565162951535312, 1.000000000000000000, 0.9510565162951535312, 1.000000000000000000, 0.9510565162951535312, 1.000000000000000000, 0.9510565162951535312, 1.000000000000000000, 0.9510565162951535312, 1.000000000000000000, 0.9510565162951535312, 1.000000000000000000, 0.9510565162951535312, 1.000000000000000000, 0.9510565162951535312, 1.000000000000000000, 0.9510565162951535312, 1.000000000000000000, 0.9510565162951535312, 1.000000000000000000, 0.9510565162951535312, 1.000000000000000000, 0.9510565162951535312, 1.000000000000000000, 0.9510565162951535312, 1.000000000000000000, 0.9510565162951535312, 1.000000000000000000, 0.9510565162951535312, 1.000000000000000000, 0.9510565162951535312, 1.000000000000000000, 0.9510565162951535312, 1.000000000000000000, 0.9510565162951535312, 1.000000000000000000, 0.9510565162951535312, 1.000000000000000000, 0.9510565162951535312, 1.000000000000000000, 0.9510565162951535312, 1.000000000000000000, 0.9510565162951535312, 1.000000000000000000, 0.9510565162951535312, 1.000000000000000000, 0.9510565162951535312, 1.000000000000000000, 0.9510565162951535312, 1.000000000000000000, 0.9510565162951535312, 1.000000000000000000, 0.9510565162951535312, 1.000000000000000000, 0.9510565162951535312, 1.000000000000000000, 0.9510565162951535312, 1.000000000000000000, 0.9510565162951535312, 1.000000000000000000, 0.9510565162951535312, 1.000000000000000000, 0.9510565162951535312, 1.000000000000000000, 0.9510565162951535312, 1.000000000000000000, 0.9510565162951535312, 1.000000000000000000, 0.9510565162951535312, 1.000000000000000000, 0.9510565162951535312, 1.000000000000000000, 0.9510565162951535312, 1.000000000000000000, 0.9510565162951535312, 1.000000000000000000, 0.9510565162951535312, 1.000000000000000000, 0.9510565162951535312, 1.000000000000000000, 0.9510565162951535312, 1.000000000000000000, 0.9510565162951535312, 1.000000000000000000, 0.9510565162951535312, 1.000000000000000000, 0.9510565162951535312, 1.000000000000000000, 0.9510565162951535312, 1.000000000000000000, 0.9510565162951535312, 1.000000000000000000, 0.9510565162951535312, 1.000000000000000000, 0.9510565162951535312, 1.000000000000000000, 0.9510565162951535312, 1.000000000000000000, 0.9510565162951535312, 1.000000000000000000, 0.9510565162951535312, 1.000000000000000000, 0.9510565162951535312, 1.000000000000000000, 0.9510565162951535312, 1.000000000000000000, 0.9510565162951535312, 1.000000000000000000, 0.9510565162951535312, 1.000000000000000000, 0.9510565162951535312, 1.000000000000000000, 0.9510565162951535312, 1.000000000000000000, 0.9510565162951535312, 1.000000000000000000, 0.9510565162951535312, 1.000000000000000000, 0.9510565162951535312, 1.000000000000000000, 0.9510565162951535312, 1.000000000000000000, 0.9510565162951535312, 1.000000000000000000, 0.9510565162951535312, 1.000000000000000000, 0.9510565162951535312, 1.000000000000000000, 0.9510565162951535312, 1.000000000000000000, 0.9510565162951535312, 1.000000000000000000, 0.9510565162951535312, 1.000000000000000000, 0.9510565162951535312, 1.000000000000000000, 0.9510565162951535312, 1.000000000000000000, 0.9510565162951535312, 1.000000000000000000, 0.9510565162951535312, 1.000000000000000000, 0.9510565162951535312, 1.000000000000000000, 0.9510565162951535312, 1.000000000000000000, 0.9510565162951535312, 1.000000000000000000, 0.9510565162951535312, 1.000000000000000000, 0.9510565162951535312, 1.000000000000000000, 0.9510565162951535312, 1.000000000000000000, 0.9510565162951535312, 1.000000000000000000),
 ( 1.000000000000000000, 0.9510565162951535312, 1.000000000000000000, 0.9510565162951535312, 1.000000000000000000, 0.9510565162951535312, 1.000000000000000000, 0.9510565162951535312, 1.000000000000000000, 0.9510565162951535312, 1.000000000000000000, 0.9510565162951535312, 1.000000000000000000, 0.9510565162951535312, 1.000000000000000000, 0.9510565162951535312, 1.000000000000000000, 0.9510565162951535312, 1.000000000000000000, 0.9510565162951535312, 1.000000000000000000, 0.9510565162951535312, 1.000000000000000000, 0.9510565162951535312, 1.000000000000000000, 0.9510565162951535312, 1.000000000000000000, 0.9510565162951535312, 1.000000000000000000, 0.9510565162951535312, 1.000000000000000000, 0.9510565162951535312, 1.000000000000000000, 0.9510565162951535312, 1.000000000000000000, 0.9510565162951535312, 1.000000000000000000, 0.9510565162951535312, 1.000000000000000000, 0.9510565162951535312, 1.000000000000000000, 0.9510565162951535312, 1.000000000000000000, 0.9510565162951535312, 1.000000000000000000, 0.9510565162951535312, 1.000000000000000000, 0.9510565162951535312, 1.000000000000000000, 0.9510565162951535312, 1.000000000000000000, 0.9510565162951535312, 1.000000000000000000, 0.9510565162951535312, 1.000000000000000000, 0.9510565162951535312, 1.000000000000000000, 0.9510565162951535312, 1.000000000000000000, 0.9510565162951535312, 1.000000000000000000, 0.9510565162951535312, 1.000000000000000000, 0.9510565162951535312, 1.000000000000000000, 0.9510565162951535312, 1.000000000000000000, 0.9510565162951535312, 1.000000000000000000, 0.9510565162951535312, 1.000000000000000000, 0.9510565162951535312, 1.000000000000000000, 0.9510565162951535312, 1.000000000000000000, 0.9510565162951535312, 1.000000000000000000, 0.9510565162951535312, 1.000000000000000000, 0.9510565162951535312, 1.000000000000000000, 0.9510565162951535312, 1.000000000000000000, 0.9510565162951535312, 1.000000000000000000, 0.9510565162951535312, 1.000000000000000000, 0.9510565162951535312, 1.000000000000000000, 0.9510565162951535312, 1.000000000000000000, 0.9510565162951535312, 1.000000000000000000, 0.9510565162951535312, 1.000000000000000000, 0.9510565162951535312, 1.000000000000000000, 0.9510565162951535312, 1.000000000000000000, 0.9510565162951535312, 1.000000000000000000, 0.9510565162951535312, 1.000000000000000000, 0.9510565162951535312, 1.000000000000000000, 0.9510565162951535312, 1.000000000000000000, 0.9510565162951535312, 1.000000000000000000, 0.9510565162951535312, 1.000000000000000000, 0.9510565162951535312, 1.000000000000000000, 0.9510565162951535312, 1.000000000000000000, 0.9510565162951535312, 1.000000000000000000, 0.9510565162951535312, 1.000000000000000000, 0.9510565162951535312, 1.000000000000000000, 0.9510565162951535312, 1.000000000000000000, 0.9510565162951535312, 1.000000000000000000, 0.9510565162951535312, 1.000000000000000000, 0.9510565162951535312, 1.000000000000000000, 0.9510565162951535312, 1.000000000000000000, 0.9510565162951535312, 1.000000000000000000, 0.9510565162951535312, 1.000000000000000000, 0.9510565162951535312, 1.000000000000000000, 0.9510565162951535312, 1.000000000000000000, 0.9510565162951535312, 1.000000000000000000, 0.9510565162951535312, 1.000000000000000000, 0.9510565162951535312, 1.000000000000000000, 0.9510565162951535312, 1.000000000000000000, 0.9510565162951535312, 1.000000000000000000, 0.9510565162951535312, 1.000000000000000000, 0.9510565162951535312, 1.000000000000000000, 0.9510565162951535312, 1.000000000000000000, 0.9510565162951535312, 1.000000000000000000, 0.9510565162951535312, 1.000000000000000000, 0.9510565162951535312, 1.000000000000000000, 0.9510565162951535312, 1.000000000000000000, 0.9510565162951535312, 1.000000000000000000, 0.9510565162951535312, 1.000000000000000000, 0.9510565162951535312, 1.000000000000000000, 0.9510565162951535312, 1.000000000000000000, 0.9510565162951535312, 1.000000000000000000, 0.9510565162951535312, 1.000000000000000000, 0.9510565162951535312, 1.000000000000000000, 0.9510565162951535312, 1.000000000000000000, 0.9510565162951535312, 1.000000000000000000, 0.9510565162951535312, 1.000000000000000000, 0.9510565162951535312, 1.000000000000000000, 0.9510565162951535312, 1.000000000000000000, 0.9510565162951535312, 1.000000000000000000, 0.9510565162951535312, 1.000000000000000000, 0.9510565162951535312, 1.000000000000000000, 0.9510565162951535312, 1.000000000000000000, 0.9510565162951535312, 1.000000000000000000, 0.9510565162951535312, 1.000000000000000000, 0.9510565162951535312, 1.000000000000000000, 0.9510565162951535312, 1.000000000000000000, 0.9510565162951535312, 1.000000000000000000, 0.9510565162951535312, 1.000000000000000000, 0.9510565162951535312, 1.000000000000000000, 0.9510565162951535312, 1.000000000000000000, 0.9510565162951535312, 1.000000000000000000, 0.9510565162951535312, 1.000000000000000000, 0.9510565162951535312, 1.000000000000000000, 0.9510565162951535312, 1.000000000000000000, 0.9510565162951535312, 1.000000000000000000, 0.9510565162951535312, 1.000000000000000000, 0.9510565162951535312, 1.000000000000000000, 0.9510565162951535312, 1.000000000000000000, 0.9510565162951535312, 1.000000000000000000, 0.9510565162951535312, 1.000000000000000000, 0.9510565162951535312, 1.000000000000000000, 0.9510565162951535312, 1.000000000000000000, 0.9510565162951535312, 1.000000000000000000, 0.9510565162951535312, 1.000000000000000000, 0.9510565162951535312, 1.000000000000000000, 0.9510565162951535312, 1.000000000000000000, 0.9510565162951535312, 1.000000000000000000, 0.9510565162951535312, 1.000000000000000000, 0.9510565162951535312, 1.000000000000000000, 0.9510565162951535312, 1.000000000000000000, 0.9510565162951535312, 1.000000000000000000, 0.9510565162951535312, 1.000000000000000000, 0.9510565162951535312, 1.000000000000000000, 0.9510565162951535312, 1.000000000000000000, 0.9510565162951535312, 1.000000000000000000, 0.9510565162951535312, 1.000000000000000000, 0.9510565162951535312, 1.000000000000000000, 0.9510565162951535312, 1.000000000000000000, 0.9510565162951535312, 1.000000000000000000, 0.9510565162951535312, 1.000000000000000000, 0.9510565162951535312, 1.000000000000000000, 0.9510565162951535312, 1.000000000000000000, 0.9510565162951535312, 1.000000000000000000, 0.9510565162951535312, 1.000000000000000000, 0.9510565162951535312, 1.000000000000000000, 0.9510565162951535312, 1.000000000000000000, 0.9510565162951535312, 1.000000000000000000, 0.9510565162951535312, 1.000000000000000000, 0.9510565162951535312, 1.000000000000000000, 0.9510565162951535312, 1.000000000000000000, 0.9510565162951535312, 1.000000000000000000, 0.9510565162951535312, 1.000000000000000000, 0.9510565162951535312, 1.000000000000000000, 0.9510565162951535312, 1.000000000000000000, 0.9510565162951535312, 1.000000000000000000, 0.9510565162951535312, 1.000000000000000000, 0.9510565162951535312, 1.000000000000000000, 0.9510565162951535312, 1.000000000000000000, 0.9510565162951535312, 1.000000000000000000, 0.9510565162951535312, 1.000000000000000000, 0.9510565162951535312, 1.000000000000000000, 0.9510565162951535312, 1.000000000000000000, 0.9510565162951535312, 1.000000000000000000, 0.9510565162951535312, 1.000000000000000000, 0.9510565162951535312, 1.000000000000000000, 0.9510565162951535312, 1.000000000000000000, 0.9510565162951535312, 1.000000000000000000, 0.9510565162951535312, 1.000000000000000000, 0.9510565162951535312, 1.000000000000000000, 0.9510565162951535312, 1.000000000000000000, 0.9510565162951535312, 1.000000000000000000, 0.9510565162951535312, 1.000000000000000000, 0.9510565162951535312, 1.000000000000000000, 0.9510565162951535312, 1.000000000000000000, 0.9510565162951535312, 1.000000000000000000, 0.9510565162951535312, 1.000000000000000000, 0.9510565162951535312, 1.000000000000000000, 0.9510565162951535312, 1.000000000000000000, 0.9510565162951535312, 1.000000000000000000, 0.9510565162951535312, 1.000000000000000000, 0.9510565162951535312, 1.000000000000000000, 0.9510565162951535312, 1.000000000000000000, 0.9510565162951535312, 1.000000000000000000, 0.9510565162951535312, 1.000000000000000000, 0.9510565162951535312, 1.000000000000000000, 0.9510565162951535312, 1.000000000000000000, 0.9510565162951535312, 1.000000000000000000, 0.9510565162951535312, 1.000000000000000000, 0.9510565162951535312, 1.000000000000000000, 0.9510565162951535312, 1.000000000000000000, 0.9510565162951535312, 1.000000000000000000, 0.9510565162951535312, 1.000000000000000000, 0.9510565162951535312, 1.000000000000000000, 0.9510565162951535312, 1.000000000000000000, 0.9510565162951535312, 1.000000000000000000, 0.9510565162951535312, 1.000000000000000000, 0.9510565162951535312, 1.000000000000000000, 0.9510565162951535312, 1.000000000000000000, 0.9510565162951535312, 1.000000000000000000, 0.9510565162951535312, 1.000000000000000000, 0.9510565162951535312, 1.000000000000000000, 0.9510565162951535312, 1.000000000000000000, 0.9510565162951535312, 1.000000000000000000, 0.9510565162951535312, 1.000000000000000000, 0.9510565162951535312, 1.000000000000000000, 0.9510565162951535312, 1.000000000000000000, 0.9510565162951535312, 1.000000000000000000, 0.9510565162951535312, 1.000000000000000000, 0.9510565162951535312, 1.000000000000000000, 0.9510565162951535312, 1.000000000000000000, 0.9510565162951535312, 1.000000000000000000, 0.9510565162951535312, 1.000000000000000000, 0.9510565162951535312, 1.000000000000000000, 0.9510565162951535312, 1.000000000000000000, 0.9510565162951535312, 1.000000000000000000, 0.9510565162951535312, 1.000000000000000000, 0.9510565162951535312, 1.000000000000000000, 0.9510565162951535312, 1.000000000000000000, 0.9510565162951535312, 1.000000000000000000, 0.9510565162951535312, 1.000000000000000000, 0.9510565162951535312, 1.000000000000000000, 0.9510565162951535312, 1.000000000000000000, 0.9510565162951535312, 1.000000000000000000, 0.9510565162951535312, 1.000000000000000000, 0.9510565162951535312, 1.000000000000000000, 0.9510565162951535312, 1.000000000000000000, 0.9510565162951535312, 1.000000000000000000, 0.9510565162951535312, 1.000000000000000000, 0.9510565162951535312, 1.000000000000000000, 0.9510565162951535312, 1.000000000000000000, 0.9510565162951535312, 1.000000000000000000, 0.9510565162951535312, 1.000000000000000000, 0.9510565162951535312, 1.000000000000000000, 0.9510565162951535312, 1.000000000000000000, 0.9510565162951535312, 1.000000000000000000, 0.9510565162951535312, 1.000000000000000000, 0.9510565162951535312, 1.000000000000000000, 0.9510565162951535312, 1.000000000000000000, 0.9510565162951535312, 1.000000000000000000, 0.9510565162951535312, 1.000000000000000000, 0.9510565162951535312, 1.000000000000000000, 0.9510565162951535312, 1.000000000000000000, 0.9510565162951535312, 1.000000000000000000, 0.9510565162951535312, 1.000000000000000000, 0.9510565162951535312, 1.000000000000000000, 0.9510565162951535312, 1.000000000000000000, 0.9510565162951535312, 1.000000000000000000, 0.9510565162951535312, 1.000000000000000000, 0.9510565162951535312, 1.000000000000000000, 0.9510565162951535312, 1.000000000000000000, 0.9510565162951535312, 1.000000000000000000, 0.9510565162951535312, 1.000000000000000000, 0.9510565162951535312, 1.000000000000000000, 0.9510565162951535312, 1.000000000000000000, 0.9510565162951535312, 1.000000000000000000, 0.9510565162951535312, 1.000000000000000000, 0.9510565162951535312, 1.000000000000000000, 0.9510565162951535312, 1.000000000000000000, 0.9510565162951535312, 1.000000000000000000, 0.9510565162951535312, 1.000000000000000000, 0.9510565162951535312, 1.000000000000000000, 0.9510565162951535312, 1.000000000000000000, 0.9510565162951535312, 1.000000000000000000, 0.9510565162951535312, 1.000000000000000000, 0.9510565162951535312, 1.000000000000000000, 0.9510565162951535312, 1.000000000000000000, 0.9510565162951535312, 1.000000000000000000, 0.9510565162951535312, 1.000000000000000000, 0.9510565162951535312, 1.000000000000000000, 0.9510565162951535312, 1.000000000000000000, 0.9510565162951535312, 1.000000000000000000, 0.9510565162951535312, 1.000000000000000000, 0.9510565162951535312, 1.000000000000000000, 0.9510565162951535312, 1.000000000000000000, 0.9510565162951535312, 1.000000000000000000, 0.9510565162951535312, 1.000000000000000000, 0.9510565162951535312, 1.000000000000000000, 0.9510565162951535312, 1.000000000000000000, 0.9510565162951535312, 1.000000000000000000, 0.9510565162951535312, 1.000000000000000000, 0.9510565162951535312, 1.000000000000000000, 0.9510565162951535312, 1.000000000000000000, 0.9510565162951535312, 1.000000000000000000, 0.9510565162951535312, 1.000000000000000000, 0.9510565162951535312, 1.000000000000000000, 0.9510565162951535312, 1.000000000000000000, 0.9510565162951535312, 1.000000000000000000, 0.9510565162951535312, 1.000000000000000000, 0.9510565162951535312, 1.000000000000000000, 0.9510565162951535312, 1.000000000000000000, 0.9510565162951535312, 1.000000000000000000, 0.9510565162951535312, 1.000000000000000000, 0.9510565162951535312, 1.000000000000000000, 0.9510565162951535312, 1.000000000000000000, 0.9510565162951535312, 1.000000000000000000, 0.9510565162951535312, 1.000000000000000000, 0.9510565162951535312, 1.000000000000000000, 0.9510565162951535312, 1.000000000000000000, 0.9510565162951535312, 1.000000000000000000, 0.9510565162951535312, 1.000000000000000000, 0.9510565162951535312, 1.000000000000000000, 0.9510565162951535312, 1.000000000000000000, 0.9510565162951535312, 1.000000000000000000, 0.9510565162951535312, 1.000000000000000000, 0.9510565162951535312, 1.000000000000000000, 0.9510565162951535312, 1.000000000000000000, 0.9510565162951535312, 1.000000000000000000, 0.9510565162951535312, 1.000000000000000000, 0.9510565162951535312, 1.000000000000000000, 0.9510565162951535312, 1.000000000000000000, 0.9510565162951535312, 1.000000000000000000, 0.9510565162951535312, 1.000000000000000000, 0.9510565162951535312, 1.000000000000000000, 0.9510565162951535312, 1.000000000000000000, 0.9510565162951535312, 1.000000000000000000, 0.9510565162951535312, 1.000000000000000000, 0.9510565162951535312, 1.000000000000000000, 0.9510565162951535312, 1.000000000000000000, 0.9510565162951535312, 1.000000000000000000, 0.9510565162951535312, 1.000000000000000000, 0.9510565162951535312, 1.000000000000000000, 0.9510565162951535312, 1.000000000000000000, 0.9510565162951535312, 1.000000000000000000, 0.9510565162951535312, 1.000000000000000000, 0.9510565162951535312, 1.000000000000000000, 0.9510565162951535312, 1.000000000000000000, 0.9510565162951535312, 1.000000000000000000, 0.9510565162951535312, 1.000000000000000000, 0.9510565162951535312, 1.000000000000000000, 0.9510565162951535312, 1.000000000000000000, 0.9510565162951535312, 1.000000000000000000, 0.9510565162951535312, 1.000000000000000000, 0.9510565162951535312, 1.000000000000000000, 0.9510565162951535312, 1.000000000000000000, 0.9510565162951535312, 1.000000000000000000, 0.9510565162951535312, 1.000000000000000000, 0.9510565162951535312, 1.000000000000000000, 0.9510565162951535312, 1.000000000000000000, 0.9510565162951535312, 1.000000000000000000, 0.9510565162951535312, 1.000000000000000000, 0.9510565162951535312, 1.000000000000000000, 0.9510565162951535312, 1.000000000000000000, 0.9510565162951535312, 1.000000000000000000, 0.9510565162951535312, 1.000000000000000000, 0.9510565162951535312, 1.000000000000000000, 0.9510565162951535312, 1.000000000000000000, 0.9510565162951535312, 1.000000000000000000, 0.9510565162951535312, 1.000000000000000000, 0.9510565162951535312, 1.000000000000000000, 0.9510565162951535312, 1.000000000000000000, 0.9510565162951535312, 1.000000000000000000, 0.9510565162951535312, 1.000000000000000000, 0.9510565162951535312, 1.000000000000000000, 0.9510565162951535312, 1.000000000000000000, 0.9510565162951535312, 1.000000000000000000, 0.9510565162951535312, 1.000000000000000000, 0.9510565162951535312, 1.000000000000000000, 0.9510565162951535312, 1.000000000000000000, 0.9510565162951535312, 1.000000000000000000, 0.9510565162951535312, 1.000000000000000000, 0.9510565162951535312, 1.000000000000000000, 0.9510565162951535312, 1.000000000000000000, 0.9510565162951535312, 1.000000000000000000, 0.9510565162951535312, 1.000000000000000000, 0.9510565162951535312, 1.000000000000000000, 0.9510565162951535312, 1.000000000000000000, 0.9510565162951535312, 1.000000000000000000, 0.9510565162951535312, 1.000000000000000000, 0.9510565162951535312, 1.000000000000000000, 0.9510565162951535312, 1.000000000000000000, 0.9510565162951535312, 1.000000000000000000, 0.9510565162951535312, 1.000000000000000000, 0.9510565162951535312, 1.000000000000000000, 0.9510565162951535312, 1.000000000000000000, 0.9510565162951535312, 1.000000000000000000, 0.9510565162951535312, 1.000000000000000000, 0.9510565162951535312, 1.000000000000000000, 0.9510565162951535312, 1.000000000000000000, 0.9510565162951535312, 1.000000000000000000, 0.9510565162951535312, 1.000000000000000000, 0.9510565162951535312, 1.000000000000000000, 0.9510565162951535312, 1.000000000000000000, 0.9510565162951535312, 1.000000000000000000, 0.9510565162951535312, 1.000000000000000000, 0.9510565162951535312, 1.000000000000000000, 0.9510565162951535312, 1.000000000000000000, 0.9510565162951535312, 1.000000000000000000, 0.9510565162951535312, 1.000000000000000000, 0.9510565162951535312, 1.000000000000000000, 0.9510565162951535312, 1.000000000000000000, 0.9510565162951535312, 1.000000000000000000, 0.9510565162951535312, 1.000000000000000000, 0.9510565162951535312, 1.000000000000000000, 0.9510565162951535312, 1.000000000000000000, 0.9510565162951535312, 1.000000000000000000) ) ) 
 REPRESENTATION_ITEM ( '' )  SURFACE ( )  );
#20824 = CARTESIAN_POINT ( 'NONE',  ( 20.75514604977248467, 10.67500000273119021, -28.56700777964554305 ) ) ;
#20825 = CYLINDRICAL_SURFACE ( 'NONE', #10747, 32.50000000000000000 ) ;
#20826 = CARTESIAN_POINT ( 'NONE',  ( 13.94119854578893580, 35.34076416574268364, -24.22776226481265383 ) ) ;
#20827 = CARTESIAN_POINT ( 'NONE',  ( -13.91746824999999532, 81.27500000273120406, -4.522059556121115875 ) ) ;
#20828 = DIRECTION ( 'NONE',  ( 0.000000000000000000, -1.000000000000000000, 0.000000000000000000 ) ) ;
#20829 = FACE_OUTER_BOUND ( 'NONE', #6434, .T. ) ;
#20830 = CARTESIAN_POINT ( 'NONE',  ( -20.75514604977248112, 73.67500000273120975, 28.56700777964554661 ) ) ;
#20831 = VERTEX_POINT ( 'NONE', #8757 ) ;
#20832 = CARTESIAN_POINT ( 'NONE',  ( -14.47279130897151589, 15.82499999726881335, -19.92008829642072598 ) ) ;
#20833 = CARTESIAN_POINT ( 'NONE',  ( -6.988114217768288228, 60.41145833333332149, -26.07999730980477437 ) ) ;
#20834 = CARTESIAN_POINT ( 'NONE',  ( -27.16883889988623935, 55.32500000273120122, 19.73931689729374739 ) ) ;
#20835 = CARTESIAN_POINT ( 'NONE',  ( 10.37757302488624056, 18.77500000273117564, -31.93888565452638417 ) ) ;
#20836 = CARTESIAN_POINT ( 'NONE',  ( 27.16883889988623935, 4.575000002731186122, -19.73931689729374384 ) ) ;
#20837 = CARTESIAN_POINT ( 'NONE',  ( 19.09188309203661049, 40.35937499999999289, -19.09188309203694445 ) ) ;
#20838 = CARTESIAN_POINT ( 'NONE',  ( -7.468012846824771955, 34.34934000092397355, -28.02196122052045624 ) ) ;
#20839 = CARTESIAN_POINT ( 'NONE',  ( -7.543491769121917656, 17.72357666574268720, -28.00173670424536354 ) ) ;
#20840 = CARTESIAN_POINT ( 'NONE',  ( -20.08610463437157989, 76.20000000546235697, -27.64615127144129758 ) ) ;
#20841 = CARTESIAN_POINT ( 'NONE',  ( 14.41072458151315594, 52.00000000000000000, -29.41684567868830769 ) ) ;
#20842 = CARTESIAN_POINT ( 'NONE',  ( -27.16883889988623935, 45.32500000273117990, 19.73931689729374739 ) ) ;
#20843 = CARTESIAN_POINT ( 'NONE',  ( 1.507698388325705758E-15, 9.124999997268822938, -24.62258325217400312 ) ) ;
#20844 = CARTESIAN_POINT ( 'NONE',  ( 19.82091636218621389, 14.19999999999999041, -14.40073868116559197 ) ) ;
#20845 = VERTEX_POINT ( 'NONE', #31929 ) ;
#20846 = CARTESIAN_POINT ( 'NONE',  ( 33.58253175000000113, 52.47500000273117138, -10.91162601494193751 ) ) ;
#20847 = CARTESIAN_POINT ( 'NONE',  ( 30.00000000000001421, -91.00000000000000000, 3.673940397442059967E-15 ) ) ;
#20848 = CARTESIAN_POINT ( 'NONE',  ( -24.22776226481240514, 40.22173583425730925, 13.94119854578937812 ) ) ;
#20849 = CARTESIAN_POINT ( 'NONE',  ( 27.16883889988623935, 78.57500000273121543, -19.73931689729374384 ) ) ;
#20850 = VERTEX_POINT ( 'NONE', #27291 ) ;
#20851 = CARTESIAN_POINT ( 'NONE',  ( -33.58253175000000113, 23.22500000273117138, 10.91162601494193929 ) ) ;
#20852 = CARTESIAN_POINT ( 'NONE',  ( 26.00068869287340334, 13.00260416666666430, -15.01150461594642316 ) ) ;
#20853 = ORIENTED_EDGE ( 'NONE', *, *, #32622, .T. ) ;
#20854 = CARTESIAN_POINT ( 'NONE',  ( -5.147494310547423346, 14.94874572391553080, 32.50000000000000000 ) ) ;
#20855 = CARTESIAN_POINT ( 'NONE',  ( 33.58253175000000823, 62.02500000273116143, 10.91162601494192863 ) ) ;
#20856 = CARTESIAN_POINT ( 'NONE',  ( 7.505752307973351023, 48.38020833333332860, 28.01184896238290278 ) ) ;
#20857 = DIRECTION ( 'NONE',  ( 0.000000000000000000, 0.000000000000000000, 1.000000000000000000 ) ) ;
#20858 = CARTESIAN_POINT ( 'NONE',  ( -23.41746824999999887, 2.024999997268815299, -7.608796670333730638 ) ) ;
#20859 = CARTESIAN_POINT ( 'NONE',  ( 27.16883889988623935, 2.325000002731170134, -19.73931689729374384 ) ) ;
#20860 = SURFACE_STYLE_FILL_AREA ( #23081 ) ;
#20861 = CARTESIAN_POINT ( 'NONE',  ( -15.04653450569338524, 65.70534749907602645, -25.98046417659831775 ) ) ;
#20862 = DIRECTION ( 'NONE',  ( -0.000000000000000000, -1.000000000000000000, -0.000000000000000000 ) ) ;
#20863 = CARTESIAN_POINT ( 'NONE',  ( 1.836970198721029589E-15, 82.00000000000001421, 15.00000000000000000 ) ) ;
#20864 = CARTESIAN_POINT ( 'NONE',  ( -26.29305231718579350, 59.80000000000000426, -19.10302069950537884 ) ) ;
#20865 = CARTESIAN_POINT ( 'NONE',  ( 26.29305231718578995, 17.19999999999997797, -19.10302069950538240 ) ) ;
#20866 = CARTESIAN_POINT ( 'NONE',  ( -26.07999730980490583, 56.40104166666666430, -6.988114217767815717 ) ) ;
#20867 = CARTESIAN_POINT ( 'NONE',  ( -19.82091636218621034, 14.54999999453762705, -14.40073868116559552 ) ) ;
#20868 = CARTESIAN_POINT ( 'NONE',  ( 13.91746824999999887, 79.87500000273118417, -1.704398294459741270E-15 ) ) ;
#20869 = CARTESIAN_POINT ( 'NONE',  ( -26.07999730980477437, 32.05208333333332860, 6.988114217768305103 ) ) ;
#20870 = CARTESIAN_POINT ( 'NONE',  ( 20.75514604977249178, 33.82500000273117990, 28.56700777964553950 ) ) ;
#20871 = PRODUCT ( 'level compensator', 'level compensator', '', ( #26382 ) ) ;
#20872 = CARTESIAN_POINT ( 'NONE',  ( 20.75514604977248467, 70.42500000273119554, -28.56700777964554305 ) ) ;
#20873 = CARTESIAN_POINT ( 'NONE',  ( -20.75514604977248112, 33.67500000273119554, 28.56700777964554661 ) ) ;
#20874 = CARTESIAN_POINT ( 'NONE',  ( 33.58253175000000823, 18.27500000273118275, 10.91162601494192685 ) ) ;
#20875 = CARTESIAN_POINT ( 'NONE',  ( -2.375766604868044585, 80.44874571845313938, 14.99999999999999822 ) ) ;
#20876 = CARTESIAN_POINT ( 'NONE',  ( -19.11951029504763611, 50.39100666759063785, 19.06425588902592239 ) ) ;
#20877 = CARTESIAN_POINT ( 'NONE',  ( -20.75514604977248112, 73.42500000273118133, 28.56700777964554661 ) ) ;
#20878 = CARTESIAN_POINT ( 'NONE',  ( -20.08610463437156923, 66.29999999999999716, 27.64615127144130113 ) ) ;
#20879 = CARTESIAN_POINT ( 'NONE',  ( -32.50000000000000000, 59.89999999999999858, -10.55989012756945478 ) ) ;
#20880 = CARTESIAN_POINT ( 'NONE',  ( -7.236395654485763274, 18.02499999726880731, 22.27133577429736633 ) ) ;
#20881 = CARTESIAN_POINT ( 'NONE',  ( -10.37757302488623701, 65.52500000273120406, 31.93888565452638417 ) ) ;
#20882 = CARTESIAN_POINT ( 'NONE',  ( 23.41746825000000243, 7.224999997268826135, -7.608796670333727974 ) ) ;
#20883 = CARTESIAN_POINT ( 'NONE',  ( -10.37757302488623701, 71.77500000273118985, 31.93888565452638417 ) ) ;
#20884 = CARTESIAN_POINT ( 'NONE',  ( 20.75514604977249178, 7.825000002731194115, 28.56700777964553950 ) ) ;
#20885 = CARTESIAN_POINT ( 'NONE',  ( -23.41746825000000243, 1.524999997268801755, -7.608796670333730638 ) ) ;
#20886 = CARTESIAN_POINT ( 'NONE',  ( 24.22776226481241224, 14.44048583425730925, -13.94119854578936923 ) ) ;
#20887 = VERTEX_POINT ( 'NONE', #26792 ) ;
#20888 = CARTESIAN_POINT ( 'NONE',  ( 10.37757302488624767, 43.72500000273120691, 31.93888565452638417 ) ) ;
#20889 = ORIENTED_EDGE ( 'NONE', *, *, #22244, .T. ) ;
#20890 = CARTESIAN_POINT ( 'NONE',  ( 26.00068869287340334, 40.50260416666666430, -15.01150461594642316 ) ) ;
#20891 = CARTESIAN_POINT ( 'NONE',  ( 3.980102097228898626E-15, 80.00000000000001421, 32.50000000000000000 ) ) ;
#20892 = CARTESIAN_POINT ( 'NONE',  ( -2.092463501923844636E-15, 2.000000005462382102, -34.17252228774368916 ) ) ;
#20893 = CARTESIAN_POINT ( 'NONE',  ( -20.08610463437156923, 72.30000000000001137, 27.64615127144130113 ) ) ;
#20894 = CARTESIAN_POINT ( 'NONE',  ( 23.41746825000000243, 3.224999997268806151, -7.608796670333727974 ) ) ;
#20895 = CARTESIAN_POINT ( 'NONE',  ( -7.236395654485763274, 16.02499999726880731, 22.27133577429736633 ) ) ;
#20896 = CARTESIAN_POINT ( 'NONE',  ( -20.75514604977248112, 17.67500000273117422, 28.56700777964554661 ) ) ;
#20897 = CARTESIAN_POINT ( 'NONE',  ( -20.08610463437156923, 58.29999999999999716, 27.64615127144130113 ) ) ;
#20898 = CARTESIAN_POINT ( 'NONE',  ( 3.880418787951178228, 12.19874571299079236, -24.49999999999998224 ) ) ;
#20899 = CARTESIAN_POINT ( 'NONE',  ( 5.147494310547440222, 73.94874572391552192, -32.50000000000000000 ) ) ;
#20900 = CIRCLE ( 'NONE', #11565, 10.72870458603808075 ) ;
#20901 = CARTESIAN_POINT ( 'NONE',  ( 7.543491769121922985, 36.62982666574267654, 28.00173670424535644 ) ) ;
#20902 = CARTESIAN_POINT ( 'NONE',  ( -13.91746824999999887, 73.37500000273119838, 0.000000000000000000 ) ) ;
#20903 = CARTESIAN_POINT ( 'NONE',  ( -2.584737979205442066E-13, 36.49218749999999289, -30.02300923189239867 ) ) ;
#20904 = DIRECTION ( 'NONE',  ( -1.000000000000000000, 0.000000000000000000, -0.000000000000000000 ) ) ;
#20905 = CARTESIAN_POINT ( 'NONE',  ( 20.08610463437158344, 6.699999999999991296, 27.64615127144129403 ) ) ;
#20906 = CARTESIAN_POINT ( 'NONE',  ( -8.891200544363830713E-16, 73.50000000000001421, -15.00000000000000000 ) ) ;
#20907 = CARTESIAN_POINT ( 'NONE',  ( 6.950374756619257965, 55.82253499907601935, -26.09010956794244507 ) ) ;
#20908 = CARTESIAN_POINT ( 'NONE',  ( 10.37757302488624767, 51.72500000273119980, 31.93888565452638417 ) ) ;
#20909 = CARTESIAN_POINT ( 'NONE',  ( -27.16883889988623935, 57.57500000273117990, 19.73931689729374739 ) ) ;
#20910 = CARTESIAN_POINT ( 'NONE',  ( -20.75514604977248823, 39.07500000273119412, -28.56700777964554305 ) ) ;
#20911 = CARTESIAN_POINT ( 'NONE',  ( 20.08610463437158344, 24.70000000000000284, 27.64615127144129403 ) ) ;
#20912 = CARTESIAN_POINT ( 'NONE',  ( 0.000000000000000000, 82.00000000000001421, 0.000000000000000000 ) ) ;
#20913 = CARTESIAN_POINT ( 'NONE',  ( -32.50000000000000000, 62.00000000000000000, 0.000000000000000000 ) ) ;
#20914 = EDGE_CURVE ( 'NONE', #26574, #6391, #7057, .T. ) ;
#20915 = CARTESIAN_POINT ( 'NONE',  ( -4.223320258572819786E-15, 5.249999994537622783, 24.50000000000000000 ) ) ;
#20916 = DIRECTION ( 'NONE',  ( -1.224646799147353454E-16, 1.000000000000000000, -0.000000000000000000 ) ) ;
#20917 = CARTESIAN_POINT ( 'NONE',  ( 20.75514604977249178, 17.82500000273120122, 28.56700777964553950 ) ) ;
#20918 = CARTESIAN_POINT ( 'NONE',  ( -5.147494310547430452, 62.05125428700922896, -32.49999999999999289 ) ) ;
#20919 = PLANE ( 'NONE',  #31434 ) ;
#20920 = EDGE_CURVE ( 'NONE', #31503, #18399, #6528, .T. ) ;
#20921 = FACE_OUTER_BOUND ( 'NONE', #6764, .T. ) ;
#20922 = CARTESIAN_POINT ( 'NONE',  ( -14.01125832528328985, 21.01784749907601579, -24.18731323226223040 ) ) ;
#20923 = CARTESIAN_POINT ( 'NONE',  ( 6.277390505771533514E-15, 35.00000000546237544, 34.17252228774368916 ) ) ;
#20924 = CARTESIAN_POINT ( 'NONE',  ( -4.405589869732278832E-13, 10.49999999999998934, 32.50000000000000000 ) ) ;
#20925 = CARTESIAN_POINT ( 'NONE',  ( 33.58253175000000823, 28.02500000273119340, 10.91162601494192685 ) ) ;
#20926 = AXIS2_PLACEMENT_3D ( 'NONE', #8021, #15763, #7849 ) ;
#20927 = CIRCLE ( 'NONE', #28037, 30.00000000000000711 ) ;
#20928 = CARTESIAN_POINT ( 'NONE',  ( 26.07999730980477437, 40.64583333333332860, -6.988114217768290004 ) ) ;
#20929 = ORIENTED_EDGE ( 'NONE', *, *, #24795, .F. ) ;
#20930 = CARTESIAN_POINT ( 'NONE',  ( 20.75514604977249178, 63.82500000273119412, 28.56700777964553950 ) ) ;
#20931 = ADVANCED_FACE ( 'NONE', ( #16496 ), #5858, .F. ) ;
#20932 = CARTESIAN_POINT ( 'NONE',  ( -28.01184896238290278, 45.80208333333333570, 7.505752307973363457 ) ) ;
#20933 = ORIENTED_EDGE ( 'NONE', *, *, #30695, .F. ) ;
#20934 = CARTESIAN_POINT ( 'NONE',  ( -15.01150461594595775, 14.43489583333332682, 26.00068869287368756 ) ) ;
#20935 = CARTESIAN_POINT ( 'NONE',  ( -20.47846945139902175, 16.87538166759064140, -20.53372385742072481 ) ) ;
#20936 = CARTESIAN_POINT ( 'NONE',  ( -27.16883889988623935, 7.325000002731188786, 19.73931689729374739 ) ) ;
#20937 = CARTESIAN_POINT ( 'NONE',  ( 18.94512977948576093, 0.8249999972688160099, -13.76444248337722875 ) ) ;
#20938 = CARTESIAN_POINT ( 'NONE',  ( -10.37757302488624411, 32.97500000273117848, -31.93888565452638417 ) ) ;
#20939 = CARTESIAN_POINT ( 'NONE',  ( -32.50000000000000000, 36.60000000546239818, 10.55989012756946366 ) ) ;
#20940 = CARTESIAN_POINT ( 'NONE',  ( -9.657523855033125146E-16, 77.50000000000000000, -15.77193336357400710 ) ) ;
#20941 = CARTESIAN_POINT ( 'NONE',  ( -26.00068869287340334, 62.84635416666667851, 15.01150461594643382 ) ) ;
#20942 = CARTESIAN_POINT ( 'NONE',  ( 20.75514604977248467, 22.42500000273119909, -28.56700777964554305 ) ) ;
#20943 = CARTESIAN_POINT ( 'NONE',  ( 7.570916362186213000, 6.149999994537635573, -23.30088464923126423 ) ) ;
#20944 = CARTESIAN_POINT ( 'NONE',  ( -20.75514604977248112, 51.67500000273117422, 28.56700777964554661 ) ) ;
#20945 = PRESENTATION_STYLE_ASSIGNMENT (( #15964 ) ) ;
#20946 = CARTESIAN_POINT ( 'NONE',  ( -10.04305231718579172, 27.59999999999999787, -30.90933677959248982 ) ) ;
#20947 = CARTESIAN_POINT ( 'NONE',  ( 10.04305231718579705, 26.60000000000001208, 30.90933677959248982 ) ) ;
#20948 = CARTESIAN_POINT ( 'NONE',  ( -4.732186688966233175E-15, 5.500000000000000888, 25.76082449383753925 ) ) ;
#20949 = CARTESIAN_POINT ( 'NONE',  ( 27.16883889988623935, 72.32500000273117280, -19.73931689729374384 ) ) ;
#20950 = CARTESIAN_POINT ( 'NONE',  ( -19.82091636218621034, 2.549999994537616388, -14.40073868116559552 ) ) ;
#20951 = CARTESIAN_POINT ( 'NONE',  ( -32.50000000000000000, 76.40000000546235981, -10.55989012756945300 ) ) ;
#20952 = CARTESIAN_POINT ( 'NONE',  ( -10.37757302488624411, 58.97500000273120691, -31.93888565452638417 ) ) ;
#20953 = CARTESIAN_POINT ( 'NONE',  ( 20.08610463437158344, 7.200000005462392494, 27.64615127144129403 ) ) ;
#20954 = CARTESIAN_POINT ( 'NONE',  ( -27.16883889988624290, 10.92500000273119376, -19.73931689729374028 ) ) ;
#20955 = CARTESIAN_POINT ( 'NONE',  ( -27.95245687107223986, 33.63319416759063785, -0.04044903254993292840 ) ) ;
#20956 = CARTESIAN_POINT ( 'NONE',  ( 3.445340210940985210E-14, 9.249999994537636994, 24.50000000000000000 ) ) ;
#20957 = CARTESIAN_POINT ( 'NONE',  ( -33.58253175000000113, 1.475000002731190474, 10.91162601494193929 ) ) ;
#20958 = CARTESIAN_POINT ( 'NONE',  ( 20.75514604977249178, 31.82500000273119056, 28.56700777964553950 ) ) ;
#20959 = CARTESIAN_POINT ( 'NONE',  ( 24.50000000000000000, 18.87499999726882649, 0.000000000000000000 ) ) ;
#20960 = CARTESIAN_POINT ( 'NONE',  ( -1.778240108872766143E-15, 19.50000000000000000, -32.49999999999999289 ) ) ;
#20961 = CARTESIAN_POINT ( 'NONE',  ( 13.91746825000000065, 77.77500000273116143, 4.522059556121115875 ) ) ;
#20962 = CARTESIAN_POINT ( 'NONE',  ( -14.97647472619899389, 47.37201416574269786, 26.02091320914878025 ) ) ;
#20963 = CARTESIAN_POINT ( 'NONE',  ( -10.04305231718579172, 56.10000000546237686, -30.90933677959248982 ) ) ;
#20964 = CARTESIAN_POINT ( 'NONE',  ( -8.601468415847515203, 79.67500000273115290, 11.83890561707634959 ) ) ;
#20965 = CARTESIAN_POINT ( 'NONE',  ( -24.20753774853756823, 15.29427083333332504, -13.97622843553588723 ) ) ;
#20966 = CARTESIAN_POINT ( 'NONE',  ( 18.94512977948576093, 1.324999997268816454, -13.76444248337722875 ) ) ;
#20967 = CARTESIAN_POINT ( 'NONE',  ( -32.50000000000000000, 68.50000000546238255, 0.000000000000000000 ) ) ;
#20968 = CARTESIAN_POINT ( 'NONE',  ( 28.01184896238290278, 23.45833333333333215, -7.505752307973347470 ) ) ;
#20969 = CARTESIAN_POINT ( 'NONE',  ( 20.75514604977249178, 36.07500000273117990, 28.56700777964553950 ) ) ;
#20970 = CARTESIAN_POINT ( 'NONE',  ( 14.47279130897151767, 12.82499999726882400, 19.92008829642072953 ) ) ;
#20971 = VERTEX_POINT ( 'NONE', #693 ) ;
#20972 = CARTESIAN_POINT ( 'NONE',  ( -20.53372385742071771, 43.51600666759065206, 20.47846945139902530 ) ) ;
#20973 = VECTOR ( 'NONE', #3042, 1000.000000000000000 ) ;
#20974 = CARTESIAN_POINT ( 'NONE',  ( -2.092463501923844636E-15, 18.00000000546237189, -34.17252228774368916 ) ) ;
#20975 = CARTESIAN_POINT ( 'NONE',  ( 20.50609665440969565, 47.23437499999999289, -20.50609665441004736 ) ) ;
#20976 = LINE ( 'NONE', #9, #23991 ) ;
#20977 = CARTESIAN_POINT ( 'NONE',  ( 33.58253175000000113, 56.47500000273116427, -10.91162601494193751 ) ) ;
#20978 = CARTESIAN_POINT ( 'NONE',  ( 32.50000000000000711, 57.40000000546237402, 10.55989012756945122 ) ) ;
#20979 = EDGE_CURVE ( 'NONE', #2384, #32915, #11179, .T. ) ;
#20980 = CARTESIAN_POINT ( 'NONE',  ( 15.14183272437242422, 6.049999994537626158, -20.84094480462497856 ) ) ;
#20981 = CARTESIAN_POINT ( 'NONE',  ( -33.58253175000000113, 45.12500000273117706, 0.000000000000000000 ) ) ;
#20982 = CARTESIAN_POINT ( 'NONE',  ( -9.270509831248419985, 76.55000000546239391, 12.75976212528060039 ) ) ;
#20983 = CARTESIAN_POINT ( 'NONE',  ( 10.37757302488624767, 69.97500000273119269, 31.93888565452638417 ) ) ;
#20984 = CARTESIAN_POINT ( 'NONE',  ( 13.18564821210877014, 74.00000000000005684, 4.476740745196889470 ) ) ;
#20985 = CARTESIAN_POINT ( 'NONE',  ( 6.486482029760648627E-15, 61.62500000273118417, 35.31076352940722529 ) ) ;
#20986 = CARTESIAN_POINT ( 'NONE',  ( 30.02300923189239867, 20.16406249999999645, -2.619432448724978208E-13 ) ) ;
#20987 = CARTESIAN_POINT ( 'NONE',  ( -32.50000000000000000, 43.99999999999998579, 0.000000000000000000 ) ) ;
#20988 = CARTESIAN_POINT ( 'NONE',  ( -18.94512977948575738, 3.424999997268807217, -13.76444248337723231 ) ) ;
#20989 = CARTESIAN_POINT ( 'NONE',  ( 10.37757302488624056, 10.77500000273118275, -31.93888565452638417 ) ) ;
#20990 = AXIS2_PLACEMENT_3D ( 'NONE', #33647, #7563, #26095 ) ;
#20991 = LINE ( 'NONE', #28864, #24427 ) ;
#20992 = CARTESIAN_POINT ( 'NONE',  ( 14.01125832528330051, 36.48659749907601935, 24.18731323226221974 ) ) ;
#20993 = CARTESIAN_POINT ( 'NONE',  ( -8.601468415847518756, 73.07500000273115859, -11.83890561707634781 ) ) ;
#20994 = LINE ( 'NONE', #2626, #12949 ) ;
#20995 = CARTESIAN_POINT ( 'NONE',  ( 0.000000000000000000, -12.99999999999999822, 27.00000000000000000 ) ) ;
#20996 = CARTESIAN_POINT ( 'NONE',  ( 10.37757302488624767, 73.97500000273120691, 31.93888565452638417 ) ) ;
#20997 = ORIENTED_EDGE ( 'NONE', *, *, #7791, .F. ) ;
#20998 = DIRECTION ( 'NONE',  ( -1.000000000000000000, 0.000000000000000000, 0.000000000000000000 ) ) ;
#20999 = CARTESIAN_POINT ( 'NONE',  ( 6.988114217768294445, 62.13020833333334281, 26.07999730980477437 ) ) ;
#21000 = CARTESIAN_POINT ( 'NONE',  ( 33.58253175000000823, 54.02500000273118275, 10.91162601494192863 ) ) ;
#21001 = CARTESIAN_POINT ( 'NONE',  ( 33.58253175000000113, 20.47500000273120335, -10.91162601494193751 ) ) ;
#21002 = CARTESIAN_POINT ( 'NONE',  ( 20.75514604977248467, 6.675000002731186655, -28.56700777964554305 ) ) ;
#21003 = CARTESIAN_POINT ( 'NONE',  ( 26.07999730980490227, 37.49479166666666430, 6.988114217767821046 ) ) ;
#21004 = CARTESIAN_POINT ( 'NONE',  ( -30.02300923189239867, 26.75819416759064495, -0.04044903254991731589 ) ) ;
#21005 = CARTESIAN_POINT ( 'NONE',  ( 7.468012846824281681, 21.44753499907601579, -28.02196122052058058 ) ) ;
#21006 = CARTESIAN_POINT ( 'NONE',  ( 10.04305231718579705, 71.10000000546239107, 30.90933677959248982 ) ) ;
#21007 = CARTESIAN_POINT ( 'NONE',  ( 5.393181536354239469, 52.00000000000000711, -32.17179393301736923 ) ) ;
#21008 = CARTESIAN_POINT ( 'NONE',  ( -27.16883889988623935, 37.32500000273120122, 19.73931689729374739 ) ) ;
#21009 = CARTESIAN_POINT ( 'NONE',  ( 26.09010956794244507, 49.80690999907602645, 6.950374756619249084 ) ) ;
#21010 = CARTESIAN_POINT ( 'NONE',  ( 23.41746825000000243, 10.52499999726880731, 7.608796670333735079 ) ) ;
#21011 = CARTESIAN_POINT ( 'NONE',  ( -7.347880794884122694E-16, -16.99999999999999645, 0.000000000000000000 ) ) ;
#21012 = ORIENTED_EDGE ( 'NONE', *, *, #19074, .F. ) ;
#21013 = CARTESIAN_POINT ( 'NONE',  ( -27.16883889988623935, 55.57500000273117280, 19.73931689729374739 ) ) ;
#21014 = AXIS2_PLACEMENT_3D ( 'NONE', #16858, #27146, #29383 ) ;
#21015 = CARTESIAN_POINT ( 'NONE',  ( 14.01125832528286352, 41.65402750092398065, -24.18731323226246843 ) ) ;
#21016 = CARTESIAN_POINT ( 'NONE',  ( 33.58253175000000823, 76.27500000273118985, 10.91162601494192863 ) ) ;
#21017 = ORIENTED_EDGE ( 'NONE', *, *, #28242, .T. ) ;
#21018 = CARTESIAN_POINT ( 'NONE',  ( -33.58253175000000113, 23.12500000273119838, 0.000000000000000000 ) ) ;
#21019 = VECTOR ( 'NONE', #12261, 1000.000000000000000 ) ;
#21020 = CARTESIAN_POINT ( 'NONE',  ( 7.505752307973351023, 17.44270833333333215, 28.01184896238290278 ) ) ;
#21021 = ADVANCED_FACE ( 'NONE', ( #26950 ), #30182, .T. ) ;
#21022 = ORIENTED_EDGE ( 'NONE', *, *, #8739, .F. ) ;
#21023 = DIRECTION ( 'NONE',  ( 0.000000000000000000, 1.000000000000000000, 0.000000000000000000 ) ) ;
#21024 = CARTESIAN_POINT ( 'NONE',  ( -2.162160676586881955E-15, 58.62500000273118417, -35.31076352940723240 ) ) ;
#21025 = CARTESIAN_POINT ( 'NONE',  ( -28.01184896238290278, 49.23958333333332860, 7.505752307973363457 ) ) ;
#21026 = EDGE_CURVE ( 'NONE', #21853, #3936, #9457, .T. ) ;
#21027 = CARTESIAN_POINT ( 'NONE',  ( 15.14183272437241889, 17.69999999999999218, 20.84094480462498211 ) ) ;
#21028 = CARTESIAN_POINT ( 'NONE',  ( -23.41746824999999887, 12.02499999726881974, -7.608796670333730638 ) ) ;
#21029 = CARTESIAN_POINT ( 'NONE',  ( 27.16883889988624290, 5.925000002731190207, 19.73931689729373673 ) ) ;
#21030 = CARTESIAN_POINT ( 'NONE',  ( -12.13525491562420910, 78.45000000546237118, 8.816778784387098611 ) ) ;
#21031 = CARTESIAN_POINT ( 'NONE',  ( -25.98046417659831420, 64.84597249907602645, 15.04653450569339945 ) ) ;
#21032 = CARTESIAN_POINT ( 'NONE',  ( -12.13525491562421088, 80.05000000546236549, -8.816778784387096835 ) ) ;
#21033 = CARTESIAN_POINT ( 'NONE',  ( -20.50609665441004736, 63.56249999999999289, -20.50609665440969565 ) ) ;
#21034 = CARTESIAN_POINT ( 'NONE',  ( 10.04305231718579705, 75.10000000546237686, 30.90933677959248982 ) ) ;
#21035 = CARTESIAN_POINT ( 'NONE',  ( -20.08610463437156923, 16.29999999999997584, 27.64615127144130113 ) ) ;
#21036 = CARTESIAN_POINT ( 'NONE',  ( 24.20753774853756113, 65.13802083333334281, 13.97622843553589789 ) ) ;
#21037 = CARTESIAN_POINT ( 'NONE',  ( -7.570916362186210335, 16.34999999453762243, -23.30088464923126779 ) ) ;
#21038 = CARTESIAN_POINT ( 'NONE',  ( -15.00000000000000000, 70.25000000546238255, 0.000000000000000000 ) ) ;
#21039 = CARTESIAN_POINT ( 'NONE',  ( -26.07999730980477437, 35.48958333333332860, 6.988114217768305103 ) ) ;
#21040 = CARTESIAN_POINT ( 'NONE',  ( 27.16883889988624290, 33.92500000273118843, 19.73931689729373673 ) ) ;
#21041 = CARTESIAN_POINT ( 'NONE',  ( -33.58253175000000113, 73.02500000273120406, -10.91162601494193218 ) ) ;
#21042 = CARTESIAN_POINT ( 'NONE',  ( -2.162160676586881955E-15, 38.87500000273120548, -35.31076352940723240 ) ) ;
#21043 = CARTESIAN_POINT ( 'NONE',  ( -27.16883889988624290, 15.17500000273119909, -19.73931689729374028 ) ) ;
#21044 = CARTESIAN_POINT ( 'NONE',  ( 1.555960095263670572E-15, 14.24999999453762278, -24.50000000000000000 ) ) ;
#21045 = CARTESIAN_POINT ( 'NONE',  ( -24.22776226481240514, 57.40923583425731636, 13.94119854578937812 ) ) ;
#21046 = AXIS2_PLACEMENT_3D ( 'NONE', #33648, #7902, #31572 ) ;
#21047 = CARTESIAN_POINT ( 'NONE',  ( 27.16883889988623935, 74.32500000273117280, -19.73931689729374384 ) ) ;
#21048 = DIRECTION ( 'NONE',  ( 0.000000000000000000, 0.000000000000000000, -1.000000000000000000 ) ) ;
#21049 = CARTESIAN_POINT ( 'NONE',  ( 32.50000000000000711, 56.90000000000001279, 10.55989012756945122 ) ) ;
#21050 = CARTESIAN_POINT ( 'NONE',  ( -23.41746824999999887, 15.52499999726882507, -7.608796670333730638 ) ) ;
#21051 = CARTESIAN_POINT ( 'NONE',  ( 27.16883889988623935, 56.32500000273118701, -19.73931689729374384 ) ) ;
#21052 = CARTESIAN_POINT ( 'NONE',  ( 14.47279130897151767, 9.424999997268814766, -19.92008829642072598 ) ) ;
#21053 = VERTEX_POINT ( 'NONE', #25398 ) ;
#21054 = CARTESIAN_POINT ( 'NONE',  ( 33.58253175000000113, 74.37500000273118417, -4.112674001490185761E-15 ) ) ;
#21055 = CARTESIAN_POINT ( 'NONE',  ( -20.75514604977248112, 5.425000002731181326, 28.56700777964554661 ) ) ;
#21056 = CARTESIAN_POINT ( 'NONE',  ( -7.236395654485763274, 18.52499999726881086, 22.27133577429736633 ) ) ;
#21057 = CARTESIAN_POINT ( 'NONE',  ( -24.18731323226248264, 13.29465250092397532, -14.01125832528284931 ) ) ;
#21058 = ORIENTED_EDGE ( 'NONE', *, *, #33397, .T. ) ;
#21059 = CARTESIAN_POINT ( 'NONE',  ( -20.75514604977248112, 43.42500000273117422, 28.56700777964554661 ) ) ;
#21060 = ORIENTED_EDGE ( 'NONE', *, *, #4613, .F. ) ;
#21061 = CARTESIAN_POINT ( 'NONE',  ( -28.01184896238290278, 38.92708333333333570, 7.505752307973363457 ) ) ;
#21062 = CARTESIAN_POINT ( 'NONE',  ( 20.08610463437157279, 5.300000000000006040, -27.64615127144129758 ) ) ;
#21063 = CARTESIAN_POINT ( 'NONE',  ( 32.50000000000000000, 3.600000005462375086, -10.55989012756945833 ) ) ;
#21064 = CARTESIAN_POINT ( 'NONE',  ( 10.04305231718579705, 27.10000000546236620, 30.90933677959248982 ) ) ;
#21065 = AXIS2_PLACEMENT_3D ( 'NONE', #24850, #19711, #30157 ) ;
#21066 = CARTESIAN_POINT ( 'NONE',  ( 15.01150461594596308, 19.59114583333332149, -26.00068869287367335 ) ) ;
#21067 = CARTESIAN_POINT ( 'NONE',  ( 7.236395654485755280, 16.22499999726881370, 22.27133577429736988 ) ) ;
#21068 = CARTESIAN_POINT ( 'NONE',  ( 33.58253175000000113, 12.47500000273119447, -10.91162601494193751 ) ) ;
#21069 = CARTESIAN_POINT ( 'NONE',  ( 6.277390505771533514E-15, 60.49999999999997868, 34.17252228774368916 ) ) ;
#21070 = CARTESIAN_POINT ( 'NONE',  ( 4.300734207923761154, 79.47500000273119269, 13.23629886949340495 ) ) ;
#21071 = LINE ( 'NONE', #17811, #8821 ) ;
#21072 = CARTESIAN_POINT ( 'NONE',  ( -15.04653450569338524, 34.76784749907601935, -25.98046417659831775 ) ) ;
#21073 = CARTESIAN_POINT ( 'NONE',  ( -8.601468415847518756, 75.07500000273118701, -11.83890561707634781 ) ) ;
#21074 = CARTESIAN_POINT ( 'NONE',  ( 30.02300923189239867, 40.78906249999999289, -2.619432448724978208E-13 ) ) ;
#21075 = ITEM_DEFINED_TRANSFORMATION ( 'NONE', 'NONE', #33688,  #1376 ) ;
#21076 = DIRECTION ( 'NONE',  ( -0.000000000000000000, -1.000000000000000000, -0.000000000000000000 ) ) ;
#21077 = CARTESIAN_POINT ( 'NONE',  ( -24.50000000000000711, 13.09999999999999432, 7.960532557706201828 ) ) ;
#21078 = CARTESIAN_POINT ( 'NONE',  ( -32.50000000000000000, 3.899999999999992806, -10.55989012756945478 ) ) ;
#21079 = CARTESIAN_POINT ( 'NONE',  ( 5.779280353836490358E-15, 41.00000000546237544, 32.49999999999999289 ) ) ;
#21080 = CARTESIAN_POINT ( 'NONE',  ( 24.18731323226221974, 59.68972249907602645, -14.01125832528328985 ) ) ;
#21081 = CARTESIAN_POINT ( 'NONE',  ( -27.16883889988624290, 50.92500000273120264, -19.73931689729374028 ) ) ;
#21082 = CARTESIAN_POINT ( 'NONE',  ( -4.635254915624211769, 73.85000000546237686, -14.26584774442730286 ) ) ;
#21083 = CARTESIAN_POINT ( 'NONE',  ( 27.16883889988624290, 58.17500000273119554, 19.73931689729373673 ) ) ;
#21084 = CARTESIAN_POINT ( 'NONE',  ( 33.58253175000000113, 32.47500000273117138, -10.91162601494193574 ) ) ;
#21085 = CARTESIAN_POINT ( 'NONE',  ( 5.147494310547426899, 25.44874571845316069, -32.50000000000000000 ) ) ;
#21086 = CARTESIAN_POINT ( 'NONE',  ( 27.95245687107223276, 16.72656249999999645, -2.463307335887066074E-13 ) ) ;
#21087 = CARTESIAN_POINT ( 'NONE',  ( -24.50000000000000000, 8.900000000000011013, -7.960532557706207157 ) ) ;
#21088 = PRESENTATION_LAYER_ASSIGNMENT (  '', '', ( #9004 ) ) ;
#21089 = EDGE_CURVE ( 'NONE', #33874, #24889, #21512, .T. ) ;
#21090 = CARTESIAN_POINT ( 'NONE',  ( 3.828750298241973660, 16.99999999999997868, -23.23455841446276082 ) ) ;
#21091 = CARTESIAN_POINT ( 'NONE',  ( 32.50000000000000000, 71.10000000000000853, -10.55989012756945833 ) ) ;
#21092 = CARTESIAN_POINT ( 'NONE',  ( 10.37757302488624056, 16.52500000273120051, -31.93888565452638417 ) ) ;
#21093 = CARTESIAN_POINT ( 'NONE',  ( 23.41746824999999887, 0.6249999972688102812, 0.000000000000000000 ) ) ;
#21094 = CARTESIAN_POINT ( 'NONE',  ( 7.570916362186207671, 11.59999999999999964, 23.30088464923126779 ) ) ;
#21095 = CARTESIAN_POINT ( 'NONE',  ( 0.04044903255044120238, 16.14805583240936215, 27.95245687107223276 ) ) ;
#21096 = CARTESIAN_POINT ( 'NONE',  ( -32.50000000000000000, 38.50000000546237544, 0.000000000000000000 ) ) ;
#21097 = CARTESIAN_POINT ( 'NONE',  ( 24.50000000000000000, 17.84999999453762953, -7.960532557706203605 ) ) ;
#21098 = CARTESIAN_POINT ( 'NONE',  ( -33.58253175000000113, 23.12500000273118417, 0.000000000000000000 ) ) ;
#21099 = CARTESIAN_POINT ( 'NONE',  ( 13.97622843553589966, 47.09114583333332860, -24.20753774853756113 ) ) ;
#21100 = ORIENTED_EDGE ( 'NONE', *, *, #26669, .T. ) ;
#21101 = CARTESIAN_POINT ( 'NONE',  ( 33.58253175000000823, 62.02500000273116143, 10.91162601494192863 ) ) ;
#21102 = VERTEX_POINT ( 'NONE', #30703 ) ;
#21103 = CARTESIAN_POINT ( 'NONE',  ( -26.02091320914849959, 64.28423583425730214, 14.97647472619947528 ) ) ;
#21104 = CARTESIAN_POINT ( 'NONE',  ( -14.97647472619946285, 17.01861083425731280, -26.02091320914851025 ) ) ;
#21105 = CARTESIAN_POINT ( 'NONE',  ( -20.75514604977248823, 4.825000002731186122, -28.56700777964554305 ) ) ;
#21106 = CARTESIAN_POINT ( 'NONE',  ( 23.95873412499999944, 18.31249999863440792, 0.000000000000000000 ) ) ;
#21107 = CARTESIAN_POINT ( 'NONE',  ( -10.37757302488623701, 33.77500000273120406, 31.93888565452638417 ) ) ;
#21108 = AXIS2_PLACEMENT_3D ( 'NONE', #14073, #11823, #31911 ) ;
#21109 = CARTESIAN_POINT ( 'NONE',  ( -10.04305231718578462, 38.90000000546237402, 30.90933677959249337 ) ) ;
#21110 = CARTESIAN_POINT ( 'NONE',  ( -20.08610463437156923, 78.29999999999999716, 27.64615127144130113 ) ) ;
#21111 = CARTESIAN_POINT ( 'NONE',  ( 5.779280353836490358E-15, 48.50000000000000000, 32.49999999999999289 ) ) ;
#21112 = CARTESIAN_POINT ( 'NONE',  ( -15.00000000000000000, 82.00000000000001421, 0.000000000000000000 ) ) ;
#21113 = CARTESIAN_POINT ( 'NONE',  ( 6.486482029760649416E-15, 47.87500000273117706, 35.31076352940723240 ) ) ;
#21114 = EDGE_CURVE ( 'NONE', #25643, #11416, #13187, .T. ) ;
#21115 = CARTESIAN_POINT ( 'NONE',  ( 10.04305231718579705, 20.59999999999999432, 30.90933677959248982 ) ) ;
#21116 = CARTESIAN_POINT ( 'NONE',  ( -20.08610463437156923, 24.29999999999999005, 27.64615127144130113 ) ) ;
#21117 = CARTESIAN_POINT ( 'NONE',  ( 7.570916362186207671, 3.599999999999992095, 23.30088464923126779 ) ) ;
#21118 = CARTESIAN_POINT ( 'NONE',  ( -33.58253175000000113, 67.12500000273119838, 0.000000000000000000 ) ) ;
#21119 = CARTESIAN_POINT ( 'NONE',  ( -32.46390416700894122, 67.00000000000000000, -8.309214287527556309 ) ) ;
#21120 = CARTESIAN_POINT ( 'NONE',  ( 33.58253175000000113, 54.47500000273117138, -10.91162601494193574 ) ) ;
#21121 = EDGE_CURVE ( 'NONE', #32300, #10964, #30186, .T. ) ;
#21122 = DIRECTION ( 'NONE',  ( -1.000000000000000000, -1.224646799147353454E-16, 0.000000000000000000 ) ) ;
#21123 = CARTESIAN_POINT ( 'NONE',  ( -27.16883889988623935, 13.32500000273117990, 19.73931689729374739 ) ) ;
#21124 = CARTESIAN_POINT ( 'NONE',  ( 26.06988505166735592, 32.05767333425730214, 7.025853678916393896 ) ) ;
#21125 = CARTESIAN_POINT ( 'NONE',  ( 21.64573397815488676, 16.99999999999998579, 8.935324268693841887 ) ) ;
#21126 = DIRECTION ( 'NONE',  ( -1.224646799147353454E-16, 1.000000000000000000, -0.000000000000000000 ) ) ;
#21127 = CARTESIAN_POINT ( 'NONE',  ( -20.75514604977248823, 32.82500000273118701, -28.56700777964554305 ) ) ;
#21128 = DIRECTION ( 'NONE',  ( 0.000000000000000000, 0.000000000000000000, 1.000000000000000000 ) ) ;
#21129 = CARTESIAN_POINT ( 'NONE',  ( 0.000000000000000000, 16.99999999999998579, 0.000000000000000000 ) ) ;
#21130 = EDGE_CURVE ( 'NONE', #15118, #13792, #2218, .T. ) ;
#21131 = CARTESIAN_POINT ( 'NONE',  ( -11.25946833292375793, 77.07500000273121543, 8.180482586598737171 ) ) ;
#21132 = CARTESIAN_POINT ( 'NONE',  ( -7.543491769121917656, 45.22357666574267654, -28.00173670424536354 ) ) ;
#21133 = CARTESIAN_POINT ( 'NONE',  ( 20.08610463437157279, 51.80000000546238681, -27.64615127144129758 ) ) ;
#21134 =( GEOMETRIC_REPRESENTATION_CONTEXT ( 3 ) GLOBAL_UNCERTAINTY_ASSIGNED_CONTEXT ( ( #20492 ) ) GLOBAL_UNIT_ASSIGNED_CONTEXT ( ( #30879, #33283, #23169 ) ) REPRESENTATION_CONTEXT ( 'NONE', 'WORKASPACE' ) );
#21135 = CARTESIAN_POINT ( 'NONE',  ( 13.91746824999999532, 74.47500000273120691, -4.522059556121118540 ) ) ;
#21136 = CARTESIAN_POINT ( 'NONE',  ( 20.08610463437158344, 60.70000000000000284, 27.64615127144129403 ) ) ;
#21137 = CARTESIAN_POINT ( 'NONE',  ( 19.09188309203661049, 16.29687499999999645, -19.09188309203694445 ) ) ;
#21138 = CARTESIAN_POINT ( 'NONE',  ( -7.236395654485763274, 4.524999997268825069, 22.27133577429736633 ) ) ;
#21139 = CARTESIAN_POINT ( 'NONE',  ( 6.277390505771533514E-15, 69.00000000546239676, 34.17252228774368916 ) ) ;
#21140 = CARTESIAN_POINT ( 'NONE',  ( 15.01150461594643204, 24.17447916666666785, 26.00068869287340334 ) ) ;
#21141 = CARTESIAN_POINT ( 'NONE',  ( 10.37757302488624056, 26.77500000273118275, -31.93888565452638417 ) ) ;
#21142 = CARTESIAN_POINT ( 'NONE',  ( 7.236395654485760609, 15.52499999726880731, -22.27133577429736633 ) ) ;
#21143 = VERTEX_POINT ( 'NONE', #28142 ) ;
#21144 = CARTESIAN_POINT ( 'NONE',  ( 26.02091320914851025, 41.94048583425730925, -14.97647472619946463 ) ) ;
#21145 = CARTESIAN_POINT ( 'NONE',  ( -26.29305231718579350, 14.30000000546237438, -19.10302069950537884 ) ) ;
#21146 = CARTESIAN_POINT ( 'NONE',  ( -15.01150461594642138, 56.83072916666665009, -26.00068869287340334 ) ) ;
#21147 = CARTESIAN_POINT ( 'NONE',  ( 10.04305231718578817, 75.39999999999999147, -30.90933677959249337 ) ) ;
#21148 = CARTESIAN_POINT ( 'NONE',  ( 10.37757302488624056, 52.77500000273118985, -31.93888565452638417 ) ) ;
#21149 = CARTESIAN_POINT ( 'NONE',  ( 26.29305231718578995, 57.70000000546238539, -19.10302069950538240 ) ) ;
#21150 = CARTESIAN_POINT ( 'NONE',  ( 4.300734207923757602, 76.77500000273118985, -13.23629886949340673 ) ) ;
#21151 = CARTESIAN_POINT ( 'NONE',  ( -20.75514604977248112, 39.42500000273118843, 28.56700777964554661 ) ) ;
#21152 = CARTESIAN_POINT ( 'NONE',  ( 5.147494310547434893, 54.55125428154682510, 32.49999999999999289 ) ) ;
#21153 = CARTESIAN_POINT ( 'NONE',  ( -10.37757302488624411, 68.97500000273117848, -31.93888565452638417 ) ) ;
#21154 = CARTESIAN_POINT ( 'NONE',  ( 3.980102097228898626E-15, 80.00000000000001421, 32.50000000000000000 ) ) ;
#21155 = CARTESIAN_POINT ( 'NONE',  ( 27.16883889988623935, 60.32500000273120833, -19.73931689729374384 ) ) ;
#21156 = CARTESIAN_POINT ( 'NONE',  ( -30.02300923189239867, 18.44531249999999645, 2.654126918244514854E-13 ) ) ;
#21157 = COLOUR_RGB ( '', 0.31764706, 0.68627451, 0.89019608) ;
#21158 = CARTESIAN_POINT ( 'NONE',  ( -20.08610463437156923, 44.30000000000000426, 27.64615127144130113 ) ) ;
#21159 = CARTESIAN_POINT ( 'NONE',  ( -23.41746824999999887, 3.624999997268813168, -2.867812753649727150E-15 ) ) ;
#21160 = CARTESIAN_POINT ( 'NONE',  ( -20.75514604977248112, 13.67500000273118133, 28.56700777964554661 ) ) ;
#21161 = DIRECTION ( 'NONE',  ( -0.000000000000000000, 1.000000000000000000, -0.000000000000000000 ) ) ;
#21162 = CARTESIAN_POINT ( 'NONE',  ( -13.94119854578892514, 37.05951416574268364, 24.22776226481266448 ) ) ;
#21163 = CARTESIAN_POINT ( 'NONE',  ( -8.960552108402742093E-16, 72.87500000273115575, -14.63369212191046387 ) ) ;
#21164 = CARTESIAN_POINT ( 'NONE',  ( -27.16883889988623935, 77.57500000273121543, 19.73931689729374739 ) ) ;
#21165 = CARTESIAN_POINT ( 'NONE',  ( 3.000384657911015469E-15, 0.000000000000000000, -24.50000000000000000 ) ) ;
#21166 = CARTESIAN_POINT ( 'NONE',  ( -10.37757302488623701, 75.77500000273117564, 31.93888565452638417 ) ) ;
#21167 = ORIENTED_EDGE ( 'NONE', *, *, #17444, .T. ) ;
#21168 = DIRECTION ( 'NONE',  ( 0.000000000000000000, 0.000000000000000000, -1.000000000000000000 ) ) ;
#21169 = CARTESIAN_POINT ( 'NONE',  ( -13.97622843553588901, 55.68489583333332860, 24.20753774853756823 ) ) ;
#21170 = AXIS2_PLACEMENT_3D ( 'NONE', #12225, #33150, #20134 ) ;
#21171 = CARTESIAN_POINT ( 'NONE',  ( 20.75514604977248467, 56.42500000273120264, -28.56700777964554305 ) ) ;
#21172 = CARTESIAN_POINT ( 'NONE',  ( -33.58253175000000113, 19.37500000273119483, 0.000000000000000000 ) ) ;
#21173 = CARTESIAN_POINT ( 'NONE',  ( -20.75514604977248823, 3.075000002731183901, -28.56700777964554305 ) ) ;
#21174 = CARTESIAN_POINT ( 'NONE',  ( 6.988114217768294445, 41.50520833333333570, 26.07999730980477437 ) ) ;
#21175 = CARTESIAN_POINT ( 'NONE',  ( 0.04044903254992426173, 34.49256916759064495, -30.02300923189239867 ) ) ;
#21176 = CARTESIAN_POINT ( 'NONE',  ( 26.02091320914876960, 15.57513916574268720, 14.97647472619900455 ) ) ;
#21177 = CARTESIAN_POINT ( 'NONE',  ( -20.08610463437156923, 70.80000000546235128, 27.64615127144130113 ) ) ;
#21178 = CARTESIAN_POINT ( 'NONE',  ( 31.04172217648528687, 52.00000000000000711, 12.81397374188273908 ) ) ;
#21179 = CARTESIAN_POINT ( 'NONE',  ( -27.16883889988623935, 39.32500000273120122, 19.73931689729374739 ) ) ;
#21180 = CARTESIAN_POINT ( 'NONE',  ( -26.09010956794245217, 44.65065999907601935, -6.950374756619243755 ) ) ;
#21181 = CARTESIAN_POINT ( 'NONE',  ( -7.236395654485763274, 18.02499999726880731, 22.27133577429736633 ) ) ;
#21182 = DIRECTION ( 'NONE',  ( -1.224646799147353454E-16, 1.000000000000000000, -0.000000000000000000 ) ) ;
#21183 = ORIENTED_EDGE ( 'NONE', *, *, #12008, .T. ) ;
#21184 = CARTESIAN_POINT ( 'NONE',  ( 10.37757302488624056, 48.77500000273120406, -31.93888565452638417 ) ) ;
#21185 = CARTESIAN_POINT ( 'NONE',  ( 4.635254915624209993, 77.39999999999996305, -14.26584774442730463 ) ) ;
#21186 = CARTESIAN_POINT ( 'NONE',  ( 14.01125832528286352, 38.21652750092398065, -24.18731323226246843 ) ) ;
#21187 = CARTESIAN_POINT ( 'NONE',  ( 20.75514604977248467, 70.67500000273118133, -28.56700777964554305 ) ) ;
#21188 = ORIENTED_EDGE ( 'NONE', *, *, #19956, .T. ) ;
#21189 = CARTESIAN_POINT ( 'NONE',  ( 10.37757302488624767, 25.72500000273118914, 31.93888565452638417 ) ) ;
#21190 = CARTESIAN_POINT ( 'NONE',  ( 2.740863092043355209E-13, 21.02343749999999645, 30.02300923189239512 ) ) ;
#21191 = ORIENTED_EDGE ( 'NONE', *, *, #31502, .T. ) ;
#21192 = CARTESIAN_POINT ( 'NONE',  ( 2.205017735002230837E-13, 57.49999999999998579, -32.50000000000000000 ) ) ;
#21193 = CARTESIAN_POINT ( 'NONE',  ( -20.75514604977248112, 61.42500000273118133, 28.56700777964554661 ) ) ;
#21194 = CARTESIAN_POINT ( 'NONE',  ( -20.50609665441004736, 53.25000000000000000, -20.50609665440969565 ) ) ;
#21195 = CARTESIAN_POINT ( 'NONE',  ( -10.04305231718578462, 66.90000000546237402, 30.90933677959249337 ) ) ;
#21196 = CARTESIAN_POINT ( 'NONE',  ( 14.47279130897151944, 9.424999997268814766, -19.92008829642072598 ) ) ;
#21197 = CARTESIAN_POINT ( 'NONE',  ( -10.37757302488623701, 5.525000002731205839, 31.93888565452638417 ) ) ;
#21198 = CARTESIAN_POINT ( 'NONE',  ( 10.37757302488624767, 31.97500000273117848, 31.93888565452638417 ) ) ;
#21199 = CARTESIAN_POINT ( 'NONE',  ( 28.00173670424535644, 59.83295166574269075, -7.543491769121920321 ) ) ;
#21200 = CARTESIAN_POINT ( 'NONE',  ( -15.00000000000000000, 74.00000000000001421, 0.000000000000000000 ) ) ;
#21201 = DIRECTION ( 'NONE',  ( -0.000000000000000000, 1.000000000000000000, -0.000000000000000000 ) ) ;
#21202 = CARTESIAN_POINT ( 'NONE',  ( -10.04305231718578462, 60.39999999999999858, 30.90933677959249337 ) ) ;
#21203 = CARTESIAN_POINT ( 'NONE',  ( -26.29305231718579350, 19.79999999999999716, -19.10302069950537884 ) ) ;
#21204 = CARTESIAN_POINT ( 'NONE',  ( 13.97622843553633842, 58.54947916666666430, 24.20753774853730889 ) ) ;
#21205 = CARTESIAN_POINT ( 'NONE',  ( 18.94512977948575738, 2.924999997268806773, 13.76444248337723408 ) ) ;
#21206 = CARTESIAN_POINT ( 'NONE',  ( -13.91746824999999532, 78.97500000273117848, 4.522059556121122093 ) ) ;
#21207 = CARTESIAN_POINT ( 'NONE',  ( -26.07999730980490583, 35.77604166666666430, -6.988114217767815717 ) ) ;
#21208 = CARTESIAN_POINT ( 'NONE',  ( -20.75514604977248112, 25.42500000273119198, 28.56700777964554661 ) ) ;
#21209 = CARTESIAN_POINT ( 'NONE',  ( 10.37757302488624056, 72.52500000273118985, -31.93888565452638417 ) ) ;
#21210 = CARTESIAN_POINT ( 'NONE',  ( 10.37757302488624767, 35.97500000273119980, 31.93888565452638417 ) ) ;
#21211 = CARTESIAN_POINT ( 'NONE',  ( 27.16883889988624290, 16.17500000273119909, 19.73931689729373673 ) ) ;
#21212 = CARTESIAN_POINT ( 'NONE',  ( 0.000000000000000000, 0.000000000000000000, 0.000000000000000000 ) ) ;
#21213 = CARTESIAN_POINT ( 'NONE',  ( -27.95245687107223986, 57.69569416759065206, -0.04044903254993292840 ) ) ;
#21214 = CARTESIAN_POINT ( 'NONE',  ( 20.75514604977248467, 68.42500000273120975, -28.56700777964554305 ) ) ;
#21215 = LINE ( 'NONE', #8818, #32168 ) ;
#21216 = ADVANCED_FACE ( 'NONE', ( #4628 ), #22317, .F. ) ;
#21217 = CARTESIAN_POINT ( 'NONE',  ( -26.29305231718578995, 56.20000000000001705, 19.10302069950538595 ) ) ;
#21218 = LINE ( 'NONE', #5925, #18836 ) ;
#21219 = CARTESIAN_POINT ( 'NONE',  ( -27.16883889988623935, 59.32500000273119412, 19.73931689729374739 ) ) ;
#21220 = EDGE_CURVE ( 'NONE', #27572, #13970, #27211, .T. ) ;
#21221 = CARTESIAN_POINT ( 'NONE',  ( 7.236395654485760609, 7.524999997268827734, -22.27133577429736633 ) ) ;
#21222 = AXIS2_PLACEMENT_3D ( 'NONE', #18174, #8195, #28617 ) ;
#21223 = ORIENTED_EDGE ( 'NONE', *, *, #846, .F. ) ;
#21224 = CARTESIAN_POINT ( 'NONE',  ( 10.37757302488624056, 72.77500000273118985, -31.93888565452638417 ) ) ;
#21225 = CARTESIAN_POINT ( 'NONE',  ( -14.47279130897152122, 1.924999997268818541, 19.92008829642072243 ) ) ;
#21226 = CARTESIAN_POINT ( 'NONE',  ( -13.94119854578936923, 13.58111083425730925, -24.22776226481241224 ) ) ;
#21227 = ORIENTED_EDGE ( 'NONE', *, *, #32716, .T. ) ;
#21228 = CIRCLE ( 'NONE', #7519, 10.11000150615022264 ) ;
#21229 = CARTESIAN_POINT ( 'NONE',  ( -27.16883889988623935, 43.32500000273119412, 19.73931689729374739 ) ) ;
#21230 = CARTESIAN_POINT ( 'NONE',  ( 0.000000000000000000, 122.0000000000000000, 0.000000000000000000 ) ) ;
#21231 = VERTEX_POINT ( 'NONE', #10804 ) ;
#21232 = CARTESIAN_POINT ( 'NONE',  ( 15.01150461594643204, 44.79947916666667140, 26.00068869287340334 ) ) ;
#21233 = CARTESIAN_POINT ( 'NONE',  ( -11.66012699757880355, 66.98735890369596291, -31.52215860731681119 ) ) ;
#21234 = CARTESIAN_POINT ( 'NONE',  ( 10.04305231718579705, 7.100000005462389296, 30.90933677959248982 ) ) ;
#21235 = CARTESIAN_POINT ( 'NONE',  ( -32.50000000000000000, 80.00000000000001421, 0.000000000000000000 ) ) ;
#21236 = CARTESIAN_POINT ( 'NONE',  ( -26.00068869287340334, 18.15885416666666075, 15.01150461594643382 ) ) ;
#21237 = CARTESIAN_POINT ( 'NONE',  ( 23.41746825000000243, 18.52499999726881441, 7.608796670333735079 ) ) ;
#21238 = CARTESIAN_POINT ( 'NONE',  ( 33.58253175000000113, 10.37500000273117173, -4.112674001490185761E-15 ) ) ;
#21239 = CARTESIAN_POINT ( 'NONE',  ( -32.50000000000000000, 59.89999999999999858, -10.55989012756945478 ) ) ;
#21240 = CARTESIAN_POINT ( 'NONE',  ( -13.91746824999999532, 76.77500000273117564, -4.522059556121115875 ) ) ;
#21241 = CARTESIAN_POINT ( 'NONE',  ( 5.779280353836490358E-15, 73.00000000546236834, 32.49999999999999289 ) ) ;
#21242 = CARTESIAN_POINT ( 'NONE',  ( -25.98046417659831420, 30.47097249907602290, 15.04653450569339945 ) ) ;
#21243 = CARTESIAN_POINT ( 'NONE',  ( 4.300734207923757602, 74.77500000273118985, -13.23629886949340673 ) ) ;
#21244 = CARTESIAN_POINT ( 'NONE',  ( -15.01150461594642316, 53.39322916666665719, -26.00068869287341045 ) ) ;
#21245 = APPLICATION_PROTOCOL_DEFINITION ( 'draft international standard', 'automotive_design', 1998, #7454 ) ;
#21246 = CARTESIAN_POINT ( 'NONE',  ( 0.000000000000000000, 80.00000000000001421, 0.000000000000000000 ) ) ;
#21247 = CARTESIAN_POINT ( 'NONE',  ( 5.147494310547380714, 64.55125428154683220, 32.50000000000002132 ) ) ;
#21248 = CARTESIAN_POINT ( 'NONE',  ( 6.277390505771533514E-15, 4.500000000000003553, 34.17252228774368916 ) ) ;
#21249 = CARTESIAN_POINT ( 'NONE',  ( -4.635254915624211769, 73.59999999999999432, -14.26584774442730286 ) ) ;
#21250 = CARTESIAN_POINT ( 'NONE',  ( -13.94119854578892514, 64.55951416574268364, 24.22776226481266448 ) ) ;
#21251 = CARTESIAN_POINT ( 'NONE',  ( 10.37757302488624767, 41.72500000273118559, 31.93888565452638417 ) ) ;
#21252 = CARTESIAN_POINT ( 'NONE',  ( -4.300734207923759378, 80.47500000273116427, -13.23629886949340495 ) ) ;
#21253 = CARTESIAN_POINT ( 'NONE',  ( -33.58253175000000113, 55.37500000273119838, 0.000000000000000000 ) ) ;
#21254 = CARTESIAN_POINT ( 'NONE',  ( 6.486482029760648627E-15, 35.87500000273117706, 35.31076352940722529 ) ) ;
#21255 = CARTESIAN_POINT ( 'NONE',  ( -30.00000000000000000, -91.00000000000000000, 0.000000000000000000 ) ) ;
#21256 = CARTESIAN_POINT ( 'NONE',  ( 19.09188309203661049, 19.73437500000000000, -19.09188309203694445 ) ) ;
#21257 = CARTESIAN_POINT ( 'NONE',  ( -1.778240108872766143E-15, 55.49999999999999289, -32.49999999999999289 ) ) ;
#21258 = CARTESIAN_POINT ( 'NONE',  ( -4.480168651474261132, 16.99999999999998579, -23.39706153295998448 ) ) ;
#21259 = CARTESIAN_POINT ( 'NONE',  ( -26.29305231718579350, 73.80000000000001137, -19.10302069950537884 ) ) ;
#21260 = CARTESIAN_POINT ( 'NONE',  ( 33.58253175000000113, 16.22500000273118914, -10.91162601494193751 ) ) ;
#21261 = CARTESIAN_POINT ( 'NONE',  ( -23.41746824999999887, 7.524999997268816188, -7.608796670333730638 ) ) ;
#21262 = CARTESIAN_POINT ( 'NONE',  ( -32.50000000000000000, 40.09999999999998721, 10.55989012756946366 ) ) ;
#21263 = CARTESIAN_POINT ( 'NONE',  ( 0.04044903255044120238, 23.02305583240935860, 27.95245687107223276 ) ) ;
#21264 = EDGE_CURVE ( 'NONE', #4440, #28702, #33971, .T. ) ;
#21265 = CARTESIAN_POINT ( 'NONE',  ( 32.50000000000000000, 35.50000000546236834, -3.980102097228898626E-15 ) ) ;
#21266 = EDGE_CURVE ( 'NONE', #33755, #15317, #24997, .T. ) ;
#21267 = CARTESIAN_POINT ( 'NONE',  ( -32.50000000000000000, 12.09999999999999609, 10.55989012756946366 ) ) ;
#21268 = CARTESIAN_POINT ( 'NONE',  ( 20.75514604977248467, 22.42500000273119909, -28.56700777964554305 ) ) ;
#21269 = CARTESIAN_POINT ( 'NONE',  ( 13.97622843553633665, 44.79947916666667140, 24.20753774853730889 ) ) ;
#21270 = EDGE_LOOP ( 'NONE', ( #27873, #26577, #24583, #28086 ) ) ;
#21271 = CARTESIAN_POINT ( 'NONE',  ( 10.37757302488624767, 65.72500000273119269, 31.93888565452638417 ) ) ;
#21272 = VERTEX_POINT ( 'NONE', #15451 ) ;
#21273 = CARTESIAN_POINT ( 'NONE',  ( 28.01184896238304134, 13.43229166666666607, 7.505752307972846538 ) ) ;
#21274 = CARTESIAN_POINT ( 'NONE',  ( -20.53372385742071771, 16.01600666759064140, 20.47846945139902530 ) ) ;
#21275 = CARTESIAN_POINT ( 'NONE',  ( 27.16883889988624290, 5.925000002731190207, 19.73931689729373673 ) ) ;
#21276 = EDGE_CURVE ( 'NONE', #17032, #23750, #28511, .T. ) ;
#21277 = ORIENTED_EDGE ( 'NONE', *, *, #28647, .F. ) ;
#21278 = DIRECTION ( 'NONE',  ( 0.000000000000000000, -1.000000000000000000, 0.000000000000000000 ) ) ;
#21279 = CARTESIAN_POINT ( 'NONE',  ( 33.58253175000000823, 26.27500000273119340, 10.91162601494192863 ) ) ;
#21280 = CIRCLE ( 'NONE', #13609, 1.500000000000008216 ) ;
#21281 = CARTESIAN_POINT ( 'NONE',  ( -2.092463501923844636E-15, 38.00000000546237544, -34.17252228774368916 ) ) ;
#21282 = CARTESIAN_POINT ( 'NONE',  ( -26.29305231718578995, 76.19999999999998863, 19.10302069950538595 ) ) ;
#21283 = CARTESIAN_POINT ( 'NONE',  ( 5.147494310547327423, 52.55125428154685352, 32.50000000000003553 ) ) ;
#21284 = CARTESIAN_POINT ( 'NONE',  ( -4.223320258572819786E-15, 5.249999994537622783, 24.50000000000000000 ) ) ;
#21285 = CARTESIAN_POINT ( 'NONE',  ( -27.16883889988623935, 43.57500000273117990, 19.73931689729374739 ) ) ;
#21286 =( NAMED_UNIT ( * ) PLANE_ANGLE_UNIT ( ) SI_UNIT ( $, .RADIAN. ) );
#21287 = CARTESIAN_POINT ( 'NONE',  ( 32.50000000000000000, 23.00000000000000711, -3.980102097228898626E-15 ) ) ;
#21288 = CARTESIAN_POINT ( 'NONE',  ( 32.50000000000000000, 21.10000000000000142, -10.55989012756945833 ) ) ;
#21289 = CARTESIAN_POINT ( 'NONE',  ( -19.82091636218621034, 4.799999999999998934, -14.40073868116559552 ) ) ;
#21290 = CARTESIAN_POINT ( 'NONE',  ( -27.16883889988624290, 64.92500000273118133, -19.73931689729374028 ) ) ;
#21291 = CARTESIAN_POINT ( 'NONE',  ( -21.77128556259171788, 66.99999999999998579, 24.67464075869981244 ) ) ;
#21292 = CARTESIAN_POINT ( 'NONE',  ( -2.111130048464370024, 74.00000000000002842, -14.50686135258029630 ) ) ;
#21293 = CARTESIAN_POINT ( 'NONE',  ( -27.16883889988623935, 55.57500000273118701, 19.73931689729374739 ) ) ;
#21294 = CARTESIAN_POINT ( 'NONE',  ( 14.47279130897151767, 4.324999997268800911, 19.92008829642072953 ) ) ;
#21295 = DIRECTION ( 'NONE',  ( 0.000000000000000000, -0.000000000000000000, 1.000000000000000000 ) ) ;
#21296 = CARTESIAN_POINT ( 'NONE',  ( 33.58253175000000113, 14.22500000273119625, -10.91162601494193751 ) ) ;
#21297 = CARTESIAN_POINT ( 'NONE',  ( -7.025853678916393008, 32.91704833425729504, 26.06988505166735592 ) ) ;
#21298 = CARTESIAN_POINT ( 'NONE',  ( 3.880418787951141812, 2.198745712990784806, -24.50000000000000000 ) ) ;
#21299 = DIRECTION ( 'NONE',  ( -1.000000000000000000, 0.000000000000000000, 0.000000000000000000 ) ) ;
#21300 = CARTESIAN_POINT ( 'NONE',  ( 27.16883889988623935, 36.32500000273118701, -19.73931689729374384 ) ) ;
#21301 = CARTESIAN_POINT ( 'NONE',  ( -32.50000000000000000, 18.40000000546238823, -10.55989012756945300 ) ) ;
#21302 = DIRECTION ( 'NONE',  ( -0.8660254037844388186, 0.000000000000000000, -0.4999999999999996669 ) ) ;
#21303 = CARTESIAN_POINT ( 'NONE',  ( -4.300734207923755825, 79.27500000273118985, 13.23629886949340673 ) ) ;
#21304 = CARTESIAN_POINT ( 'NONE',  ( 25.98046417659831775, 42.50222249907603356, -15.04653450569338879 ) ) ;
#21305 = CARTESIAN_POINT ( 'NONE',  ( -2.092463501923844636E-15, 54.00000000546236834, -34.17252228774368916 ) ) ;
#21306 = CARTESIAN_POINT ( 'NONE',  ( 11.25946833292375793, 74.17500000273119554, 8.180482586598731842 ) ) ;
#21307 = CARTESIAN_POINT ( 'NONE',  ( -19.09188309203660694, 18.01562499999999645, 19.09188309203694800 ) ) ;
#21308 = CARTESIAN_POINT ( 'NONE',  ( -10.04305231718578462, 66.90000000546237402, 30.90933677959249337 ) ) ;
#21309 = CARTESIAN_POINT ( 'NONE',  ( -30.02300923189239512, 21.88281249999999645, 2.654126918244515359E-13 ) ) ;
#21310 = CARTESIAN_POINT ( 'NONE',  ( 20.75514604977249178, 26.07500000273119767, 28.56700777964553950 ) ) ;
#21311 = CARTESIAN_POINT ( 'NONE',  ( -23.41746825000000243, 12.22499999726881370, 7.608796670333725309 ) ) ;
#21312 = ORIENTED_EDGE ( 'NONE', *, *, #15884, .T. ) ;
#21313 = CARTESIAN_POINT ( 'NONE',  ( -7.543491769121417612, 39.79204833425731636, 28.00173670424549499 ) ) ;
#21314 = CARTESIAN_POINT ( 'NONE',  ( -20.08610463437157989, 14.20000000546237295, -27.64615127144129758 ) ) ;
#21315 = CARTESIAN_POINT ( 'NONE',  ( 28.01184896238290278, 54.39583333333332860, -7.505752307973347470 ) ) ;
#21316 = CARTESIAN_POINT ( 'NONE',  ( -27.16883889988623935, 51.57500000273118701, 19.73931689729374739 ) ) ;
#21317 = CARTESIAN_POINT ( 'NONE',  ( 26.29305231718579350, 57.30000000546237260, 19.10302069950537529 ) ) ;
#21318 =( BOUNDED_CURVE ( )  B_SPLINE_CURVE ( 2, ( #9731, #27585, #4413, #4586, #27756, #17295, #14890 ),
 .UNSPECIFIED., .F., .T. ) 
 B_SPLINE_CURVE_WITH_KNOTS ( ( 3, 2, 2, 3 ),
 ( 0.1666666666666667962, 0.1692307692307693234, 0.1717948717948718229, 0.1730769230769230727 ),
 .UNSPECIFIED. ) 
 CURVE ( )  GEOMETRIC_REPRESENTATION_ITEM ( )  RATIONAL_B_SPLINE_CURVE ( ( 0.9999999999999974465, 0.9510565162951561957, 1.000000000000000000, 0.9510565162951535312, 1.000000000000000000, 0.9755282581475768211, 0.9755282581475768211 ) ) 
 REPRESENTATION_ITEM ( '' )  );
#21319 = CARTESIAN_POINT ( 'NONE',  ( 13.91746825000000065, 76.27500000273116143, 4.522059556121114987 ) ) ;
#21320 = CARTESIAN_POINT ( 'NONE',  ( 33.58253175000000113, 38.22500000273119269, -10.91162601494193751 ) ) ;
#21321 = CARTESIAN_POINT ( 'NONE',  ( 12.13525491562421088, 73.05000000546237970, 8.816778784387095058 ) ) ;
#21322 = CARTESIAN_POINT ( 'NONE',  ( -20.75514604977248823, 61.07500000273119412, -28.56700777964554305 ) ) ;
#21323 = CARTESIAN_POINT ( 'NONE',  ( 10.37757302488624056, 52.52500000273117564, -31.93888565452638417 ) ) ;
#21324 = CARTESIAN_POINT ( 'NONE',  ( 26.00068869287367690, 23.88802083333332504, 15.01150461594596486 ) ) ;
#21325 = CARTESIAN_POINT ( 'NONE',  ( 32.50000000000000000, 41.00000000000000711, -3.980102097228898626E-15 ) ) ;
#21326 = CARTESIAN_POINT ( 'NONE',  ( -18.94512977948576093, 3.824999997268818674, 13.76444248337722698 ) ) ;
#21327 = CARTESIAN_POINT ( 'NONE',  ( -27.16883889988624290, 11.17500000273119554, -19.73931689729374028 ) ) ;
#21328 = DIRECTION ( 'NONE',  ( 0.000000000000000000, 1.000000000000000000, 0.000000000000000000 ) ) ;
#21329 = CARTESIAN_POINT ( 'NONE',  ( -7.025853678916861966, 38.34857666574267654, -26.06988505166722803 ) ) ;
#21330 = CARTESIAN_POINT ( 'NONE',  ( 6.054684311146244891E-15, -72.44024934668307480, 0.000000000000000000 ) ) ;
#21331 = CARTESIAN_POINT ( 'NONE',  ( -2.162160676586882350E-15, 74.87500000273116996, -35.31076352940722529 ) ) ;
#21332 = DIRECTION ( 'NONE',  ( 0.000000000000000000, 0.000000000000000000, 1.000000000000000000 ) ) ;
#21333 = CARTESIAN_POINT ( 'NONE',  ( 10.37757302488624056, 66.77500000273118985, -31.93888565452638417 ) ) ;
#21334 = VERTEX_POINT ( 'NONE', #13202 ) ;
#21335 = CARTESIAN_POINT ( 'NONE',  ( 1.555960095263670572E-15, 14.24999999453762278, -24.50000000000000000 ) ) ;
#21336 = CARTESIAN_POINT ( 'NONE',  ( 26.07999730980490227, 61.55729166666666430, 6.988114217767821046 ) ) ;
#21337 = CARTESIAN_POINT ( 'NONE',  ( 20.75514604977249178, 53.82500000273119412, 28.56700777964553950 ) ) ;
#21338 = CARTESIAN_POINT ( 'NONE',  ( 10.37757302488624056, 16.77500000273117564, -31.93888565452638417 ) ) ;
#21339 = CARTESIAN_POINT ( 'NONE',  ( -10.37757302488624411, 78.72500000273117848, -31.93888565452638417 ) ) ;
#21340 = CARTESIAN_POINT ( 'NONE',  ( 26.07999730980490227, 44.36979166666666430, 6.988114217767821046 ) ) ;
#21341 = CARTESIAN_POINT ( 'NONE',  ( 28.02196122052045268, 31.77121500092397000, -7.468012846824774620 ) ) ;
#21342 = CARTESIAN_POINT ( 'NONE',  ( -14.97647472619899389, 23.30951416574269075, 26.02091320914878025 ) ) ;
#21343 = CARTESIAN_POINT ( 'NONE',  ( -20.08610463437156923, 76.80000000546239391, 27.64615127144130113 ) ) ;
#21344 = EDGE_CURVE ( 'NONE', #12209, #8211, #7261, .T. ) ;
#21345 = CARTESIAN_POINT ( 'NONE',  ( 29.06502868860493294, 52.00000000000000000, -15.87274502311855251 ) ) ;
#21346 = CARTESIAN_POINT ( 'NONE',  ( -10.37757302488624411, 36.72500000273118559, -31.93888565452638417 ) ) ;
#21347 = CARTESIAN_POINT ( 'NONE',  ( -26.06988505166722803, 47.80170166574269786, 7.025853678916877953 ) ) ;
#21348 = CARTESIAN_POINT ( 'NONE',  ( -4.523095164977116484E-15, 14.12499999726881050, 24.62258325217400312 ) ) ;
#21349 = CARTESIAN_POINT ( 'NONE',  ( -20.08610463437156923, 2.800000005462385921, 27.64615127144130113 ) ) ;
#21350 = ORIENTED_EDGE ( 'NONE', *, *, #10080, .T. ) ;
#21351 = CARTESIAN_POINT ( 'NONE',  ( 20.75514604977248467, 48.67500000273117422, -28.56700777964554305 ) ) ;
#21352 = CARTESIAN_POINT ( 'NONE',  ( 26.50000000000000000, -15.84529946162074943, 0.000000000000000000 ) ) ;
#21353 = CARTESIAN_POINT ( 'NONE',  ( 24.18731323226247554, 49.38840250092398776, 14.01125832528285997 ) ) ;
#21354 = CARTESIAN_POINT ( 'NONE',  ( 33.58253175000000113, 66.37500000273119838, -4.112674001490185761E-15 ) ) ;
#21355 = ORIENTED_EDGE ( 'NONE', *, *, #11443, .F. ) ;
#21356 = CARTESIAN_POINT ( 'NONE',  ( -27.16883889988624290, 18.92500000273118843, -19.73931689729374028 ) ) ;
#21357 = CARTESIAN_POINT ( 'NONE',  ( -26.00068869287368756, 25.60677083333332149, -15.01150461594595775 ) ) ;
#21358 = ORIENTED_EDGE ( 'NONE', *, *, #757, .F. ) ;
#21359 = CARTESIAN_POINT ( 'NONE',  ( -24.50000000000000000, 2.749999994537621895, -3.000384657911015469E-15 ) ) ;
#21360 = CARTESIAN_POINT ( 'NONE',  ( 33.58253175000000113, 52.12500000273118417, -4.112674001490185761E-15 ) ) ;
#21361 = CARTESIAN_POINT ( 'NONE',  ( 7.505752307972854531, 46.94791666666666430, -28.01184896238303423 ) ) ;
#21362 = CARTESIAN_POINT ( 'NONE',  ( 20.08610463437158344, 21.20000000546238894, 27.64615127144129403 ) ) ;
#21363 = CARTESIAN_POINT ( 'NONE',  ( -19.82091636218621389, 6.949999994537630954, 14.40073868116558842 ) ) ;
#21364 = CARTESIAN_POINT ( 'NONE',  ( 1.507698388325705758E-15, 7.624999997268813168, -24.62258325217400312 ) ) ;
#21365 = CARTESIAN_POINT ( 'NONE',  ( 33.58253175000000113, 30.37500000273119127, -4.112674001490185761E-15 ) ) ;
#21366 = CARTESIAN_POINT ( 'NONE',  ( -7.543491769121917656, 62.41107666574269075, -28.00173670424536354 ) ) ;
#21367 = CARTESIAN_POINT ( 'NONE',  ( -15.14183272437242778, 15.30000000000001137, 20.84094480462497856 ) ) ;
#21368 = CARTESIAN_POINT ( 'NONE',  ( -4.934616302121927505E-14, 72.50000000000001421, 32.50000000000000000 ) ) ;
#21369 = CARTESIAN_POINT ( 'NONE',  ( 32.50000000000000000, 9.100000000000003197, -10.55989012756945833 ) ) ;
#21370 = CARTESIAN_POINT ( 'NONE',  ( -32.50000000000000000, 11.99999999999999645, 0.000000000000000000 ) ) ;
#21371 = CARTESIAN_POINT ( 'NONE',  ( -6.988114217768288228, 56.97395833333333570, -26.07999730980477437 ) ) ;
#21372 = CARTESIAN_POINT ( 'NONE',  ( 1.577395562988744260E-15, 18.24999999453762101, -25.76082449383753925 ) ) ;
#21373 = CARTESIAN_POINT ( 'NONE',  ( -13.91746824999999887, 72.87500000273119838, 0.000000000000000000 ) ) ;
#21374 = CARTESIAN_POINT ( 'NONE',  ( 26.07999730980477437, 33.77083333333333570, -6.988114217768290004 ) ) ;
#21375 = CARTESIAN_POINT ( 'NONE',  ( -27.16883889988623935, 27.32500000273119412, 19.73931689729374739 ) ) ;
#21376 = CARTESIAN_POINT ( 'NONE',  ( -2.162160676586881955E-15, 74.62500000273116996, -35.31076352940723240 ) ) ;
#21377 = CARTESIAN_POINT ( 'NONE',  ( 27.16883889988624290, 38.17500000273120264, 19.73931689729373673 ) ) ;
#21378 = CARTESIAN_POINT ( 'NONE',  ( 27.16883889988623935, 16.57500000273118346, -19.73931689729374384 ) ) ;
#21379 = CARTESIAN_POINT ( 'NONE',  ( -24.18731323226248264, 57.98215250092397355, -14.01125832528284931 ) ) ;
#21380 = CARTESIAN_POINT ( 'NONE',  ( -27.16883889988624290, 70.92500000273119554, -19.73931689729374028 ) ) ;
#21381 = DIRECTION ( 'NONE',  ( -0.000000000000000000, -1.000000000000000000, -0.000000000000000000 ) ) ;
#21382 = CARTESIAN_POINT ( 'NONE',  ( 10.04305231718578817, 55.39999999999999147, -30.90933677959249337 ) ) ;
#21383 = CARTESIAN_POINT ( 'NONE',  ( 2.375766604868043697, 78.80125428700924317, 15.00000000000000178 ) ) ;
#21384 = CARTESIAN_POINT ( 'NONE',  ( 33.58253175000000113, 58.22500000273117138, -10.91162601494193574 ) ) ;
#21385 = CARTESIAN_POINT ( 'NONE',  ( 1.507698388325705758E-15, 17.62499999726881938, -24.62258325217400312 ) ) ;
#21386 = ORIENTED_EDGE ( 'NONE', *, *, #15037, .F. ) ;
#21387 = CARTESIAN_POINT ( 'NONE',  ( -10.37757302488624411, 64.97500000273119269, -31.93888565452638417 ) ) ;
#21388 = CARTESIAN_POINT ( 'NONE',  ( 20.75514604977249178, 1.825000002731179460, 28.56700777964553950 ) ) ;
#21389 = CARTESIAN_POINT ( 'NONE',  ( -4.523095164977116484E-15, 4.124999997268806951, 24.62258325217400312 ) ) ;
#21390 = CARTESIAN_POINT ( 'NONE',  ( -24.22776226481240514, 23.03423583425731280, 13.94119854578937812 ) ) ;
#21391 = VERTEX_POINT ( 'NONE', #10634 ) ;
#21392 = CARTESIAN_POINT ( 'NONE',  ( 27.16883889988624290, 39.92500000273118133, 19.73931689729373673 ) ) ;
#21393 = CARTESIAN_POINT ( 'NONE',  ( -15.14183272437242067, 0.7000000000000070610, -20.84094480462497856 ) ) ;
#21394 = ORIENTED_EDGE ( 'NONE', *, *, #28858, .F. ) ;
#21395 = CARTESIAN_POINT ( 'NONE',  ( -7.505752307973343918, 46.66145833333332860, -28.01184896238290989 ) ) ;
#21396 = CARTESIAN_POINT ( 'NONE',  ( -10.04305231718578462, 60.90000000546237402, 30.90933677959249337 ) ) ;
#21397 = CARTESIAN_POINT ( 'NONE',  ( -4.223320258572819786E-15, 19.24999999453763166, 24.50000000000000000 ) ) ;
#21398 = CARTESIAN_POINT ( 'NONE',  ( 10.04305231718578817, 27.90000000546238823, -30.90933677959249337 ) ) ;
#21399 = CARTESIAN_POINT ( 'NONE',  ( 7.505752307973351023, 20.88020833333333215, 28.01184896238290278 ) ) ;
#21400 = CARTESIAN_POINT ( 'NONE',  ( -24.50000000000001066, 1.099999999999994094, 7.960532557706201828 ) ) ;
#21401 = CARTESIAN_POINT ( 'NONE',  ( -2.162160676586881955E-15, 8.875000002731189497, -35.31076352940723240 ) ) ;
#21402 = EDGE_CURVE ( 'NONE', #29266, #927, #14087, .T. ) ;
#21403 = CARTESIAN_POINT ( 'NONE',  ( 20.08610463437158344, 58.70000000000000995, 27.64615127144129403 ) ) ;
#21404 = CARTESIAN_POINT ( 'NONE',  ( 11.25946833292375793, 77.67500000273119554, 8.180482586598731842 ) ) ;
#21405 = CARTESIAN_POINT ( 'NONE',  ( 5.779280353836490358E-15, 55.00000000546238965, 32.49999999999999289 ) ) ;
#21406 = CARTESIAN_POINT ( 'NONE',  ( -25.98046417659831420, 33.90847249907601935, 15.04653450569339945 ) ) ;
#21407 = CARTESIAN_POINT ( 'NONE',  ( 11.25946833292375793, 76.17500000273119554, 8.180482586598731842 ) ) ;
#21408 = CARTESIAN_POINT ( 'NONE',  ( 20.50609665441005092, 51.53124999999999289, 20.50609665440969209 ) ) ;
#21409 = EDGE_CURVE ( 'NONE', #10580, #6717, #31222, .T. ) ;
#21410 = LINE ( 'NONE', #5616, #19563 ) ;
#21411 = CARTESIAN_POINT ( 'NONE',  ( 6.001560367445586717E-15, 1.500000000000005995, 24.50000000000000000 ) ) ;
#21412 = CARTESIAN_POINT ( 'NONE',  ( 32.50000000000000000, 5.000000000000004441, -3.980102097228898626E-15 ) ) ;
#21413 = CARTESIAN_POINT ( 'NONE',  ( 20.08610463437158344, 49.20000000546237118, 27.64615127144129403 ) ) ;
#21414 = CARTESIAN_POINT ( 'NONE',  ( -19.11951029504797006, 58.68711833240935505, -19.06425588902558133 ) ) ;
#21415 = CARTESIAN_POINT ( 'NONE',  ( 33.58253175000000113, 42.22500000273118559, -10.91162601494193751 ) ) ;
#21416 = CARTESIAN_POINT ( 'NONE',  ( -15.00000000000000000, 72.15000000546238823, -4.873795443493594171 ) ) ;
#21417 = CARTESIAN_POINT ( 'NONE',  ( 10.37757302488624767, 57.97500000273118559, 31.93888565452638417 ) ) ;
#21418 = CARTESIAN_POINT ( 'NONE',  ( -33.58253175000000113, 37.37500000273119838, 0.000000000000000000 ) ) ;
#21419 =( BOUNDED_CURVE ( )  B_SPLINE_CURVE ( 2, ( #16180, #2623, #18919, #13086, #29365, #5865, #13428, #23896, #26799, #23560, #24, #5702, #10513 ),
 .UNSPECIFIED., .F., .F. ) 
 B_SPLINE_CURVE_WITH_KNOTS ( ( 3, 2, 2, 2, 2, 2, 3 ),
 ( 0.1474358975042141251, 0.1487179487179487170, 0.1512820512820512719, 0.1538461538461538547, 0.1564102564102564097, 0.1589743589743589647, 0.1602564102564102699 ),
 .UNSPECIFIED. ) 
 CURVE ( )  GEOMETRIC_REPRESENTATION_ITEM ( )  RATIONAL_B_SPLINE_CURVE ( ( 0.9755282581475768211, 0.9755282594516028194, 1.000000000000000000, 0.9510565162951535312, 1.000000000000000000, 0.9510565162951535312, 1.000000000000000000, 0.9510565162951535312, 1.000000000000000000, 0.9510565162951535312, 1.000000000000000000, 0.9755282581475764880, 0.9755282581475768211 ) ) 
 REPRESENTATION_ITEM ( '' )  );
#21420 = CARTESIAN_POINT ( 'NONE',  ( -4.223320258572821363E-15, 80.50000000000000000, 15.00000000000000355 ) ) ;
#21421 = CARTESIAN_POINT ( 'NONE',  ( 6.988114217767829928, 26.32291666666666075, -26.07999730980489872 ) ) ;
#21422 = LINE ( 'NONE', #21757, #1520 ) ;
#21423 = CARTESIAN_POINT ( 'NONE',  ( 5.147494310547426899, 31.44874571845313582, -32.50000000000000000 ) ) ;
#21424 =( BOUNDED_CURVE ( )  B_SPLINE_CURVE ( 2, ( #27034, #939, #14001, #21894, #19321, #14841, #9170, #19654, #22554, #16912, #27540, #1779, #9687 ),
 .UNSPECIFIED., .F., .T. ) 
 B_SPLINE_CURVE_WITH_KNOTS ( ( 3, 2, 2, 2, 2, 2, 3 ),
 ( 0.1089743589743589758, 0.1102564102564102533, 0.1128205128205128221, 0.1153846153846153910, 0.1179487179487179460, 0.1205128205128205149, 0.1217948717948718063 ),
 .UNSPECIFIED. ) 
 CURVE ( )  GEOMETRIC_REPRESENTATION_ITEM ( )  RATIONAL_B_SPLINE_CURVE ( ( 0.9755282581475768211, 0.9755282581475768211, 1.000000000000000000, 0.9510565162951535312, 1.000000000000000000, 0.9510565162951535312, 1.000000000000000000, 0.9510565162951535312, 1.000000000000000000, 0.9510565162951535312, 1.000000000000000000, 0.9755282581475765991, 0.9755282581475767101 ) ) 
 REPRESENTATION_ITEM ( '' )  );
#21425 = CARTESIAN_POINT ( 'NONE',  ( 10.04305231718579705, 72.59999999999998010, 30.90933677959248982 ) ) ;
#21426 = CARTESIAN_POINT ( 'NONE',  ( 20.75514604977248467, 8.425000002731186655, -28.56700777964554305 ) ) ;
#21427 = CARTESIAN_POINT ( 'NONE',  ( 7.236395654485755280, 6.224999997268803931, 22.27133577429736988 ) ) ;
#21428 = LINE ( 'NONE', #29962, #2251 ) ;
#21429 = CARTESIAN_POINT ( 'NONE',  ( -0.04044903255042732459, 28.17930583240935860, -27.95245687107223986 ) ) ;
#21430 = CARTESIAN_POINT ( 'NONE',  ( 10.37757302488624056, 20.52500000273119340, -31.93888565452638417 ) ) ;
#21431 = CARTESIAN_POINT ( 'NONE',  ( 26.07999730980490227, 58.11979166666665719, 6.988114217767821046 ) ) ;
#21432 = VERTEX_POINT ( 'NONE', #15629 ) ;
#21433 = CARTESIAN_POINT ( 'NONE',  ( 33.58253175000000113, 64.22500000273117848, -10.91162601494193751 ) ) ;
#21434 = ORIENTED_EDGE ( 'NONE', *, *, #32828, .F. ) ;
#21435 = CARTESIAN_POINT ( 'NONE',  ( -26.00068869287340334, 18.15885416666666075, 15.01150461594643382 ) ) ;
#21436 = CARTESIAN_POINT ( 'NONE',  ( 20.47846945139902530, 11.71913166759064318, 20.53372385742071771 ) ) ;
#21437 = CARTESIAN_POINT ( 'NONE',  ( 33.58253175000000823, 4.025000002731196957, 10.91162601494192863 ) ) ;
#21438 = ORIENTED_EDGE ( 'NONE', *, *, #25716, .T. ) ;
#21439 = DIRECTION ( 'NONE',  ( 0.000000000000000000, 0.000000000000000000, -1.000000000000000000 ) ) ;
#21440 = CARTESIAN_POINT ( 'NONE',  ( -33.58253175000000113, 25.47500000273118914, 10.91162601494193929 ) ) ;
#21441 = CARTESIAN_POINT ( 'NONE',  ( -32.50000000000000000, 32.50000000546238255, 0.000000000000000000 ) ) ;
#21442 = EDGE_CURVE ( 'NONE', #17842, #2121, #22592, .T. ) ;
#21443 = CARTESIAN_POINT ( 'NONE',  ( -10.04305231718578462, 78.39999999999999147, 30.90933677959249337 ) ) ;
#21444 = DIRECTION ( 'NONE',  ( -1.000000000000000000, -1.224646799147353454E-16, 0.000000000000000000 ) ) ;
#21445 = CARTESIAN_POINT ( 'NONE',  ( 5.779280353836490358E-15, 37.00000000546237544, 32.49999999999999289 ) ) ;
#21446 = CARTESIAN_POINT ( 'NONE',  ( 20.75514604977249178, 42.07500000273117990, 28.56700777964553950 ) ) ;
#21447 = CARTESIAN_POINT ( 'NONE',  ( -26.29305231718579350, 23.80000000000000071, -19.10302069950537884 ) ) ;
#21448 = CARTESIAN_POINT ( 'NONE',  ( -32.50000000000000000, 21.99999999999999289, 0.000000000000000000 ) ) ;
#21449 = CARTESIAN_POINT ( 'NONE',  ( 19.82091636218621389, 4.200000000000009059, -14.40073868116559197 ) ) ;
#21450 = CARTESIAN_POINT ( 'NONE',  ( -33.58253175000000113, 61.02500000273118985, -10.91162601494193218 ) ) ;
#21451 = CARTESIAN_POINT ( 'NONE',  ( -5.147494310547430452, 78.44874571845313938, 32.50000000000000000 ) ) ;
#21452 = CARTESIAN_POINT ( 'NONE',  ( -8.446640517145639571E-15, 77.00000000546236834, 32.49999999999999289 ) ) ;
#21453 = CARTESIAN_POINT ( 'NONE',  ( 33.58253175000000113, 56.47500000273116427, -10.91162601494193574 ) ) ;
#21454 = CARTESIAN_POINT ( 'NONE',  ( -18.94512977948576093, 5.824999997268820451, 13.76444248337722698 ) ) ;
#21455 = CARTESIAN_POINT ( 'NONE',  ( 32.50000000000000711, 39.40000000546236691, 10.55989012756945122 ) ) ;
#21456 = CARTESIAN_POINT ( 'NONE',  ( -33.58253175000000113, 5.125000002731194826, 0.000000000000000000 ) ) ;
#21457 = CARTESIAN_POINT ( 'NONE',  ( 26.06988505166735592, 35.49517333425730214, 7.025853678916393896 ) ) ;
#21458 = CYLINDRICAL_SURFACE ( 'NONE', #22842, 32.50000000000000000 ) ;
#21459 = CARTESIAN_POINT ( 'NONE',  ( -7.689115195225046939, 52.00000000000003553, 32.34176759466017614 ) ) ;
#21460 = CARTESIAN_POINT ( 'NONE',  ( 10.37757302488624056, 28.52500000273118630, -31.93888565452638417 ) ) ;
#21461 = VECTOR ( 'NONE', #21742, 1000.000000000000000 ) ;
#21463 = AXIS2_PLACEMENT_3D ( 'NONE', #21230, #27201, #3692 ) ;
#21462 = CARTESIAN_POINT ( 'NONE',  ( 26.29305231718578995, 65.20000000000001705, -19.10302069950538240 ) ) ;
#21464 = CARTESIAN_POINT ( 'NONE',  ( -5.147494310547430452, 58.05125428700922185, -32.49999999999999289 ) ) ;
#21465 = CARTESIAN_POINT ( 'NONE',  ( 8.601468415847516980, 76.17500000273116711, -11.83890561707634603 ) ) ;
#21466 = CARTESIAN_POINT ( 'NONE',  ( -26.02091320914878025, 55.10638916574269786, -14.97647472619899389 ) ) ;
#21467 = CARTESIAN_POINT ( 'NONE',  ( -32.50000000000000000, 54.60000000546237686, 10.55989012756946366 ) ) ;
#21468 = CARTESIAN_POINT ( 'NONE',  ( 32.50000000000000711, 48.89999999999999858, 10.55989012756945122 ) ) ;
#21469 = CARTESIAN_POINT ( 'NONE',  ( 26.07999730980490227, 13.43229166666666607, 6.988114217767821046 ) ) ;
#21470 = CARTESIAN_POINT ( 'NONE',  ( -10.04305231718579172, 70.10000000546237686, -30.90933677959248982 ) ) ;
#21471 = CARTESIAN_POINT ( 'NONE',  ( -26.00068869287368756, 32.48177083333332860, -15.01150461594595775 ) ) ;
#21472 = CARTESIAN_POINT ( 'NONE',  ( 0.000000000000000000, 80.00000000000001421, 0.000000000000000000 ) ) ;
#21473 = ORIENTED_EDGE ( 'NONE', *, *, #18195, .T. ) ;
#21474 = CARTESIAN_POINT ( 'NONE',  ( 15.04653450569292872, 38.21652750092398065, -25.98046417659857710 ) ) ;
#21475 = CARTESIAN_POINT ( 'NONE',  ( 26.29305231718578995, 17.70000000546238894, -19.10302069950538240 ) ) ;
#21476 = CARTESIAN_POINT ( 'NONE',  ( 20.50609665440969565, 54.10937499999999289, -20.50609665441004736 ) ) ;
#21477 = CARTESIAN_POINT ( 'NONE',  ( -28.01184896238304134, 66.71354166666665719, -7.505752307972844761 ) ) ;
#21478 = CARTESIAN_POINT ( 'NONE',  ( 33.58253175000000113, 46.47500000273118559, -10.91162601494193751 ) ) ;
#21479 = CARTESIAN_POINT ( 'NONE',  ( -2.092463501923844636E-15, 56.00000000546236123, -34.17252228774368916 ) ) ;
#21480 = CARTESIAN_POINT ( 'NONE',  ( 13.91746825000000065, 78.27500000273118985, 4.522059556121114987 ) ) ;
#21481 = CARTESIAN_POINT ( 'NONE',  ( 20.75514604977249178, 35.82500000273117990, 28.56700777964553950 ) ) ;
#21482 = DIRECTION ( 'NONE',  ( 0.000000000000000000, 0.000000000000000000, -1.000000000000000000 ) ) ;
#21483 = CARTESIAN_POINT ( 'NONE',  ( -33.58253175000000113, 63.37500000273119127, 0.000000000000000000 ) ) ;
#21484 = CARTESIAN_POINT ( 'NONE',  ( 20.08610463437158344, 1.200000005462378283, 27.64615127144129403 ) ) ;
#21485 = CARTESIAN_POINT ( 'NONE',  ( -10.37757302488624411, 54.72500000273118559, -31.93888565452638417 ) ) ;
#21486 = CARTESIAN_POINT ( 'NONE',  ( 15.01150461594643382, 17.29947916666666430, 26.00068869287340334 ) ) ;
#21487 = CARTESIAN_POINT ( 'NONE',  ( 10.04305231718578817, 43.39999999999999147, -30.90933677959249337 ) ) ;
#21488 = CARTESIAN_POINT ( 'NONE',  ( 7.236395654485755280, 8.224999997268806595, 22.27133577429736988 ) ) ;
#21489 = CARTESIAN_POINT ( 'NONE',  ( -20.75514604977248112, 7.675000002731199089, 28.56700777964554661 ) ) ;
#21490 = CARTESIAN_POINT ( 'NONE',  ( 0.000000000000000000, 52.00000000000000711, 0.000000000000000000 ) ) ;
#21491 = DIRECTION ( 'NONE',  ( 0.8660254037844402619, -0.4999999999999970579, 0.000000000000000000 ) ) ;
#21492 = CARTESIAN_POINT ( 'NONE',  ( 10.37757302488624056, 70.77500000273117564, -31.93888565452638417 ) ) ;
#21493 = CARTESIAN_POINT ( 'NONE',  ( 5.348221797398307942, 74.00000000000001421, 12.84883053416113974 ) ) ;
#21494 = CARTESIAN_POINT ( 'NONE',  ( 27.16883889988624290, 66.17500000273116711, 19.73931689729373673 ) ) ;
#21495 = ORIENTED_EDGE ( 'NONE', *, *, #10557, .F. ) ;
#21496 = CARTESIAN_POINT ( 'NONE',  ( 0.000000000000000000, 111.9999999999999858, 0.000000000000000000 ) ) ;
#21497 = CARTESIAN_POINT ( 'NONE',  ( 2.584737979205441561E-13, 58.83593750000000000, 27.95245687107222921 ) ) ;
#21498 = CARTESIAN_POINT ( 'NONE',  ( -10.37757302488624411, 50.72500000273118559, -31.93888565452638417 ) ) ;
#21499 = CARTESIAN_POINT ( 'NONE',  ( 10.37757302488624056, 12.77500000273117031, -31.93888565452638417 ) ) ;
#21500 = CARTESIAN_POINT ( 'NONE',  ( 27.16883889988623935, 64.57500000273118701, -19.73931689729374384 ) ) ;
#21501 = CARTESIAN_POINT ( 'NONE',  ( -13.97622843553632777, 43.08072916666666430, -24.20753774853731599 ) ) ;
#21502 = CARTESIAN_POINT ( 'NONE',  ( -20.53372385742071771, 33.20350666759063074, 20.47846945139902530 ) ) ;
#21503 = CARTESIAN_POINT ( 'NONE',  ( 20.53372385742108008, 22.59336833240935505, 20.47846945139866648 ) ) ;
#21504 = CARTESIAN_POINT ( 'NONE',  ( -10.04305231718579172, 74.10000000546239107, -30.90933677959248982 ) ) ;
#21505 = CARTESIAN_POINT ( 'NONE',  ( 4.300734207923757602, 76.27500000273118985, -13.23629886949340673 ) ) ;
#21506 = CARTESIAN_POINT ( 'NONE',  ( 20.75514604977249178, 35.82500000273117990, 28.56700777964553950 ) ) ;
#21507 = CARTESIAN_POINT ( 'NONE',  ( 24.18731323226221974, 49.37722249907602645, -14.01125832528328985 ) ) ;
#21508 = CARTESIAN_POINT ( 'NONE',  ( -23.41746825000000243, 15.52499999726882507, -7.608796670333730638 ) ) ;
#21509 = CARTESIAN_POINT ( 'NONE',  ( 7.570916362186213000, 14.39999999999999680, -23.30088464923126423 ) ) ;
#21510 = EDGE_LOOP ( 'NONE', ( #27813, #23503, #11170, #9483 ) ) ;
#21511 = CARTESIAN_POINT ( 'NONE',  ( 33.58253175000000113, 50.37500000273119127, -4.112674001490185761E-15 ) ) ;
#21512 =( BOUNDED_CURVE ( )  B_SPLINE_CURVE ( 2, ( #7028, #17511, #25572, #20259, #28310, #1875, #33281, #7374, #12353, #22822, #9777, #4798, #15277 ),
 .UNSPECIFIED., .F., .T. ) 
 B_SPLINE_CURVE_WITH_KNOTS ( ( 3, 2, 2, 2, 2, 2, 3 ),
 ( 0.6388888888888889506, 0.6444444444444444864, 0.6555555555555555580, 0.6666666666666666297, 0.6777777777777778123, 0.6888888888888888840, 0.6944444444444444198 ),
 .UNSPECIFIED. ) 
 CURVE ( )  GEOMETRIC_REPRESENTATION_ITEM ( )  RATIONAL_B_SPLINE_CURVE ( ( 0.9755282581475768211, 0.9755282581475770431, 1.000000000000000000, 0.9510565162951535312, 1.000000000000000000, 0.9510565162951535312, 1.000000000000000000, 0.9510565162951535312, 1.000000000000000000, 0.9510565162951535312, 1.000000000000000000, 0.9755282581475768211, 0.9755282581475768211 ) ) 
 REPRESENTATION_ITEM ( '' )  );
#21513 = CARTESIAN_POINT ( 'NONE',  ( 26.29305231718578995, 51.19999999999999574, -19.10302069950538240 ) ) ;
#21514 = CARTESIAN_POINT ( 'NONE',  ( -24.18731323226248264, 47.66965250092398065, -14.01125832528284931 ) ) ;
#21515 = CARTESIAN_POINT ( 'NONE',  ( -27.16883889988624290, 69.17500000273119554, -19.73931689729374028 ) ) ;
#21516 = ORIENTED_EDGE ( 'NONE', *, *, #18122, .F. ) ;
#21517 = CARTESIAN_POINT ( 'NONE',  ( -20.75514604977248823, 18.82500000273119767, -28.56700777964554305 ) ) ;
#21518 = CARTESIAN_POINT ( 'NONE',  ( -2.584737979205441561E-13, 26.17968750000000000, -30.02300923189239512 ) ) ;
#21519 = ORIENTED_EDGE ( 'NONE', *, *, #11270, .T. ) ;
#21520 = VECTOR ( 'NONE', #28623, 1000.000000000000000 ) ;
#21521 = CARTESIAN_POINT ( 'NONE',  ( -32.50000000000000000, 48.50000000546239676, 0.000000000000000000 ) ) ;
#21522 = CARTESIAN_POINT ( 'NONE',  ( 20.75514604977248467, 52.42500000273118133, -28.56700777964554305 ) ) ;
#21523 = CARTESIAN_POINT ( 'NONE',  ( 7.505752307972854531, 50.38541666666666430, -28.01184896238303423 ) ) ;
#21524 = CARTESIAN_POINT ( 'NONE',  ( 26.29305231718579350, 17.30000000546239036, 19.10302069950537529 ) ) ;
#21525 = DIRECTION ( 'NONE',  ( 0.000000000000000000, -1.000000000000000000, 0.000000000000000000 ) ) ;
#21526 = CARTESIAN_POINT ( 'NONE',  ( -14.47279130897151767, 7.824999997268806240, -19.92008829642072598 ) ) ;
#21527 = CARTESIAN_POINT ( 'NONE',  ( -2.162160676586881955E-15, 26.87500000273116996, -35.31076352940723240 ) ) ;
#21528 = LINE ( 'NONE', #15879, #16003 ) ;
#21529 = CARTESIAN_POINT ( 'NONE',  ( 14.97647472619900455, 66.27826416574268364, -26.02091320914876960 ) ) ;
#21530 = CARTESIAN_POINT ( 'NONE',  ( 11.25946833292375793, 80.07500000273121543, -8.180482586598735395 ) ) ;
#21531 = EDGE_CURVE ( 'NONE', #1522, #3647, #15395, .T. ) ;
#21532 = CARTESIAN_POINT ( 'NONE',  ( 32.50000000000000711, 8.900000000000011013, 10.55989012756945122 ) ) ;
#21533 = ORIENTED_EDGE ( 'NONE', *, *, #3570, .T. ) ;
#21534 = CARTESIAN_POINT ( 'NONE',  ( 15.14183272437241889, 19.44999999453763806, 20.84094480462498211 ) ) ;
#21535 = CARTESIAN_POINT ( 'NONE',  ( 4.300734207923761154, 75.47500000273119269, 13.23629886949340495 ) ) ;
#21536 = CARTESIAN_POINT ( 'NONE',  ( 24.20753774853756113, 34.20052083333332860, 13.97622843553589789 ) ) ;
#21537 = CARTESIAN_POINT ( 'NONE',  ( -20.75514604977248823, 24.82500000273117635, -28.56700777964554305 ) ) ;
#21538 = CARTESIAN_POINT ( 'NONE',  ( 33.58253175000000823, 74.02500000273120406, 10.91162601494192863 ) ) ;
#21539 = CARTESIAN_POINT ( 'NONE',  ( -20.75514604977248823, 31.07500000273118701, -28.56700777964554305 ) ) ;
#21540 = CARTESIAN_POINT ( 'NONE',  ( -20.75514604977248823, 15.07500000273116747, -28.56700777964554305 ) ) ;
#21541 = CARTESIAN_POINT ( 'NONE',  ( -14.01125832528285109, 53.68527750092398065, 24.18731323226248264 ) ) ;
#21542 = EDGE_CURVE ( 'NONE', #25961, #30646, #32056, .T. ) ;
#21543 = CARTESIAN_POINT ( 'NONE',  ( -20.75514604977248112, 71.42500000273119554, 28.56700777964554661 ) ) ;
#21544 = EDGE_CURVE ( 'NONE', #16826, #774, #445, .T. ) ;
#21545 = DIRECTION ( 'NONE',  ( -0.000000000000000000, 1.000000000000000000, -0.000000000000000000 ) ) ;
#21546 = CARTESIAN_POINT ( 'NONE',  ( -13.91746824999999887, 81.37500000273118417, 0.000000000000000000 ) ) ;
#21547 = VECTOR ( 'NONE', #33470, 1000.000000000000000 ) ;
#21548 = CARTESIAN_POINT ( 'NONE',  ( 6.277390505771533514E-15, 54.49999999999999289, 34.17252228774368916 ) ) ;
#21549 = CARTESIAN_POINT ( 'NONE',  ( -4.635254915624211769, 71.85000000546237686, -14.26584774442730286 ) ) ;
#21550 = CARTESIAN_POINT ( 'NONE',  ( -33.58253175000000113, 55.12500000273118417, 0.000000000000000000 ) ) ;
#21551 = CARTESIAN_POINT ( 'NONE',  ( -23.41746825000000598, 18.22499999726882436, 7.608796670333726198 ) ) ;
#21552 = EDGE_CURVE ( 'NONE', #11228, #4064, #31293, .T. ) ;
#21553 =( BOUNDED_SURFACE ( )  B_SPLINE_SURFACE ( 1, 2, ( 
 ( #4758, #30660, #30838, #25181, #2010, #12652, #33768, #18160, #28602, #6989, #15065, #5101, #17640, #15235, #27932, #7330, #4416, #28101, #2179, #23122, #7843, #26380, #26210, #15924, #24146, #13000, #2704, #3044, #13164, #2871, #13516, #18670, #23979, #18332, #13340, #31350, #32020, #5613, #450, #18501, #31522, #28945, #21574, #616, #10424, #10932, #29446, #29109, #10596, #23813, #15587, #278, #21407, #11105, #8516, #18834, #33933, #19002, #105, #5274, #10766, #31686, #8180, #21073, #23641, #16097, #21243, #31853, #29280, #5781, #26548, #8345, #26038, #16261, #26718, #3214, #13682, #2532, #23471, #8016, #20902, #28777, #15756, #5443, #16755, #24472, #32515, #6108, #16921, #1107, #22238, #3376, #6449, #16588, #32190, #1451, #19662, #947, #17089, #1277, #30105 ),
 ( #22400, #6611, #11427, #786, #24969, #19168, #27381, #29771, #3705, #21902, #11930, #27548, #9340, #19329, #8684, #26880, #3870, #29606, #9015, #14343, #32848, #24800, #27044, #11757, #32683, #9178, #19497, #6279, #24634, #3538, #14177, #32354, #22071, #14510, #4035, #19825, #5949, #8848, #29945, #16428, #11592, #13846, #24312, #11268, #14010, #21744, #27214, #27891, #30449, #22915, #6947, #30277, #7287, #15370, #17951, #28230, #12094, #9695, #17771, #25825, #14679, #10046, #27719, #1970, #2315, #22741, #4716, #30619, #9520, #33544, #23261, #4546, #6777, #20175, #15196, #4375, #20344, #23083, #15021, #12788, #33724, #25660, #7115, #22564, #17597, #17430, #28059, #4889, #4207, #14849, #2139, #25315, #25491, #12614, #33371, #20525, #33015, #12445, #20002, #10222, #30794 ) ),
 .UNSPECIFIED., .F., .F., .F. ) 
 B_SPLINE_SURFACE_WITH_KNOTS ( ( 2, 2 ),
 ( 3, 2, 2, 2, 2, 2, 2, 2, 2, 2, 2, 2, 2, 2, 2, 2, 2, 2, 2, 2, 2, 2, 2, 2, 2, 2, 2, 2, 2, 2, 2, 2, 2, 2, 2, 2, 2, 2, 2, 2, 2, 2, 2, 2, 2, 2, 2, 2, 2, 2, 3 ),
 ( 0.000000000000000000, 1.000000000000000000 ),
 ( 0.000000000000000000, 0.02000000000000000042, 0.04000000000000000083, 0.05999999999999999778, 0.08000000000000000167, 0.1000000000000000056, 0.1199999999999999956, 0.1400000000000000133, 0.1600000000000000033, 0.1799999999999999933, 0.2000000000000000111, 0.2200000000000000011, 0.2399999999999999911, 0.2600000000000000089, 0.2800000000000000266, 0.2999999999999999889, 0.3200000000000000067, 0.3400000000000000244, 0.3599999999999999867, 0.3800000000000000044, 0.4000000000000000222, 0.4199999999999999845, 0.4400000000000000022, 0.4600000000000000200, 0.4799999999999999822, 0.5000000000000000000, 0.5200000000000000178, 0.5400000000000000355, 0.5600000000000000533, 0.5799999999999999600, 0.5999999999999999778, 0.6199999999999999956, 0.6400000000000000133, 0.6600000000000000311, 0.6800000000000000488, 0.6999999999999999556, 0.7199999999999999734, 0.7399999999999999911, 0.7600000000000000089, 0.7800000000000000266, 0.8000000000000000444, 0.8199999999999999512, 0.8399999999999999689, 0.8599999999999999867, 0.8800000000000000044, 0.9000000000000000222, 0.9200000000000000400, 0.9399999999999999467, 0.9599999999999999645, 0.9799999999999999822, 1.000000000000000000 ),
 .UNSPECIFIED. ) 
 GEOMETRIC_REPRESENTATION_ITEM ( )  RATIONAL_B_SPLINE_SURFACE ( (
 ( 1.000000000000000000, 0.9510565162951535312, 1.000000000000000000, 0.9510565162951535312, 1.000000000000000000, 0.9510565162951535312, 1.000000000000000000, 0.9510565162951535312, 1.000000000000000000, 0.9510565162951535312, 1.000000000000000000, 0.9510565162951535312, 1.000000000000000000, 0.9510565162951535312, 1.000000000000000000, 0.9510565162951535312, 1.000000000000000000, 0.9510565162951535312, 1.000000000000000000, 0.9510565162951535312, 1.000000000000000000, 0.9510565162951535312, 1.000000000000000000, 0.9510565162951535312, 1.000000000000000000, 0.9510565162951535312, 1.000000000000000000, 0.9510565162951535312, 1.000000000000000000, 0.9510565162951535312, 1.000000000000000000, 0.9510565162951535312, 1.000000000000000000, 0.9510565162951535312, 1.000000000000000000, 0.9510565162951535312, 1.000000000000000000, 0.9510565162951535312, 1.000000000000000000, 0.9510565162951535312, 1.000000000000000000, 0.9510565162951535312, 1.000000000000000000, 0.9510565162951535312, 1.000000000000000000, 0.9510565162951535312, 1.000000000000000000, 0.9510565162951535312, 1.000000000000000000, 0.9510565162951535312, 1.000000000000000000, 0.9510565162951535312, 1.000000000000000000, 0.9510565162951535312, 1.000000000000000000, 0.9510565162951535312, 1.000000000000000000, 0.9510565162951535312, 1.000000000000000000, 0.9510565162951535312, 1.000000000000000000, 0.9510565162951535312, 1.000000000000000000, 0.9510565162951535312, 1.000000000000000000, 0.9510565162951535312, 1.000000000000000000, 0.9510565162951535312, 1.000000000000000000, 0.9510565162951535312, 1.000000000000000000, 0.9510565162951535312, 1.000000000000000000, 0.9510565162951535312, 1.000000000000000000, 0.9510565162951535312, 1.000000000000000000, 0.9510565162951535312, 1.000000000000000000, 0.9510565162951535312, 1.000000000000000000, 0.9510565162951535312, 1.000000000000000000, 0.9510565162951535312, 1.000000000000000000, 0.9510565162951535312, 1.000000000000000000, 0.9510565162951535312, 1.000000000000000000, 0.9510565162951535312, 1.000000000000000000, 0.9510565162951535312, 1.000000000000000000, 0.9510565162951535312, 1.000000000000000000, 0.9510565162951535312, 1.000000000000000000, 0.9510565162951535312, 1.000000000000000000, 0.9510565162951535312, 1.000000000000000000),
 ( 1.000000000000000000, 0.9510565162951535312, 1.000000000000000000, 0.9510565162951535312, 1.000000000000000000, 0.9510565162951535312, 1.000000000000000000, 0.9510565162951535312, 1.000000000000000000, 0.9510565162951535312, 1.000000000000000000, 0.9510565162951535312, 1.000000000000000000, 0.9510565162951535312, 1.000000000000000000, 0.9510565162951535312, 1.000000000000000000, 0.9510565162951535312, 1.000000000000000000, 0.9510565162951535312, 1.000000000000000000, 0.9510565162951535312, 1.000000000000000000, 0.9510565162951535312, 1.000000000000000000, 0.9510565162951535312, 1.000000000000000000, 0.9510565162951535312, 1.000000000000000000, 0.9510565162951535312, 1.000000000000000000, 0.9510565162951535312, 1.000000000000000000, 0.9510565162951535312, 1.000000000000000000, 0.9510565162951535312, 1.000000000000000000, 0.9510565162951535312, 1.000000000000000000, 0.9510565162951535312, 1.000000000000000000, 0.9510565162951535312, 1.000000000000000000, 0.9510565162951535312, 1.000000000000000000, 0.9510565162951535312, 1.000000000000000000, 0.9510565162951535312, 1.000000000000000000, 0.9510565162951535312, 1.000000000000000000, 0.9510565162951535312, 1.000000000000000000, 0.9510565162951535312, 1.000000000000000000, 0.9510565162951535312, 1.000000000000000000, 0.9510565162951535312, 1.000000000000000000, 0.9510565162951535312, 1.000000000000000000, 0.9510565162951535312, 1.000000000000000000, 0.9510565162951535312, 1.000000000000000000, 0.9510565162951535312, 1.000000000000000000, 0.9510565162951535312, 1.000000000000000000, 0.9510565162951535312, 1.000000000000000000, 0.9510565162951535312, 1.000000000000000000, 0.9510565162951535312, 1.000000000000000000, 0.9510565162951535312, 1.000000000000000000, 0.9510565162951535312, 1.000000000000000000, 0.9510565162951535312, 1.000000000000000000, 0.9510565162951535312, 1.000000000000000000, 0.9510565162951535312, 1.000000000000000000, 0.9510565162951535312, 1.000000000000000000, 0.9510565162951535312, 1.000000000000000000, 0.9510565162951535312, 1.000000000000000000, 0.9510565162951535312, 1.000000000000000000, 0.9510565162951535312, 1.000000000000000000, 0.9510565162951535312, 1.000000000000000000, 0.9510565162951535312, 1.000000000000000000, 0.9510565162951535312, 1.000000000000000000) ) ) 
 REPRESENTATION_ITEM ( '' )  SURFACE ( )  );
#21554 = EDGE_LOOP ( 'NONE', ( #5645, #6007, #19318, #32135 ) ) ;
#21555 = ORIENTED_EDGE ( 'NONE', *, *, #13790, .F. ) ;
#21556 = CARTESIAN_POINT ( 'NONE',  ( -2.162160676586881955E-15, 64.87500000273119838, -35.31076352940723240 ) ) ;
#21557 = CARTESIAN_POINT ( 'NONE',  ( 14.47279130897151589, 4.324999997268801799, 19.92008829642072953 ) ) ;
#21558 = CARTESIAN_POINT ( 'NONE',  ( -24.18731323226248264, 23.60715250092398421, -14.01125832528284931 ) ) ;
#21559 = ORIENTED_EDGE ( 'NONE', *, *, #23100, .T. ) ;
#21560 = CARTESIAN_POINT ( 'NONE',  ( -27.16883889988623935, 39.32500000273118701, 19.73931689729374739 ) ) ;
#21561 = CARTESIAN_POINT ( 'NONE',  ( -7.570916362186210335, 0.5999999999999894307, -23.30088464923126779 ) ) ;
#21562 = ORIENTED_EDGE ( 'NONE', *, *, #18568, .T. ) ;
#21563 = CARTESIAN_POINT ( 'NONE',  ( 20.50609665441005092, 54.96875000000000000, 20.50609665440969209 ) ) ;
#21564 = CARTESIAN_POINT ( 'NONE',  ( -20.08610463437157989, 60.20000000546237828, -27.64615127144129758 ) ) ;
#21565 = CARTESIAN_POINT ( 'NONE',  ( 0.000000000000000000, 16.99999999999998579, 0.000000000000000000 ) ) ;
#21566 = CARTESIAN_POINT ( 'NONE',  ( -33.58253175000000113, 73.12500000273119838, 0.000000000000000000 ) ) ;
#21567 = CARTESIAN_POINT ( 'NONE',  ( -20.50609665440969209, 24.89062500000000000, 20.50609665441005092 ) ) ;
#21568 = CARTESIAN_POINT ( 'NONE',  ( 1.577395562988744260E-15, 8.499999999999992895, -25.76082449383753925 ) ) ;
#21569 = CARTESIAN_POINT ( 'NONE',  ( -33.58253175000000113, 11.47500000273119625, 10.91162601494193929 ) ) ;
#21570 = CARTESIAN_POINT ( 'NONE',  ( 10.37757302488624767, 17.72500000273119625, 31.93888565452638417 ) ) ;
#21571 = CARTESIAN_POINT ( 'NONE',  ( -13.91746824999999887, 76.87500000273116996, 0.000000000000000000 ) ) ;
#21572 = CARTESIAN_POINT ( 'NONE',  ( -15.00000000000000000, 72.00000000000001421, 0.000000000000000000 ) ) ;
#21573 = CARTESIAN_POINT ( 'NONE',  ( 20.47846945139867003, 38.92149333240934794, -20.53372385742107653 ) ) ;
#21574 = CARTESIAN_POINT ( 'NONE',  ( -11.25946833292375793, 77.17500000273119554, -8.180482586598733619 ) ) ;
#21575 = CARTESIAN_POINT ( 'NONE',  ( -15.01150461594642316, 49.95572916666665009, -26.00068869287341045 ) ) ;
#21576 = VECTOR ( 'NONE', #22801, 999.9999999999998863 ) ;
#21577 = CARTESIAN_POINT ( 'NONE',  ( -7.570916362186215665, 11.39999999999999325, 23.30088464923126423 ) ) ;
#21578 = CARTESIAN_POINT ( 'NONE',  ( -20.08610463437157989, 54.20000000546236407, -27.64615127144129758 ) ) ;
#21579 = CARTESIAN_POINT ( 'NONE',  ( -19.06425588902558133, 64.70274333240935505, 19.11951029504797006 ) ) ;
#21580 = CARTESIAN_POINT ( 'NONE',  ( 10.37757302488624767, 45.72500000273119269, 31.93888565452638417 ) ) ;
#21581 = CARTESIAN_POINT ( 'NONE',  ( -15.00000000000000000, 72.35000000546239107, 4.873795443493597723 ) ) ;
#21582 = CARTESIAN_POINT ( 'NONE',  ( -27.16883889988624290, 49.17500000273118843, -19.73931689729374028 ) ) ;
#21583 = CARTESIAN_POINT ( 'NONE',  ( 10.37757302488624767, 33.97500000273117848, 31.93888565452638417 ) ) ;
#21584 = CARTESIAN_POINT ( 'NONE',  ( 21.27620594755971695, 16.99999999999997868, 9.851211979822984688 ) ) ;
#21585 = CARTESIAN_POINT ( 'NONE',  ( 6.988114217768294445, 24.31770833333332504, 26.07999730980477437 ) ) ;
#21586 = CARTESIAN_POINT ( 'NONE',  ( 7.570916362186213000, 12.14999999453761426, -23.30088464923126423 ) ) ;
#21587 = CARTESIAN_POINT ( 'NONE',  ( -32.50000000000000000, 44.50000000546238965, 0.000000000000000000 ) ) ;
#21588 = CARTESIAN_POINT ( 'NONE',  ( -2.092463501923844636E-15, 71.50000000000001421, -34.17252228774368916 ) ) ;
#21589 = CARTESIAN_POINT ( 'NONE',  ( -10.37757302488623701, 11.52500000273119696, 31.93888565452638417 ) ) ;
#21590 = CARTESIAN_POINT ( 'NONE',  ( -18.94512977948576093, 3.824999997268818674, 13.76444248337722698 ) ) ;
#21591 = FACE_OUTER_BOUND ( 'NONE', #26151, .T. ) ;
#21592 = CARTESIAN_POINT ( 'NONE',  ( -14.01125832528328985, 31.33034749907602290, -24.18731323226223040 ) ) ;
#21593 = EDGE_CURVE ( 'NONE', #24499, #11893, #29479, .T. ) ;
#21594 = CARTESIAN_POINT ( 'NONE',  ( -4.635254915624208216, 76.65000000546237402, 14.26584774442730463 ) ) ;
#21595 = CARTESIAN_POINT ( 'NONE',  ( 33.58253175000000113, 20.12500000273118062, -4.112674001490185761E-15 ) ) ;
#21596 = VECTOR ( 'NONE', #20055, 1000.000000000000000 ) ;
#21597 = CARTESIAN_POINT ( 'NONE',  ( -6.988114217768288228, 53.53645833333332860, -26.07999730980477437 ) ) ;
#21598 = AXIS2_PLACEMENT_3D ( 'NONE', #27855, #30583, #1749 ) ;
#21599 = ORIENTED_EDGE ( 'NONE', *, *, #14693, .F. ) ;
#21600 = CARTESIAN_POINT ( 'NONE',  ( -10.37757302488623701, 57.52500000273118275, 31.93888565452638417 ) ) ;
#21601 = ORIENTED_EDGE ( 'NONE', *, *, #27904, .T. ) ;
#21602 = CARTESIAN_POINT ( 'NONE',  ( 28.01184896238290278, 20.02083333333332860, -7.505752307973347470 ) ) ;
#21603 = CARTESIAN_POINT ( 'NONE',  ( 0.04044903254992426173, 24.18006916759064140, -30.02300923189239867 ) ) ;
#21604 = CARTESIAN_POINT ( 'NONE',  ( 7.570916362186207671, 15.34999999453762243, 23.30088464923126779 ) ) ;
#21605 = ORIENTED_EDGE ( 'NONE', *, *, #15946, .T. ) ;
#21606 = CARTESIAN_POINT ( 'NONE',  ( 23.41746825000000243, 0.7249999972688272454, -7.608796670333727974 ) ) ;
#21607 = CARTESIAN_POINT ( 'NONE',  ( 27.16883889988624290, 28.17500000273118133, 19.73931689729373673 ) ) ;
#21608 = CARTESIAN_POINT ( 'NONE',  ( -10.04305231718578462, 32.90000000546239534, 30.90933677959249337 ) ) ;
#21609 = CARTESIAN_POINT ( 'NONE',  ( 20.08610463437157279, 77.30000000000001137, -27.64615127144129758 ) ) ;
#21610 = DIRECTION ( 'NONE',  ( 0.000000000000000000, 0.000000000000000000, 1.000000000000000000 ) ) ;
#21611 = CARTESIAN_POINT ( 'NONE',  ( -24.50000000000000000, 11.00000000000001066, -3.000384657911015469E-15 ) ) ;
#21612 = CARTESIAN_POINT ( 'NONE',  ( -20.75514604977248823, 45.07500000273117990, -28.56700777964554305 ) ) ;
#21613 =( BOUNDED_CURVE ( )  B_SPLINE_CURVE ( 2, ( #31141, #7113, #28562, #17595, #15542, #12786, #15019, #10382, #25658, #33722, #1968, #28057, #12443 ),
 .UNSPECIFIED., .F., .T. ) 
 B_SPLINE_CURVE_WITH_KNOTS ( ( 3, 2, 2, 2, 2, 2, 3 ),
 ( 0.2499999999999999722, 0.2555555555555555358, 0.2666666666666666630, 0.2777777777777777901, 0.2888888888888888618, 0.2999999999999999889, 0.3055555555555555802 ),
 .UNSPECIFIED. ) 
 CURVE ( )  GEOMETRIC_REPRESENTATION_ITEM ( )  RATIONAL_B_SPLINE_CURVE ( ( 0.9755282581475768211, 0.9755282581475768211, 1.000000000000000000, 0.9510565162951535312, 1.000000000000000000, 0.9510565162951535312, 1.000000000000000000, 0.9510565162951535312, 1.000000000000000000, 0.9510565162951535312, 1.000000000000000000, 0.9755282581475765991, 0.9755282581475767101 ) ) 
 REPRESENTATION_ITEM ( '' )  );
#21614 = CARTESIAN_POINT ( 'NONE',  ( 10.04305231718579705, 22.59999999999999432, 30.90933677959248982 ) ) ;
#21615 = CARTESIAN_POINT ( 'NONE',  ( 10.04305231718579705, 20.60000000000000853, 30.90933677959248982 ) ) ;
#21616 = CARTESIAN_POINT ( 'NONE',  ( -7.570916362186215665, 13.39999999999999503, 23.30088464923126423 ) ) ;
#21617 =( BOUNDED_CURVE ( )  B_SPLINE_CURVE ( 2, ( #10565, #23783, #7814, #250, #33736, #15894, #2326, #2678, #12970, #18132, #79, #20713, #23444 ),
 .UNSPECIFIED., .F., .F. ) 
 B_SPLINE_CURVE_WITH_KNOTS ( ( 3, 2, 2, 2, 2, 2, 3 ),
 ( 0.1987179487179487336, 0.2000000000000000111, 0.2025641025641025661, 0.2051282051282051211, 0.2076923076923077038, 0.2102564102564102588, 0.2115384615384615363 ),
 .UNSPECIFIED. ) 
 CURVE ( )  GEOMETRIC_REPRESENTATION_ITEM ( )  RATIONAL_B_SPLINE_CURVE ( ( 0.9755282581475768211, 0.9755282581475770431, 1.000000000000000000, 0.9510565162951535312, 1.000000000000000000, 0.9510565162951535312, 1.000000000000000000, 0.9510565162951535312, 1.000000000000000000, 0.9510565162951535312, 1.000000000000000000, 0.9755282581475768211, 0.9755282581475768211 ) ) 
 REPRESENTATION_ITEM ( '' )  );
#21618 = CARTESIAN_POINT ( 'NONE',  ( -2.162160676586881955E-15, 60.62500000273117706, -35.31076352940723240 ) ) ;
#21619 = TOROIDAL_SURFACE ( 'NONE', #237, 12.11000150615021553, 1.999999999999992228 ) ;
#21620 = CARTESIAN_POINT ( 'NONE',  ( 33.58253175000000823, 54.27500000273118985, 10.91162601494192685 ) ) ;
#21621 = CARTESIAN_POINT ( 'NONE',  ( 1.507698388325705758E-15, 11.12499999726881761, -24.62258325217400312 ) ) ;
#21622 = CARTESIAN_POINT ( 'NONE',  ( 24.50000000000000000, 3.899999999999992806, 7.960532557706212486 ) ) ;
#21623 = CARTESIAN_POINT ( 'NONE',  ( -20.75514604977248112, 5.425000002731182214, 28.56700777964554661 ) ) ;
#21624 = CARTESIAN_POINT ( 'NONE',  ( 26.06988505166735592, 38.93267333425729504, 7.025853678916393896 ) ) ;
#21625 = PLANE ( 'NONE',  #10240 ) ;
#21626 = CARTESIAN_POINT ( 'NONE',  ( -6.668400408272875007E-16, 2.249999994537632553, -24.50000000000000355 ) ) ;
#21627 = CARTESIAN_POINT ( 'NONE',  ( 33.58253175000000113, 28.22500000273119269, -10.91162601494193751 ) ) ;
#21628 = CARTESIAN_POINT ( 'NONE',  ( 32.50000000000000711, 64.89999999999999147, 10.55989012756945122 ) ) ;
#21629 = CARTESIAN_POINT ( 'NONE',  ( 5.779280353836490358E-15, 59.00000000546238255, 32.49999999999999289 ) ) ;
#21630 = CARTESIAN_POINT ( 'NONE',  ( 26.29305231718578995, 1.700000005462387609, -19.10302069950538240 ) ) ;
#21631 = CARTESIAN_POINT ( 'NONE',  ( 14.97647472619900455, 55.96576416574269786, -26.02091320914876960 ) ) ;
#21632 = CARTESIAN_POINT ( 'NONE',  ( -20.08610463437157989, 50.20000000546237118, -27.64615127144129758 ) ) ;
#21633 = ADVANCED_FACE ( 'NONE', ( #24350 ), #3411, .T. ) ;
#21634 = CARTESIAN_POINT ( 'NONE',  ( 31.91025403784435710, -18.96891108675447413, 3.952264761658314980E-15 ) ) ;
#21635 = DIRECTION ( 'NONE',  ( -0.000000000000000000, -1.000000000000000000, -0.000000000000000000 ) ) ;
#21636 = CARTESIAN_POINT ( 'NONE',  ( 24.20753774853756113, 27.32552083333332860, 13.97622843553589789 ) ) ;
#21637 = ADVANCED_FACE ( 'NONE', ( #29639 ), #6142, .T. ) ;
#21638 = CARTESIAN_POINT ( 'NONE',  ( -27.16883889988623935, 73.32500000273118701, 19.73931689729374739 ) ) ;
#21639 = CARTESIAN_POINT ( 'NONE',  ( -15.01150461594642138, 29.33072916666665719, -26.00068869287340334 ) ) ;
#21640 = CARTESIAN_POINT ( 'NONE',  ( -23.41746824999999887, 14.12499999726882294, -2.867812753649727150E-15 ) ) ;
#21641 = ORIENTED_EDGE ( 'NONE', *, *, #24810, .F. ) ;
#21642 = CARTESIAN_POINT ( 'NONE',  ( 25.98046417659858420, 42.51340250092398065, 15.04653450569292872 ) ) ;
#21643 = CARTESIAN_POINT ( 'NONE',  ( -32.50000000000000000, 18.60000000546238041, 10.55989012756946366 ) ) ;
#21644 = CARTESIAN_POINT ( 'NONE',  ( -7.505752307973343918, 50.09895833333332860, -28.01184896238290989 ) ) ;
#21645 = CARTESIAN_POINT ( 'NONE',  ( 0.000000000000000000, 82.00000000000001421, -15.00000000000000000 ) ) ;
#21646 = CARTESIAN_POINT ( 'NONE',  ( 20.75514604977248467, 46.67500000273118133, -28.56700777964554305 ) ) ;
#21647 = CARTESIAN_POINT ( 'NONE',  ( -26.29305231718579350, 50.30000000546236549, -19.10302069950537884 ) ) ;
#21648 = CARTESIAN_POINT ( 'NONE',  ( -7.579748464070167083E-14, 16.50000000000000355, -24.50000000000000000 ) ) ;
#21649 = CARTESIAN_POINT ( 'NONE',  ( -27.16883889988623935, 35.32500000273120122, 19.73931689729374739 ) ) ;
#21650 = CARTESIAN_POINT ( 'NONE',  ( 3.980102097228898626E-15, 80.00000000000001421, 32.50000000000000000 ) ) ;
#21651 = CARTESIAN_POINT ( 'NONE',  ( -20.75514604977248823, 63.07500000273119412, -28.56700777964554305 ) ) ;
#21652 = FILL_AREA_STYLE_COLOUR ( '', #6871 ) ;
#21653 = CARTESIAN_POINT ( 'NONE',  ( 26.29305231718579350, 40.80000000000000426, 19.10302069950537529 ) ) ;
#21654 = CARTESIAN_POINT ( 'NONE',  ( -14.47279130897152122, 9.924999997268825425, 19.92008829642072243 ) ) ;
#21655 = CARTESIAN_POINT ( 'NONE',  ( 33.58253175000000823, 2.275000002731194293, 10.91162601494192863 ) ) ;
#21656 = FACE_OUTER_BOUND ( 'NONE', #13872, .T. ) ;
#21657 = CARTESIAN_POINT ( 'NONE',  ( -11.25946833292375793, 75.57500000273120122, 8.180482586598737171 ) ) ;
#21658 = CARTESIAN_POINT ( 'NONE',  ( 6.486482029760648627E-15, 73.87500000273119838, 35.31076352940722529 ) ) ;
#21659 = CYLINDRICAL_SURFACE ( 'NONE', #25898, 32.50000000000000000 ) ;
#21660 = CARTESIAN_POINT ( 'NONE',  ( -33.58253175000000113, 71.27500000273118985, -10.91162601494193218 ) ) ;
#21661 = ORIENTED_EDGE ( 'NONE', *, *, #10556, .F. ) ;
#21662 = CARTESIAN_POINT ( 'NONE',  ( 23.41746825000000243, 17.22499999726880304, -7.608796670333727974 ) ) ;
#21663 = PRESENTATION_LAYER_ASSIGNMENT (  '', '', ( #11770 ) ) ;
#21664 = CARTESIAN_POINT ( 'NONE',  ( 26.06988505166735592, 14.87017333425730747, 7.025853678916393896 ) ) ;
#21665 = DIRECTION ( 'NONE',  ( 0.000000000000000000, 0.000000000000000000, 1.000000000000000000 ) ) ;
#21666 = CARTESIAN_POINT ( 'NONE',  ( 10.37757302488624767, 47.72500000273117848, 31.93888565452638417 ) ) ;
#21667 = CARTESIAN_POINT ( 'NONE',  ( 33.58253175000000823, 12.27500000273118452, 10.91162601494192863 ) ) ;
#21668 = CARTESIAN_POINT ( 'NONE',  ( -27.16883889988624290, 65.17500000273116711, -19.73931689729374028 ) ) ;
#21669 = CARTESIAN_POINT ( 'NONE',  ( -2.428612866367529427E-13, 53.67968750000000000, -27.95245687107223276 ) ) ;
#21670 = CARTESIAN_POINT ( 'NONE',  ( 28.00173670424549499, 42.37017333425730925, 7.543491769121417612 ) ) ;
#21671 = CARTESIAN_POINT ( 'NONE',  ( 20.53372385742108008, 32.90586833240934794, 20.47846945139866648 ) ) ;
#21672 = CARTESIAN_POINT ( 'NONE',  ( -26.29305231718579350, 70.30000000546236549, -19.10302069950537884 ) ) ;
#21673 = CARTESIAN_POINT ( 'NONE',  ( -11.25946833292375793, 76.67500000273119554, -8.180482586598733619 ) ) ;
#21674 = CARTESIAN_POINT ( 'NONE',  ( -33.58253175000000113, 39.02500000273119696, -10.91162601494193041 ) ) ;
#21675 = CARTESIAN_POINT ( 'NONE',  ( -26.09010956794245217, 58.40065999907601935, -6.950374756619243755 ) ) ;
#21676 = CARTESIAN_POINT ( 'NONE',  ( -4.523095164977116484E-15, 16.12499999726880873, 24.62258325217400312 ) ) ;
#21677 = EDGE_CURVE ( 'NONE', #6411, #19947, #3084, .T. ) ;
#21678 = CARTESIAN_POINT ( 'NONE',  ( 26.29305231718579350, 13.30000000546238681, 19.10302069950537529 ) ) ;
#21679 = EDGE_CURVE ( 'NONE', #26497, #4231, #2076, .T. ) ;
#21680 = ORIENTED_EDGE ( 'NONE', *, *, #14450, .T. ) ;
#21681 = CARTESIAN_POINT ( 'NONE',  ( 10.37757302488624767, 45.97500000273117848, 31.93888565452638417 ) ) ;
#21682 = FACE_OUTER_BOUND ( 'NONE', #32669, .T. ) ;
#21683 = CARTESIAN_POINT ( 'NONE',  ( -6.950374756619716266, 48.09934000092398065, -26.09010956794232428 ) ) ;
#21684 = CARTESIAN_POINT ( 'NONE',  ( -10.37757302488624411, 68.97500000273117848, -31.93888565452638417 ) ) ;
#21685 = VERTEX_POINT ( 'NONE', #27929 ) ;
#21686 = CARTESIAN_POINT ( 'NONE',  ( -33.58253175000000113, 17.12500000273119127, 0.000000000000000000 ) ) ;
#21687 = CARTESIAN_POINT ( 'NONE',  ( 15.01150461594596308, 26.46614583333332149, -26.00068869287367335 ) ) ;
#21688 = ORIENTED_EDGE ( 'NONE', *, *, #33358, .T. ) ;
#21689 = VERTEX_POINT ( 'NONE', #6986 ) ;
#21690 = DIRECTION ( 'NONE',  ( 0.8660254037844410391, 0.4999999999999958367, 0.000000000000000000 ) ) ;
#21691 = CARTESIAN_POINT ( 'NONE',  ( -20.75514604977248823, 56.82500000273117990, -28.56700777964554305 ) ) ;
#21692 = CARTESIAN_POINT ( 'NONE',  ( 20.50609665441005092, 61.84374999999998579, 20.50609665440969209 ) ) ;
#21693 = CARTESIAN_POINT ( 'NONE',  ( 10.04305231718579705, 21.10000000546238752, 30.90933677959248982 ) ) ;
#21694 = CARTESIAN_POINT ( 'NONE',  ( 30.16025403784430736, -21.99999999999999289, 3.693565856891707127E-15 ) ) ;
#21695 = CARTESIAN_POINT ( 'NONE',  ( -23.41746824999999887, 6.124999997268814944, -2.867812753649727150E-15 ) ) ;
#21696 = EDGE_CURVE ( 'NONE', #21685, #2770, #21318, .T. ) ;
#21697 = CARTESIAN_POINT ( 'NONE',  ( 10.37757302488624767, 21.97500000273119980, 31.93888565452638417 ) ) ;
#21698 = AXIS2_PLACEMENT_3D ( 'NONE', #18249, #31769, #23391 ) ;
#21699 = CARTESIAN_POINT ( 'NONE',  ( -32.50000000000000000, 64.10000000000000853, 10.55989012756946366 ) ) ;
#21700 = CARTESIAN_POINT ( 'NONE',  ( 13.94119854578893580, 18.15326416574268720, -24.22776226481265383 ) ) ;
#21701 = CARTESIAN_POINT ( 'NONE',  ( -8.960552108402742093E-16, 78.37500000273116996, -14.63369212191046387 ) ) ;
#21702 = CARTESIAN_POINT ( 'NONE',  ( 1.836970198721029589E-15, 74.00000000000001421, -15.00000000000000000 ) ) ;
#21703 = CARTESIAN_POINT ( 'NONE',  ( -26.29305231718578995, 8.199999999999999289, 19.10302069950538595 ) ) ;
#21704 = ORIENTED_EDGE ( 'NONE', *, *, #3277, .T. ) ;
#21705 = CARTESIAN_POINT ( 'NONE',  ( 18.94512977948576093, 3.324999997268818230, -13.76444248337722875 ) ) ;
#21706 = CARTESIAN_POINT ( 'NONE',  ( 2.688165632520823219E-15, 75.37500000273118417, 14.63369212191046387 ) ) ;
#21707 = CARTESIAN_POINT ( 'NONE',  ( 26.07999730980477437, 37.20833333333332860, -6.988114217768290004 ) ) ;
#21708 = CARTESIAN_POINT ( 'NONE',  ( -20.75514604977248823, 22.82500000273118701, -28.56700777964554305 ) ) ;
#21709 = CARTESIAN_POINT ( 'NONE',  ( -33.58253175000000113, 69.02500000273118985, -10.91162601494193218 ) ) ;
#21710 = CARTESIAN_POINT ( 'NONE',  ( -10.37757302488624411, 26.97500000273118914, -31.93888565452638417 ) ) ;
#21711 = CARTESIAN_POINT ( 'NONE',  ( 27.16883889988623935, 14.57500000273119412, -19.73931689729374384 ) ) ;
#21712 = CARTESIAN_POINT ( 'NONE',  ( -2.162160676586882350E-15, 8.875000002731189497, -35.31076352940722529 ) ) ;
#21713 = CARTESIAN_POINT ( 'NONE',  ( -19.06425588902591173, 61.56288166759063074, -19.11951029504763611 ) ) ;
#21714 = CARTESIAN_POINT ( 'NONE',  ( 33.58253175000000113, 72.22500000273119269, -10.91162601494193574 ) ) ;
#21715 = CARTESIAN_POINT ( 'NONE',  ( -20.50609665441004736, 49.81249999999999289, -20.50609665440969565 ) ) ;
#21716 = CARTESIAN_POINT ( 'NONE',  ( -24.49999999999999645, -17.00000000000000000, 3.000384657911015074E-15 ) ) ;
#21717 =( BOUNDED_CURVE ( )  B_SPLINE_CURVE ( 2, ( #20956, #26432, #13394, #23692, #8229, #2924, #2751, #4986, #18383, #20792, #28829, #5496, #20625 ),
 .UNSPECIFIED., .F., .T. ) 
 B_SPLINE_CURVE_WITH_KNOTS ( ( 3, 2, 2, 2, 2, 2, 3 ),
 ( 0.4166666666666666852, 0.4222222222222222210, 0.4333333333333333481, 0.4444444444444444198, 0.4555555555555555469, 0.4666666666666666741, 0.4722222222222222654 ),
 .UNSPECIFIED. ) 
 CURVE ( )  GEOMETRIC_REPRESENTATION_ITEM ( )  RATIONAL_B_SPLINE_CURVE ( ( 0.9755282581475767101, 0.9755282581475768211, 1.000000000000000000, 0.9510565162951535312, 1.000000000000000000, 0.9510565162951535312, 1.000000000000000000, 0.9510565162951535312, 1.000000000000000000, 0.9510565162951535312, 1.000000000000000000, 0.9755282581475765991, 0.9755282581475767101 ) ) 
 REPRESENTATION_ITEM ( '' )  );
#21718 = CARTESIAN_POINT ( 'NONE',  ( -13.91746824999999532, 75.47500000273116427, 4.522059556121122093 ) ) ;
#21719 = CARTESIAN_POINT ( 'NONE',  ( 20.08610463437157279, 55.29999999999999716, -27.64615127144129758 ) ) ;
#21720 = CARTESIAN_POINT ( 'NONE',  ( -9.270509831248423538, 71.95000000546238539, -12.75976212528059861 ) ) ;
#21721 = CARTESIAN_POINT ( 'NONE',  ( 33.58253175000000823, 60.02500000273116854, 10.91162601494192685 ) ) ;
#21722 = CARTESIAN_POINT ( 'NONE',  ( 18.94512977948576093, 15.32499999726880091, -13.76444248337722875 ) ) ;
#21723 = ORIENTED_EDGE ( 'NONE', *, *, #27657, .F. ) ;
#21724 = CARTESIAN_POINT ( 'NONE',  ( 10.37757302488624767, 67.97500000273119269, 31.93888565452638417 ) ) ;
#21725 = LINE ( 'NONE', #32171, #8131 ) ;
#21726 = VECTOR ( 'NONE', #13765, 1000.000000000000000 ) ;
#21727 = CARTESIAN_POINT ( 'NONE',  ( -23.41746825000000243, 3.524999997268826402, -7.608796670333730638 ) ) ;
#21728 = CARTESIAN_POINT ( 'NONE',  ( -27.95245687107223986, 26.75819416759064495, -0.04044903254993292840 ) ) ;
#21729 = EDGE_LOOP ( 'NONE', ( #16657, #8325, #13283, #28007 ) ) ;
#21730 = CARTESIAN_POINT ( 'NONE',  ( -2.162160676586881955E-15, 38.62500000273118417, -35.31076352940723240 ) ) ;
#21731 = DIRECTION ( 'NONE',  ( 0.000000000000000000, 0.000000000000000000, 1.000000000000000000 ) ) ;
#21732 = ORIENTED_EDGE ( 'NONE', *, *, #223, .F. ) ;
#21733 = CARTESIAN_POINT ( 'NONE',  ( -28.01184896238304134, 49.52604166666666430, -7.505752307972844761 ) ) ;
#21734 = CARTESIAN_POINT ( 'NONE',  ( 33.58253175000000113, 66.37500000273121259, -4.112674001490185761E-15 ) ) ;
#21735 = CARTESIAN_POINT ( 'NONE',  ( 20.08610463437158344, 58.70000000000000995, 27.64615127144129403 ) ) ;
#21736 = CARTESIAN_POINT ( 'NONE',  ( -2.162160676586881955E-15, 74.62500000273116996, -35.31076352940723240 ) ) ;
#21737 = CARTESIAN_POINT ( 'NONE',  ( -7.505752307973343918, 26.03645833333333215, -28.01184896238290989 ) ) ;
#21738 = CARTESIAN_POINT ( 'NONE',  ( -19.82091636218621034, 6.800000000000000711, -14.40073868116559552 ) ) ;
#21739 = CARTESIAN_POINT ( 'NONE',  ( -33.58253175000000113, 11.27500000273117031, -10.91162601494193218 ) ) ;
#21740 = CARTESIAN_POINT ( 'NONE',  ( -20.75514604977248823, 18.82500000273119767, -28.56700777964554305 ) ) ;
#21741 = CARTESIAN_POINT ( 'NONE',  ( 11.25946833292375793, 76.07500000273120122, -8.180482586598735395 ) ) ;
#21742 = DIRECTION ( 'NONE',  ( 0.000000000000000000, -1.000000000000000000, 0.000000000000000000 ) ) ;
#21743 = CARTESIAN_POINT ( 'NONE',  ( 28.00173670424535644, 39.20795166574269075, -7.543491769121920321 ) ) ;
#21744 = CARTESIAN_POINT ( 'NONE',  ( -9.657523855033125146E-16, 77.50000000000000000, -15.77193336357400710 ) ) ;
#21745 = CARTESIAN_POINT ( 'NONE',  ( 2.740863092043355209E-13, 45.08593750000000000, 30.02300923189239867 ) ) ;
#21746 = EDGE_CURVE ( 'NONE', #18703, #8542, #19699, .T. ) ;
#21747 = CARTESIAN_POINT ( 'NONE',  ( -15.14183272437242778, 9.049999994537618164, 20.84094480462497856 ) ) ;
#21748 = CARTESIAN_POINT ( 'NONE',  ( -32.50000000000000000, 54.50000000546238965, 0.000000000000000000 ) ) ;
#21749 = CARTESIAN_POINT ( 'NONE',  ( 14.01125832528330051, 63.98659749907601935, 24.18731323226221974 ) ) ;
#21750 = CARTESIAN_POINT ( 'NONE',  ( 27.16883889988623935, 46.32500000273117990, -19.73931689729374384 ) ) ;
#21751 = CARTESIAN_POINT ( 'NONE',  ( -9.657523855033125146E-16, 71.75000000546242518, -15.77193336357400710 ) ) ;
#21752 = CARTESIAN_POINT ( 'NONE',  ( -33.58253175000000113, 47.27500000273116143, -10.91162601494193218 ) ) ;
#21753 = CARTESIAN_POINT ( 'NONE',  ( 10.37757302488624767, 31.97500000273117848, 31.93888565452638417 ) ) ;
#21754 = EDGE_CURVE ( 'NONE', #17565, #1221, #20515, .T. ) ;
#21755 = CARTESIAN_POINT ( 'NONE',  ( 7.570916362186207671, 17.60000000000000497, 23.30088464923126779 ) ) ;
#21756 = CARTESIAN_POINT ( 'NONE',  ( -19.09188309203694445, 22.31250000000000000, -19.09188309203661049 ) ) ;
#21757 = CARTESIAN_POINT ( 'NONE',  ( 0.000000000000000000, 82.00000000000001421, -15.00000000000000000 ) ) ;
#21758 =( BOUNDED_CURVE ( )  B_SPLINE_CURVE ( 2, ( #17212, #19953, #4498, #33143, #33497, #32800, #30400, #1404, #19614, #9649, #30060, #9472, #1570, #6900, #3990, #14463, #24919, #27670, #25092, #12047, #17381, #27845, #4329, #25267, #1740, #12220, #18412, #20655, #26461, #33848, #5356, #31095, #10172, #7592, #13081, #31263, #7758, #18244, #20473, #28691, #18069, #5188, #26121, #23891, #10507, #2618, #20819, #15672, #18583, #17903, #28518, #23555, #7927, #28859, #19, #20985, #5013, #31435, #15495, #15836, #26293, #2782, #28356, #13248, #23386, #23721, #188, #10675, #21155, #31597, #7417, #4842, #8096, #10343, #33674, #2953, #29023, #25950, #15324, #13423, #5526, #16006, #10000, #2444, #30924, #25780, #2268, #12741, #23214, #12911, #11801, #24061, #3912, #22279, #30320, #32722, #528, #6651, #17132, #27588, #14381, #1148, #13596, #4077, #27759, #9057, #10847, #24674, #9218, #31932, #24840, #14552, #19537, #19866, #6817, #19702, #14218, #26630, #11630, #11015, #22114, #26795, #17298, #1318, #21485, #25011, #27421, #8425, #29985, #30147, #5697, #1493, #11967, #18914, #4247, #32558, #22438, #29360, #5861, #16339, #32885, #3288, #9384, #6490, #14721, #362, #21323, #16963, #31764, #8257, #18749, #29191, #16174 ),
 .UNSPECIFIED., .F., .F. ) 
 B_SPLINE_CURVE_WITH_KNOTS ( ( 3, 2, 2, 2, 2, 2, 2, 2, 2, 2, 2, 2, 2, 2, 2, 2, 2, 2, 2, 2, 2, 2, 2, 2, 2, 2, 2, 2, 2, 2, 2, 2, 2, 2, 2, 2, 2, 2, 2, 2, 2, 2, 2, 2, 2, 2, 2, 2, 2, 2, 2, 2, 2, 2, 2, 2, 2, 2, 2, 2, 2, 2, 2, 2, 2, 2, 2, 2, 2, 2, 2, 2, 2, 2, 2, 2, 3 ),
 ( 0.1554413423931151617, 0.1564102564102564097, 0.1589743589743589647, 0.1615384615384615474, 0.1641025641025641024, 0.1666666666666666574, 0.1692307692307692402, 0.1717948717948717952, 0.1743589743589743501, 0.1769230769230769329, 0.1794871794871794879, 0.1820512820512820429, 0.1846153846153846256, 0.1871794871794871806, 0.1897435897435897356, 0.1923076923076923184, 0.1948717948717948734, 0.1974358974358974284, 0.2000000000000000111, 0.2025641025641025661, 0.2051282051282051211, 0.2076923076923077038, 0.2102564102564102588, 0.2128205128205128138, 0.2153846153846153966, 0.2179487179487179516, 0.2205128205128205066, 0.2230769230769230893, 0.2256410256410256443, 0.2282051282051281993, 0.2307692307692307820, 0.2333333333333333370, 0.2358974358974358920, 0.2384615384615384470, 0.2410256410256410298, 0.2435897435897435848, 0.2461538461538461675, 0.2487179487179487225, 0.2512820512820512775, 0.2538461538461538325, 0.2564102564102563875, 0.2589743589743589980, 0.2615384615384615530, 0.2641025641025641080, 0.2666666666666666630, 0.2692307692307692180, 0.2717948717948717730, 0.2743589743589743835, 0.2769230769230769384, 0.2794871794871794934, 0.2820512820512820484, 0.2846153846153846034, 0.2871794871794871584, 0.2897435897435897689, 0.2923076923076923239, 0.2948717948717948789, 0.2974358974358974339, 0.2999999999999999889, 0.3025641025641025439, 0.3051282051282051544, 0.3076923076923077094, 0.3102564102564102644, 0.3128205128205128194, 0.3153846153846153744, 0.3179487179487179294, 0.3205128205128205399, 0.3230769230769230949, 0.3256410256410256499, 0.3282051282051281493, 0.3307692307692307598, 0.3333333333333333148, 0.3358974358974358698, 0.3384615384615384803, 0.3410256410256410353, 0.3435897435897435903, 0.3461538461538461453, 0.3477490347008075355 ),
 .UNSPECIFIED. ) 
 CURVE ( )  GEOMETRIC_REPRESENTATION_ITEM ( )  RATIONAL_B_SPLINE_CURVE ( ( 0.9769881597858880440, 0.9815054093103534605, 1.000000000000000000, 0.9510565162951535312, 1.000000000000000000, 0.9510565162951535312, 1.000000000000000000, 0.9510565162951535312, 1.000000000000000000, 0.9510565162951535312, 1.000000000000000000, 0.9510565162951535312, 1.000000000000000000, 0.9510565162951535312, 1.000000000000000000, 0.9510565162951535312, 1.000000000000000000, 0.9510565162951535312, 1.000000000000000000, 0.9510565162951535312, 1.000000000000000000, 0.9510565162951535312, 1.000000000000000000, 0.9510565162951535312, 1.000000000000000000, 0.9510565162951535312, 1.000000000000000000, 0.9510565162951535312, 1.000000000000000000, 0.9510565162951535312, 1.000000000000000000, 0.9510565162951535312, 1.000000000000000000, 0.9510565162951535312, 1.000000000000000000, 0.9510565162951535312, 1.000000000000000000, 0.9510565162951535312, 1.000000000000000000, 0.9510565162951535312, 1.000000000000000000, 0.9510565162951535312, 1.000000000000000000, 0.9510565162951535312, 1.000000000000000000, 0.9510565162951535312, 1.000000000000000000, 0.9510565162951535312, 1.000000000000000000, 0.9510565162951535312, 1.000000000000000000, 0.9510565162951535312, 1.000000000000000000, 0.9510565162951535312, 1.000000000000000000, 0.9510565162951535312, 1.000000000000000000, 0.9510565162951535312, 1.000000000000000000, 0.9510565162951535312, 1.000000000000000000, 0.9510565162951535312, 1.000000000000000000, 0.9510565162951535312, 1.000000000000000000, 0.9510565162951535312, 1.000000000000000000, 0.9510565162951535312, 1.000000000000000000, 0.9510565162951535312, 1.000000000000000000, 0.9510565162951535312, 1.000000000000000000, 0.9510565162951535312, 1.000000000000000000, 0.9510565162951535312, 1.000000000000000000, 0.9510565162951535312, 1.000000000000000000, 0.9510565162951535312, 1.000000000000000000, 0.9510565162951535312, 1.000000000000000000, 0.9510565162951535312, 1.000000000000000000, 0.9510565162951535312, 1.000000000000000000, 0.9510565162951535312, 1.000000000000000000, 0.9510565162951535312, 1.000000000000000000, 0.9510565162951535312, 1.000000000000000000, 0.9510565162951535312, 1.000000000000000000, 0.9510565162951535312, 1.000000000000000000, 0.9510565162951535312, 1.000000000000000000, 0.9510565162951535312, 1.000000000000000000, 0.9510565162951535312, 1.000000000000000000, 0.9510565162951535312, 1.000000000000000000, 0.9510565162951535312, 1.000000000000000000, 0.9510565162951535312, 1.000000000000000000, 0.9510565162951535312, 1.000000000000000000, 0.9510565162951535312, 1.000000000000000000, 0.9510565162951535312, 1.000000000000000000, 0.9510565162951535312, 1.000000000000000000, 0.9510565162951535312, 1.000000000000000000, 0.9510565162951535312, 1.000000000000000000, 0.9510565162951535312, 1.000000000000000000, 0.9510565162951535312, 1.000000000000000000, 0.9510565162951535312, 1.000000000000000000, 0.9510565162951535312, 1.000000000000000000, 0.9510565162951535312, 1.000000000000000000, 0.9510565162951535312, 1.000000000000000000, 0.9510565162951535312, 1.000000000000000000, 0.9510565162951535312, 1.000000000000000000, 0.9510565162951535312, 1.000000000000000000, 0.9510565162951535312, 1.000000000000000000, 0.9510565162951535312, 1.000000000000000000, 0.9510565162951535312, 1.000000000000000000, 0.9510565162951535312, 1.000000000000000000, 0.9510565162951535312, 1.000000000000000000, 0.9510565162951535312, 1.000000000000000000, 0.9695511069847985164, 0.9769881597858887101 ) ) 
 REPRESENTATION_ITEM ( '' )  );
#21759 = CARTESIAN_POINT ( 'NONE',  ( -2.375766604868045029, 79.55125428154684641, -14.99999999999999822 ) ) ;
#21760 = CARTESIAN_POINT ( 'NONE',  ( -32.50000000000000000, 72.09999999999999432, 10.55989012756946366 ) ) ;
#21761 = CARTESIAN_POINT ( 'NONE',  ( 20.75514604977248467, 10.42500000273120087, -28.56700777964554305 ) ) ;
#21762 = CARTESIAN_POINT ( 'NONE',  ( 23.41746824999999887, 4.724999997268818142, -7.608796670333727974 ) ) ;
#21763 = VECTOR ( 'NONE', #29390, 1000.000000000000000 ) ;
#21764 = CARTESIAN_POINT ( 'NONE',  ( -10.04305231718578462, 52.90000000546238113, 30.90933677959249337 ) ) ;
#21765 = CARTESIAN_POINT ( 'NONE',  ( 26.06988505166722803, 28.89545166574268009, -7.025853678916862854 ) ) ;
#21766 = DIRECTION ( 'NONE',  ( -0.000000000000000000, -1.000000000000000000, -0.000000000000000000 ) ) ;
#21767 = CARTESIAN_POINT ( 'NONE',  ( -33.58253175000000113, 21.22500000273117848, 10.91162601494193929 ) ) ;
#21768 = CARTESIAN_POINT ( 'NONE',  ( 14.47279130897151589, 8.824999997268804464, 19.92008829642072953 ) ) ;
#21769 = CARTESIAN_POINT ( 'NONE',  ( 13.97622843553589966, 53.96614583333333570, -24.20753774853756113 ) ) ;
#21770 = VERTEX_POINT ( 'NONE', #1490 ) ;
#21771 = CARTESIAN_POINT ( 'NONE',  ( 27.16883889988624290, 55.92500000273119554, 19.73931689729373673 ) ) ;
#21772 = VERTEX_POINT ( 'NONE', #30317 ) ;
#21773 = CARTESIAN_POINT ( 'NONE',  ( -30.02300923189239512, 21.88281249999999645, 2.654126918244515359E-13 ) ) ;
#21774 = CARTESIAN_POINT ( 'NONE',  ( 28.02196122052045268, 24.89621500092397710, -7.468012846824774620 ) ) ;
#21775 = CARTESIAN_POINT ( 'NONE',  ( -4.405589869732278832E-13, 10.49999999999998934, 32.50000000000000000 ) ) ;
#21776 = CARTESIAN_POINT ( 'NONE',  ( -18.94512977948576093, 7.824999997268822227, 13.76444248337722698 ) ) ;
#21777 = CARTESIAN_POINT ( 'NONE',  ( -27.16883889988624290, 31.17500000273118488, -19.73931689729374028 ) ) ;
#21778 = CARTESIAN_POINT ( 'NONE',  ( -2.092463501923844636E-15, 30.00000000546236478, -34.17252228774368916 ) ) ;
#21779 = CARTESIAN_POINT ( 'NONE',  ( -32.50000000000000000, 75.89999999999996305, -10.55989012756945478 ) ) ;
#21780 = CARTESIAN_POINT ( 'NONE',  ( 26.29305231718578995, 53.19999999999999574, -19.10302069950538240 ) ) ;
#21781 = DIRECTION ( 'NONE',  ( 0.000000000000000000, 0.000000000000000000, 1.000000000000000000 ) ) ;
#21782 = CARTESIAN_POINT ( 'NONE',  ( 6.486482029760649416E-15, 45.87500000273117706, 35.31076352940723240 ) ) ;
#21783 = CARTESIAN_POINT ( 'NONE',  ( 32.50000000000000711, 22.90000000000000568, 10.55989012756945122 ) ) ;
#21784 = CARTESIAN_POINT ( 'NONE',  ( 26.29305231718578995, 19.19999999999999574, -19.10302069950538240 ) ) ;
#21785 = CARTESIAN_POINT ( 'NONE',  ( -7.570916362186210335, 10.59999999999999787, -23.30088464923126779 ) ) ;
#21786 = CARTESIAN_POINT ( 'NONE',  ( 27.16883889988623935, 66.32500000273117280, -19.73931689729374384 ) ) ;
#21787 = CARTESIAN_POINT ( 'NONE',  ( 33.58253175000000113, 54.37500000273118417, -4.112674001490185761E-15 ) ) ;
#21788 = CARTESIAN_POINT ( 'NONE',  ( -7.236395654485763274, 12.02499999726880375, 22.27133577429736633 ) ) ;
#21789 = CARTESIAN_POINT ( 'NONE',  ( 7.570916362186207671, 3.599999999999992095, 23.30088464923126779 ) ) ;
#21790 = CARTESIAN_POINT ( 'NONE',  ( 10.37757302488624056, 6.525000002731207616, -31.93888565452638417 ) ) ;
#21791 = CARTESIAN_POINT ( 'NONE',  ( 19.06425588902592239, 39.21913166759063785, 19.11951029504763611 ) ) ;
#21792 = CARTESIAN_POINT ( 'NONE',  ( -13.91746824999999887, 81.37500000273118417, 0.000000000000000000 ) ) ;
#21793 = CARTESIAN_POINT ( 'NONE',  ( -10.28315354913682711, 52.00000000000000000, 31.56665548893541029 ) ) ;
#21794 = CARTESIAN_POINT ( 'NONE',  ( -10.37757302488624411, 26.72500000273118914, -31.93888565452638417 ) ) ;
#21795 = CARTESIAN_POINT ( 'NONE',  ( 20.08610463437157279, 61.80000000546237970, -27.64615127144129758 ) ) ;
#21796 = CARTESIAN_POINT ( 'NONE',  ( -20.08610463437156923, 30.80000000546237615, 27.64615127144130113 ) ) ;
#21797 = CARTESIAN_POINT ( 'NONE',  ( 25.98046417659831775, 56.25222249907602645, -15.04653450569338879 ) ) ;
#21798 = CARTESIAN_POINT ( 'NONE',  ( -26.29305231718579350, 50.30000000546237970, -19.10302069950537884 ) ) ;
#21799 = CARTESIAN_POINT ( 'NONE',  ( 2.694222958124179176E-15, -45.00000000000001421, 0.000000000000000000 ) ) ;
#21800 = CARTESIAN_POINT ( 'NONE',  ( -32.50000000000000000, 58.60000000546236265, 10.55989012756946366 ) ) ;
#21801 = CARTESIAN_POINT ( 'NONE',  ( -26.07999730980477437, 28.61458333333333215, 6.988114217768305103 ) ) ;
#21802 = AXIS2_PLACEMENT_3D ( 'NONE', #24588, #24424, #6397 ) ;
#21803 = CARTESIAN_POINT ( 'NONE',  ( -27.16883889988624290, 72.92500000273120975, -19.73931689729374028 ) ) ;
#21804 = CARTESIAN_POINT ( 'NONE',  ( 20.50609665440969565, 30.04687500000000000, -20.50609665441004736 ) ) ;
#21805 = PLANE ( 'NONE',  #14643 ) ;
#21806 = ORIENTED_EDGE ( 'NONE', *, *, #13556, .F. ) ;
#21807 = CARTESIAN_POINT ( 'NONE',  ( -14.97647472619946285, 51.39361083425730925, -26.02091320914851025 ) ) ;
#21808 = CARTESIAN_POINT ( 'NONE',  ( 10.04305231718579705, 13.10000000546239463, 30.90933677959248982 ) ) ;
#21809 =( BOUNDED_CURVE ( )  B_SPLINE_CURVE ( 2, ( #18454, #5227, #23594, #25991, #2658, #23427, #28897, #10889, #21363, #10379, #31806, #18286, #13289 ),
 .UNSPECIFIED., .F., .F. ) 
 B_SPLINE_CURVE_WITH_KNOTS ( ( 3, 2, 2, 2, 2, 2, 3 ),
 ( 0.2500000000000000000, 0.2555555555555555358, 0.2666666666666666630, 0.2777777777777777901, 0.2888888888888888618, 0.2999999999999999889, 0.3055555555555555802 ),
 .UNSPECIFIED. ) 
 CURVE ( )  GEOMETRIC_REPRESENTATION_ITEM ( )  RATIONAL_B_SPLINE_CURVE ( ( 0.9755282581475768211, 0.9755282581475768211, 1.000000000000000000, 0.9510565162951535312, 1.000000000000000000, 0.9510565162951535312, 1.000000000000000000, 0.9510565162951535312, 1.000000000000000000, 0.9510565162951535312, 1.000000000000000000, 0.9755282581475765991, 0.9755282581475767101 ) ) 
 REPRESENTATION_ITEM ( '' )  );
#21810 = CARTESIAN_POINT ( 'NONE',  ( -26.00068869287340334, 59.40885416666666430, 15.01150461594643382 ) ) ;
#21811 = CARTESIAN_POINT ( 'NONE',  ( 26.29305231718579350, 20.79999999999998650, 19.10302069950537529 ) ) ;
#21812 = CARTESIAN_POINT ( 'NONE',  ( -20.75514604977248112, 47.67500000273118843, 28.56700777964554661 ) ) ;
#21813 = CARTESIAN_POINT ( 'NONE',  ( -32.50000000000000000, 50.60000000546236265, 10.55989012756946366 ) ) ;
#21814 = CARTESIAN_POINT ( 'NONE',  ( -4.300734207923759378, 78.97500000273122112, -13.23629886949340495 ) ) ;
#21815 = CARTESIAN_POINT ( 'NONE',  ( 6.486482029760649416E-15, 35.62500000273119127, 35.31076352940723240 ) ) ;
#21816 = CARTESIAN_POINT ( 'NONE',  ( 5.878266837044421923E-15, -70.99969134886156041, 0.000000000000000000 ) ) ;
#21817 = CARTESIAN_POINT ( 'NONE',  ( -33.58253175000000113, 63.27500000273118985, -10.91162601494193218 ) ) ;
#21818 = DIRECTION ( 'NONE',  ( 1.000000000000000000, 0.000000000000000000, 0.000000000000000000 ) ) ;
#21819 = CARTESIAN_POINT ( 'NONE',  ( -26.29305231718579350, 39.80000000000000426, -19.10302069950537884 ) ) ;
#21820 = CARTESIAN_POINT ( 'NONE',  ( -4.523095164977116484E-15, 14.12499999726881050, 24.62258325217400312 ) ) ;
#21821 = EDGE_CURVE ( 'NONE', #15868, #18620, #20900, .T. ) ;
#21822 = CARTESIAN_POINT ( 'NONE',  ( -33.58253175000000113, 3.375000002731193049, 0.000000000000000000 ) ) ;
#21823 = CARTESIAN_POINT ( 'NONE',  ( -19.09188309203694445, 11.99999999999999645, -19.09188309203661049 ) ) ;
#21824 = CYLINDRICAL_SURFACE ( 'NONE', #11679, 24.50000000000000000 ) ;
#21825 = CARTESIAN_POINT ( 'NONE',  ( -10.37757302488623701, 73.77500000273118985, 31.93888565452638417 ) ) ;
#21826 = CARTESIAN_POINT ( 'NONE',  ( 7.890940483122900408E-14, 18.24999999453761745, -24.50000000000000000 ) ) ;
#21827 = ADVANCED_FACE ( 'NONE', ( #7841 ), #31181, .F. ) ;
#21828 = CARTESIAN_POINT ( 'NONE',  ( -27.16883889988624290, 67.17500000273118133, -19.73931689729374028 ) ) ;
#21829 = VERTEX_POINT ( 'NONE', #12827 ) ;
#21830 = CARTESIAN_POINT ( 'NONE',  ( -15.14183272437242600, 5.049999994537627934, 20.84094480462497856 ) ) ;
#21831 = VECTOR ( 'NONE', #18344, 1000.000000000000114 ) ;
#21832 = CARTESIAN_POINT ( 'NONE',  ( -27.95245687107223986, 13.00819416759064318, -0.04044903254993292840 ) ) ;
#21833 = FACE_OUTER_BOUND ( 'NONE', #15052, .T. ) ;
#21834 = CARTESIAN_POINT ( 'NONE',  ( -27.16883889988623935, 49.32500000273120122, 19.73931689729374739 ) ) ;
#21835 = CARTESIAN_POINT ( 'NONE',  ( -20.75514604977248112, 13.67500000273118133, 28.56700777964554661 ) ) ;
#21836 = CARTESIAN_POINT ( 'NONE',  ( -10.37757302488624411, 62.97500000273119269, -31.93888565452638417 ) ) ;
#21837 = CARTESIAN_POINT ( 'NONE',  ( -2.428612866367529427E-13, 50.24218750000000711, -27.95245687107223276 ) ) ;
#21838 = CARTESIAN_POINT ( 'NONE',  ( 20.53372385742072481, 38.35975666759064495, -20.47846945139902175 ) ) ;
#21839 = CARTESIAN_POINT ( 'NONE',  ( -25.98046417659831420, 30.47097249907602290, 15.04653450569339945 ) ) ;
#21840 = CARTESIAN_POINT ( 'NONE',  ( 32.50000000000000000, 69.50000000546239676, -3.980102097228898626E-15 ) ) ;
#21841 = CARTESIAN_POINT ( 'NONE',  ( 8.601468415847520532, 79.57500000273117280, 11.83890561707634781 ) ) ;
#21842 = CARTESIAN_POINT ( 'NONE',  ( 24.22776226481265383, 56.82513916574268364, 13.94119854578893580 ) ) ;
#21843 = CARTESIAN_POINT ( 'NONE',  ( -18.94512977948576093, 13.82499999726879913, 13.76444248337722698 ) ) ;
#21844 = CARTESIAN_POINT ( 'NONE',  ( -19.82091636218621034, 4.549999994537618164, -14.40073868116559552 ) ) ;
#21845 = ORIENTED_EDGE ( 'NONE', *, *, #15985, .T. ) ;
#21846 = CARTESIAN_POINT ( 'NONE',  ( 33.58253175000000823, 50.27500000273118985, 10.91162601494192863 ) ) ;
#21847 = CARTESIAN_POINT ( 'NONE',  ( 23.41746824999999887, 1.224999997268811480, -7.608796670333727974 ) ) ;
#21848 = CARTESIAN_POINT ( 'NONE',  ( -27.95245687107223986, 50.82069416759063785, -0.04044903254993292840 ) ) ;
#21849 = CARTESIAN_POINT ( 'NONE',  ( -20.75514604977248823, 67.07500000273118701, -28.56700777964554305 ) ) ;
#21850 = VERTEX_POINT ( 'NONE', #4927 ) ;
#21851 = CARTESIAN_POINT ( 'NONE',  ( -27.16883889988624290, 16.92500000273118488, -19.73931689729374028 ) ) ;
#21852 = CARTESIAN_POINT ( 'NONE',  ( 28.01184896238290278, 23.45833333333333215, -7.505752307973347470 ) ) ;
#21853 = VERTEX_POINT ( 'NONE', #23119 ) ;
#21854 = CARTESIAN_POINT ( 'NONE',  ( 0.000000000000000000, 70.00000000000000000, 0.000000000000000000 ) ) ;
#21855 = CARTESIAN_POINT ( 'NONE',  ( 27.16883889988623935, 56.32500000273118701, -19.73931689729374384 ) ) ;
#21856 = CARTESIAN_POINT ( 'NONE',  ( 28.01184896238290278, 57.83333333333333570, -7.505752307973347470 ) ) ;
#21857 = CARTESIAN_POINT ( 'NONE',  ( -26.29305231718579350, 10.30000000546238326, -19.10302069950537884 ) ) ;
#21858 = CARTESIAN_POINT ( 'NONE',  ( 1.093617666956751375E-13, 66.00000000546238255, -32.50000000000000711 ) ) ;
#21859 = CARTESIAN_POINT ( 'NONE',  ( 14.47279130897151944, 15.42499999726883075, -19.92008829642072598 ) ) ;
#21860 = ADVANCED_FACE ( 'NONE', ( #15754 ), #15407, .F. ) ;
#21861 = CARTESIAN_POINT ( 'NONE',  ( -33.58253175000000113, 25.37500000273118417, 0.000000000000000000 ) ) ;
#21862 = CARTESIAN_POINT ( 'NONE',  ( -20.08610463437156923, 24.80000000546235839, 27.64615127144130113 ) ) ;
#21863 = CARTESIAN_POINT ( 'NONE',  ( -19.06425588902558133, 16.57774333240934794, 19.11951029504797006 ) ) ;
#21864 = CARTESIAN_POINT ( 'NONE',  ( 4.300734207923761154, 79.47500000273119269, 13.23629886949340495 ) ) ;
#21865 = CARTESIAN_POINT ( 'NONE',  ( -10.04305231718579172, 11.59999999999998543, -30.90933677959248982 ) ) ;
#21866 = ORIENTED_EDGE ( 'NONE', *, *, #15625, .T. ) ;
#21867 = CARTESIAN_POINT ( 'NONE',  ( 23.41746824999999887, 7.124999997268815832, 0.000000000000000000 ) ) ;
#21868 = CARTESIAN_POINT ( 'NONE',  ( 2.688165632520823219E-15, 73.37500000273118417, 14.63369212191046387 ) ) ;
#21869 = CARTESIAN_POINT ( 'NONE',  ( 6.988114217768294445, 41.50520833333333570, 26.07999730980477437 ) ) ;
#21870 = CARTESIAN_POINT ( 'NONE',  ( 10.37757302488624767, 19.72500000273119625, 31.93888565452638417 ) ) ;
#21871 = CARTESIAN_POINT ( 'NONE',  ( 10.37757302488624056, 68.52500000273118985, -31.93888565452638417 ) ) ;
#21872 = CARTESIAN_POINT ( 'NONE',  ( -33.58253175000000113, 29.27500000273118630, -10.91162601494193218 ) ) ;
#21873 = CARTESIAN_POINT ( 'NONE',  ( -27.16883889988624290, 19.17500000273118843, -19.73931689729374028 ) ) ;
#21874 = CARTESIAN_POINT ( 'NONE',  ( -27.16883889988623935, 9.575000002731204773, 19.73931689729374739 ) ) ;
#21875 = CARTESIAN_POINT ( 'NONE',  ( 25.98046417659858420, 11.57590250092397355, 15.04653450569292872 ) ) ;
#21876 = CARTESIAN_POINT ( 'NONE',  ( -2.584737979205441561E-13, 50.24218750000000711, -30.02300923189239512 ) ) ;
#21877 = LINE ( 'NONE', #18975, #30808 ) ;
#21878 = CARTESIAN_POINT ( 'NONE',  ( 11.25946833292375793, 78.17500000273119554, 8.180482586598731842 ) ) ;
#21879 = CARTESIAN_POINT ( 'NONE',  ( 10.04305231718579705, 46.60000000000001563, 30.90933677959248982 ) ) ;
#21880 = DIRECTION ( 'NONE',  ( 0.000000000000000000, 0.000000000000000000, 1.000000000000000000 ) ) ;
#21881 = CARTESIAN_POINT ( 'NONE',  ( -10.37757302488624411, 48.72500000273119269, -31.93888565452638417 ) ) ;
#21882 = CARTESIAN_POINT ( 'NONE',  ( 23.41746825000000243, 17.02499999726880731, 7.608796670333735079 ) ) ;
#21883 = VERTEX_POINT ( 'NONE', #18330 ) ;
#21884 = CARTESIAN_POINT ( 'NONE',  ( -27.16883889988623935, 67.57500000273118701, 19.73931689729374739 ) ) ;
#21885 = CARTESIAN_POINT ( 'NONE',  ( -10.37757302488624411, 2.725000002731181592, -31.93888565452638417 ) ) ;
#21886 = CARTESIAN_POINT ( 'NONE',  ( 23.41746825000000243, 6.524999997268818852, 7.608796670333735079 ) ) ;
#21887 = CARTESIAN_POINT ( 'NONE',  ( -26.09010956794232428, 23.17746500092398065, 6.950374756619732253 ) ) ;
#21888 = ORIENTED_EDGE ( 'NONE', *, *, #9080, .F. ) ;
#21889 = CARTESIAN_POINT ( 'NONE',  ( 27.16883889988623935, 36.32500000273118701, -19.73931689729374384 ) ) ;
#21890 = CARTESIAN_POINT ( 'NONE',  ( -24.50000000000000000, 1.000000000000000888, -3.000384657911015469E-15 ) ) ;
#21891 = EDGE_LOOP ( 'NONE', ( #30602, #17283, #22346, #33042 ) ) ;
#21892 = CARTESIAN_POINT ( 'NONE',  ( 26.00068869287367335, 51.38802083333332149, 15.01150461594596308 ) ) ;
#21893 = CARTESIAN_POINT ( 'NONE',  ( 33.58253175000000113, 62.47500000273118559, -10.91162601494193751 ) ) ;
#21894 = CARTESIAN_POINT ( 'NONE',  ( 20.08610463437157279, 69.80000000546239391, -27.64615127144129758 ) ) ;
#21895 = CARTESIAN_POINT ( 'NONE',  ( -33.58253175000000113, 77.02500000273118985, -10.91162601494193218 ) ) ;
#21896 = CARTESIAN_POINT ( 'NONE',  ( 7.505752307972854531, 26.32291666666666075, -28.01184896238303423 ) ) ;
#21897 = CARTESIAN_POINT ( 'NONE',  ( 24.50000000000000000, 4.000000000000003553, 0.000000000000000000 ) ) ;
#21898 = CARTESIAN_POINT ( 'NONE',  ( 33.58253175000000113, 6.375000002731168181, -4.112674001490185761E-15 ) ) ;
#21899 = CARTESIAN_POINT ( 'NONE',  ( -33.58253175000000113, 15.02500000273120051, -10.91162601494193218 ) ) ;
#21900 = CARTESIAN_POINT ( 'NONE',  ( -8.601468415847518756, 74.57500000273117280, -11.83890561707634603 ) ) ;
#21901 = CARTESIAN_POINT ( 'NONE',  ( 15.04653450569339945, 46.79909749907603356, 25.98046417659831775 ) ) ;
#21902 = CARTESIAN_POINT ( 'NONE',  ( 15.00000000000000000, 81.09999999999999432, -4.873795443493596835 ) ) ;
#21903 = CARTESIAN_POINT ( 'NONE',  ( 7.505752307973351023, 44.94270833333332860, 28.01184896238290278 ) ) ;
#21904 = PRODUCT_RELATED_PRODUCT_CATEGORY ( 'part', '', ( #9557 ) ) ;
#21905 = CARTESIAN_POINT ( 'NONE',  ( -7.570916362186210335, 10.59999999999999787, -23.30088464923126779 ) ) ;
#21906 = CARTESIAN_POINT ( 'NONE',  ( 10.04305231718579705, 70.59999999999999432, 30.90933677959248982 ) ) ;
#21907 = CARTESIAN_POINT ( 'NONE',  ( 6.988114217767829928, 16.01041666666666075, -26.07999730980489872 ) ) ;
#21908 =( BOUNDED_CURVE ( )  B_SPLINE_CURVE ( 2, ( #16716, #22030, #23475, #13519, #15928, #454, #13344, #32474, #23816, #19287, #33937, #21247, #10770 ),
 .UNSPECIFIED., .F., .F. ) 
 B_SPLINE_CURVE_WITH_KNOTS ( ( 3, 2, 2, 2, 2, 2, 3 ),
 ( 0.1858974358974359031, 0.1871794871794871806, 0.1897435897435897356, 0.1923076923076923184, 0.1948717948717948734, 0.1974358974358974284, 0.1987179487179487336 ),
 .UNSPECIFIED. ) 
 CURVE ( )  GEOMETRIC_REPRESENTATION_ITEM ( )  RATIONAL_B_SPLINE_CURVE ( ( 0.9755282581475768211, 0.9755282581475768211, 1.000000000000000000, 0.9510565162951535312, 1.000000000000000000, 0.9510565162951535312, 1.000000000000000000, 0.9510565162951535312, 1.000000000000000000, 0.9510565162951535312, 1.000000000000000000, 0.9755282581475764880, 0.9755282581475768211 ) ) 
 REPRESENTATION_ITEM ( '' )  );
#21909 = CARTESIAN_POINT ( 'NONE',  ( -10.37757302488624411, 46.72500000273119269, -31.93888565452638417 ) ) ;
#21910 = CARTESIAN_POINT ( 'NONE',  ( -4.300734207923755825, 75.27500000273118985, 13.23629886949340673 ) ) ;
#21911 = CARTESIAN_POINT ( 'NONE',  ( 6.486482029760649416E-15, 47.87500000273117706, 35.31076352940723240 ) ) ;
#21912 = CARTESIAN_POINT ( 'NONE',  ( 20.75514604977248467, 28.67500000273117422, -28.56700777964554305 ) ) ;
#21913 = CARTESIAN_POINT ( 'NONE',  ( 21.64573397815488676, 16.99999999999998579, 8.935324268693841887 ) ) ;
#21914 = CARTESIAN_POINT ( 'NONE',  ( -26.07999730980490583, 18.58854166666666430, -6.988114217767815717 ) ) ;
#21915 = DIRECTION ( 'NONE',  ( 0.000000000000000000, 1.000000000000000000, 0.000000000000000000 ) ) ;
#21916 = CARTESIAN_POINT ( 'NONE',  ( -8.891200544363830713E-16, 79.49999999999998579, -15.00000000000000000 ) ) ;
#21917 = CARTESIAN_POINT ( 'NONE',  ( 32.50000000000000000, 65.10000000000000853, -10.55989012756945833 ) ) ;
#21918 = CARTESIAN_POINT ( 'NONE',  ( -20.75514604977248823, 8.825000002731190563, -28.56700777964554305 ) ) ;
#21919 = CARTESIAN_POINT ( 'NONE',  ( -23.41746824999999887, 1.624999997268811169, -2.867812753649727150E-15 ) ) ;
#21920 = CARTESIAN_POINT ( 'NONE',  ( -24.50000000000000000, 10.64999999453762669, -7.960532557706207157 ) ) ;
#21921 = CARTESIAN_POINT ( 'NONE',  ( 13.94119854578893580, 25.02826416574268720, -24.22776226481265383 ) ) ;
#21922 = CARTESIAN_POINT ( 'NONE',  ( -4.223320258572819786E-15, 13.50000000000000355, 24.50000000000000000 ) ) ;
#21923 = CARTESIAN_POINT ( 'NONE',  ( -2.162160676586882350E-15, 16.62500000273120548, -35.31076352940722529 ) ) ;
#21924 = CARTESIAN_POINT ( 'NONE',  ( 7.236395654485755280, 2.724999997268801266, 22.27133577429736988 ) ) ;
#21925 = CARTESIAN_POINT ( 'NONE',  ( -19.09188309203660694, 55.82812499999999289, 19.09188309203694800 ) ) ;
#21926 = VERTEX_POINT ( 'NONE', #7505 ) ;
#21927 = CARTESIAN_POINT ( 'NONE',  ( 10.37757302488624767, 53.72500000273118559, 31.93888565452638417 ) ) ;
#21928 = CARTESIAN_POINT ( 'NONE',  ( 6.486482029760649416E-15, 27.87500000273120193, 35.31076352940723240 ) ) ;
#21929 = VERTEX_POINT ( 'NONE', #28775 ) ;
#21930 = CARTESIAN_POINT ( 'NONE',  ( -7.505752307972844761, 24.60416666666666430, 28.01184896238304134 ) ) ;
#21931 = CARTESIAN_POINT ( 'NONE',  ( -28.02196122052045268, 23.17746500092398065, 7.468012846824790607 ) ) ;
#21932 = CARTESIAN_POINT ( 'NONE',  ( -10.37757302488623701, 1.525000002731188964, 31.93888565452638417 ) ) ;
#21933 = CARTESIAN_POINT ( 'NONE',  ( 15.14183272437242245, 18.04999999453762172, -20.84094480462497856 ) ) ;
#21934 = APPLICATION_CONTEXT ( 'automotive_design' ) ;
#21935 = CARTESIAN_POINT ( 'NONE',  ( 23.41746824999999887, 8.624999997268817609, 0.000000000000000000 ) ) ;
#21936 = CARTESIAN_POINT ( 'NONE',  ( -33.58253175000000113, 29.37500000273118772, 0.000000000000000000 ) ) ;
#21937 = CARTESIAN_POINT ( 'NONE',  ( -2.092463501923844636E-15, 28.00000000546237544, -34.17252228774368916 ) ) ;
#21938 = CARTESIAN_POINT ( 'NONE',  ( -2.092463501923844636E-15, 75.50000000000001421, -34.17252228774368916 ) ) ;
#21939 = CARTESIAN_POINT ( 'NONE',  ( -4.000000000000003553, 0.000000000000000000, 0.000000000000000000 ) ) ;
#21940 = DIRECTION ( 'NONE',  ( -0.000000000000000000, -1.000000000000000000, -0.000000000000000000 ) ) ;
#21941 = CARTESIAN_POINT ( 'NONE',  ( -25.98046417659859486, 54.54465250092398776, -15.04653450569291628 ) ) ;
#21942 = CARTESIAN_POINT ( 'NONE',  ( 27.16883889988623935, 40.57500000273117280, -19.73931689729374384 ) ) ;
#21943 = CARTESIAN_POINT ( 'NONE',  ( 7.236395654485760609, 7.524999997268800200, -22.27133577429736633 ) ) ;
#21944 = CARTESIAN_POINT ( 'NONE',  ( -20.08610463437157989, 13.70000000000000462, -27.64615127144129758 ) ) ;
#21945 = CARTESIAN_POINT ( 'NONE',  ( -24.50000000000000000, 15.00000000000001421, -3.000384657911015469E-15 ) ) ;
#21946 = CARTESIAN_POINT ( 'NONE',  ( 24.18731323226221974, 39.06472249907601935, -14.01125832528328985 ) ) ;
#21947 = CARTESIAN_POINT ( 'NONE',  ( -27.16883889988624290, 62.92500000273118843, -19.73931689729374028 ) ) ;
#21948 = CARTESIAN_POINT ( 'NONE',  ( -20.75514604977248112, 45.67500000273118843, 28.56700777964554661 ) ) ;
#21949 = CARTESIAN_POINT ( 'NONE',  ( -23.41746824999999887, 11.52499999726880553, -7.608796670333730638 ) ) ;
#21950 = EDGE_CURVE ( 'NONE', #29891, #27031, #10582, .T. ) ;
#21951 = CARTESIAN_POINT ( 'NONE',  ( 5.147494310547434893, 39.05125428700922185, 32.49999999999999289 ) ) ;
#21952 = CARTESIAN_POINT ( 'NONE',  ( 27.16883889988624290, 7.925000002731191984, 19.73931689729373673 ) ) ;
#21953 = CARTESIAN_POINT ( 'NONE',  ( -26.06988505166735237, 37.21392333425730214, -7.025853678916388567 ) ) ;
#21954 = EDGE_CURVE ( 'NONE', #33710, #5395, #7672, .T. ) ;
#21955 = CARTESIAN_POINT ( 'NONE',  ( 32.50000000000000000, 66.99999999999998579, -3.980102097228898626E-15 ) ) ;
#21956 = CARTESIAN_POINT ( 'NONE',  ( -26.29305231718578995, 20.19999999999999574, 19.10302069950538595 ) ) ;
#21957 = UNCERTAINTY_MEASURE_WITH_UNIT (LENGTH_MEASURE( 1.000000000000000082E-05 ), #13404, 'distance_accuracy_value', 'NONE');
#21958 = CARTESIAN_POINT ( 'NONE',  ( -20.75514604977248112, 27.42500000273118488, 28.56700777964554661 ) ) ;
#21959 = CARTESIAN_POINT ( 'NONE',  ( 5.147494310547434893, 56.55125428154684641, 32.49999999999999289 ) ) ;
#21960 = CARTESIAN_POINT ( 'NONE',  ( 32.50000000000000000, 1.500000005462381880, -3.980102097228898626E-15 ) ) ;
#21961 = ADVANCED_FACE ( 'NONE', ( #31008 ), #2353, .T. ) ;
#21962 = CARTESIAN_POINT ( 'NONE',  ( -0.04044903255044120238, 52.24180583240936215, -30.02300923189239867 ) ) ;
#21963 = CARTESIAN_POINT ( 'NONE',  ( -10.04305231718578462, 46.90000000546238823, 30.90933677959249337 ) ) ;
#21964 = DIRECTION ( 'NONE',  ( 0.000000000000000000, 0.000000000000000000, 1.000000000000000000 ) ) ;
#21965 = CARTESIAN_POINT ( 'NONE',  ( 40.00000000000000000, 66.99999999999998579, 23.09401076758503990 ) ) ;
#21966 = CARTESIAN_POINT ( 'NONE',  ( -2.428612866367529427E-13, 29.61718749999999645, -27.95245687107222921 ) ) ;
#21967 = ORIENTED_EDGE ( 'NONE', *, *, #9886, .F. ) ;
#21968 = CARTESIAN_POINT ( 'NONE',  ( -2.162160676586881955E-15, 72.62500000273118417, -35.31076352940723240 ) ) ;
#21969 = CARTESIAN_POINT ( 'NONE',  ( 15.01150461594596308, 33.34114583333332860, -26.00068869287367335 ) ) ;
#21970 = CARTESIAN_POINT ( 'NONE',  ( 40.00000000000000000, 52.00000000000000711, 23.09401076758503990 ) ) ;
#21971 = VERTEX_POINT ( 'NONE', #20739 ) ;
#21972 = CARTESIAN_POINT ( 'NONE',  ( -0.04044903254990864921, 49.96131916759065206, 30.02300923189239867 ) ) ;
#21973 = CARTESIAN_POINT ( 'NONE',  ( -20.08610463437156923, 12.80000000546237615, 27.64615127144130113 ) ) ;
#21974 = CARTESIAN_POINT ( 'NONE',  ( -28.01184896238304134, 63.27604166666667140, -7.505752307972844761 ) ) ;
#21975 = CARTESIAN_POINT ( 'NONE',  ( -32.50000000000000000, 46.40000000546237402, -10.55989012756945300 ) ) ;
#21976 = CARTESIAN_POINT ( 'NONE',  ( -10.37757302488624411, 44.97500000273119269, -31.93888565452638417 ) ) ;
#21977 = CARTESIAN_POINT ( 'NONE',  ( -20.08610463437156923, 52.80000000546237260, 27.64615127144130113 ) ) ;
#21978 = CARTESIAN_POINT ( 'NONE',  ( 12.13525491562420910, 81.19999999999998863, -8.816778784387098611 ) ) ;
#21979 = CARTESIAN_POINT ( 'NONE',  ( -27.16883889988623935, 33.32500000273120122, 19.73931689729374739 ) ) ;
#21980 = CARTESIAN_POINT ( 'NONE',  ( 32.50000000000000000, 77.50000000546236834, -3.980102097228898626E-15 ) ) ;
#21981 = CARTESIAN_POINT ( 'NONE',  ( -33.58253175000000113, 61.47500000273117848, 10.91162601494193929 ) ) ;
#21982 =( NAMED_UNIT ( * ) PLANE_ANGLE_UNIT ( ) SI_UNIT ( $, .RADIAN. ) );
#21983 = CARTESIAN_POINT ( 'NONE',  ( 32.50000000000000711, 38.89999999999999147, 10.55989012756945122 ) ) ;
#21984 = CARTESIAN_POINT ( 'NONE',  ( 32.50000000000000000, 43.10000000000000853, -10.55989012756945833 ) ) ;
#21985 = CARTESIAN_POINT ( 'NONE',  ( -7.236395654485757944, 11.22499999726880837, -22.27133577429736988 ) ) ;
#21986 = CARTESIAN_POINT ( 'NONE',  ( 10.37757302488624767, 5.975000002731184701, 31.93888565452638417 ) ) ;
#21987 = DIRECTION ( 'NONE',  ( 1.000000000000000000, 1.309225264888156377E-16, 0.000000000000000000 ) ) ;
#21988 = CARTESIAN_POINT ( 'NONE',  ( 13.91746824999999887, 80.37500000273118417, -1.704398294459741270E-15 ) ) ;
#21989 = CARTESIAN_POINT ( 'NONE',  ( 20.75514604977249178, 74.07500000273120122, 28.56700777964553950 ) ) ;
#21990 = CARTESIAN_POINT ( 'NONE',  ( 3.880418787951139592, 3.301254276084478523, 24.50000000000000000 ) ) ;
#21991 = CARTESIAN_POINT ( 'NONE',  ( 6.486482029760649416E-15, 65.87500000273119838, 35.31076352940723240 ) ) ;
#21992 = ORIENTED_EDGE ( 'NONE', *, *, #31174, .T. ) ;
#21993 = CARTESIAN_POINT ( 'NONE',  ( -15.14183272437241889, 4.449999994537617631, -20.84094480462497856 ) ) ;
#21994 = CARTESIAN_POINT ( 'NONE',  ( 24.20753774853756113, 65.13802083333334281, 13.97622843553589789 ) ) ;
#21995 = LINE ( 'NONE', #8944, #23958 ) ;
#21996 = CARTESIAN_POINT ( 'NONE',  ( 33.58253175000000113, 48.12500000273119127, -4.112674001490185761E-15 ) ) ;
#21997 = CARTESIAN_POINT ( 'NONE',  ( 10.37757302488624767, 11.97500000273120335, 31.93888565452638417 ) ) ;
#21998 = CARTESIAN_POINT ( 'NONE',  ( 33.58253175000000823, 60.27500000273116143, 10.91162601494192685 ) ) ;
#21999 = CARTESIAN_POINT ( 'NONE',  ( 26.07999730980490227, 47.80729166666666430, 6.988114217767821046 ) ) ;
#22000 = CARTESIAN_POINT ( 'NONE',  ( 15.04653450569292872, 34.77902750092397355, -25.98046417659857710 ) ) ;
#22001 = CARTESIAN_POINT ( 'NONE',  ( 0.04044903255045854962, 26.46055583240935505, 30.02300923189239867 ) ) ;
#22002 = CARTESIAN_POINT ( 'NONE',  ( -26.29305231718578995, 68.70000000546237118, 19.10302069950538595 ) ) ;
#22003 = AXIS2_PLACEMENT_3D ( 'NONE', #16336, #13752, #24222 ) ;
#22004 = CARTESIAN_POINT ( 'NONE',  ( 13.91746824999999887, 77.87500000273116996, -1.704398294459741270E-15 ) ) ;
#22005 = CARTESIAN_POINT ( 'NONE',  ( 24.18731323226221974, 56.25222249907602645, -14.01125832528328985 ) ) ;
#22006 = FACE_OUTER_BOUND ( 'NONE', #3693, .T. ) ;
#22007 = CARTESIAN_POINT ( 'NONE',  ( 26.29305231718578995, 59.20000000000000284, -19.10302069950538240 ) ) ;
#22008 = ORIENTED_EDGE ( 'NONE', *, *, #14197, .F. ) ;
#22009 = ADVANCED_FACE ( 'NONE', ( #4755 ), #2869, .F. ) ;
#22010 = CARTESIAN_POINT ( 'NONE',  ( 20.75514604977248467, 42.67500000273119554, -28.56700777964554305 ) ) ;
#22011 = CARTESIAN_POINT ( 'NONE',  ( 2.445080149700053643E-15, 76.50000000000001421, 15.00000000000000000 ) ) ;
#22012 = AXIS2_PLACEMENT_3D ( 'NONE', #27755, #22602, #4243 ) ;
#22013 = CARTESIAN_POINT ( 'NONE',  ( -20.08610463437157989, 28.20000000546236762, -27.64615127144129758 ) ) ;
#22014 = VERTEX_POINT ( 'NONE', #18158 ) ;
#22015 = CARTESIAN_POINT ( 'NONE',  ( 10.37757302488624056, 20.52500000273117919, -31.93888565452638417 ) ) ;
#22016 = CARTESIAN_POINT ( 'NONE',  ( 26.00068869287340334, 37.06510416666666430, -15.01150461594642316 ) ) ;
#22017 = ORIENTED_EDGE ( 'NONE', *, *, #17336, .T. ) ;
#22018 = VERTEX_POINT ( 'NONE', #28436 ) ;
#22019 = CARTESIAN_POINT ( 'NONE',  ( 32.50000000000000711, 26.89999999999999503, 10.55989012756945122 ) ) ;
#22020 = CARTESIAN_POINT ( 'NONE',  ( -20.75514604977248112, 55.42500000273119554, 28.56700777964554661 ) ) ;
#22021 = CARTESIAN_POINT ( 'NONE',  ( -30.02300923189239512, 56.25781249999997868, 2.654126918244515359E-13 ) ) ;
#22022 = CARTESIAN_POINT ( 'NONE',  ( 10.04305231718578817, 13.90000000546237580, -30.90933677959249337 ) ) ;
#22023 = CARTESIAN_POINT ( 'NONE',  ( 24.50000000000000000, 15.64999999453761248, 7.960532557706212486 ) ) ;
#22024 = CARTESIAN_POINT ( 'NONE',  ( -7.236395654485757944, 17.72499999726881370, -22.27133577429736988 ) ) ;
#22025 = CARTESIAN_POINT ( 'NONE',  ( -26.29305231718579350, 59.79999999999999005, -19.10302069950537884 ) ) ;
#22026 = CARTESIAN_POINT ( 'NONE',  ( 27.16883889988623935, 22.57500000273118701, -19.73931689729374384 ) ) ;
#22027 = DIRECTION ( 'NONE',  ( -0.000000000000000000, -1.000000000000000000, -0.000000000000000000 ) ) ;
#22028 = CARTESIAN_POINT ( 'NONE',  ( -14.97647472619899389, 67.99701416574269786, 26.02091320914878025 ) ) ;
#22029 = CARTESIAN_POINT ( 'NONE',  ( -8.601468415847518756, 76.57500000273115859, -11.83890561707634781 ) ) ;
#22030 = CARTESIAN_POINT ( 'NONE',  ( 5.147494310547426899, 65.44874571845315359, -32.50000000000000000 ) ) ;
#22031 = CARTESIAN_POINT ( 'NONE',  ( 10.04305231718579705, 14.60000000000000142, 30.90933677959248982 ) ) ;
#22032 = CARTESIAN_POINT ( 'NONE',  ( -26.29305231718578995, 10.20000000000000107, 19.10302069950538595 ) ) ;
#22033 = ORIENTED_EDGE ( 'NONE', *, *, #20351, .T. ) ;
#22034 = CARTESIAN_POINT ( 'NONE',  ( -7.236395654485757944, 9.724999997268806595, -22.27133577429736988 ) ) ;
#22035 = CARTESIAN_POINT ( 'NONE',  ( -11.25946833292375793, 74.67500000273119554, -8.180482586598733619 ) ) ;
#22036 = CARTESIAN_POINT ( 'NONE',  ( -26.07999730980477437, 42.36458333333332860, 6.988114217768305103 ) ) ;
#22037 = CARTESIAN_POINT ( 'NONE',  ( 33.58253175000000823, 20.02500000273118275, 10.91162601494192863 ) ) ;
#22038 = CARTESIAN_POINT ( 'NONE',  ( 27.16883889988623935, 68.32500000273118701, -19.73931689729374384 ) ) ;
#22039 = CARTESIAN_POINT ( 'NONE',  ( -33.58253175000000113, 31.47500000273117493, 10.91162601494193929 ) ) ;
#22040 = CARTESIAN_POINT ( 'NONE',  ( -2.162160676586881955E-15, 14.87500000273120193, -35.31076352940723240 ) ) ;
#22041 = CARTESIAN_POINT ( 'NONE',  ( 10.37757302488624767, 5.975000002731184701, 31.93888565452638417 ) ) ;
#22042 = CARTESIAN_POINT ( 'NONE',  ( -26.02091320914849959, 12.72173583425731458, 14.97647472619947528 ) ) ;
#22043 = CARTESIAN_POINT ( 'NONE',  ( -20.50609665441004736, 53.25000000000000000, -20.50609665440969565 ) ) ;
#22044 = CARTESIAN_POINT ( 'NONE',  ( 24.50000000000000000, 16.09999999999998721, -7.960532557706203605 ) ) ;
#22045 = CARTESIAN_POINT ( 'NONE',  ( -4.300734207923755825, 79.77500000273118985, 13.23629886949340673 ) ) ;
#22046 = CARTESIAN_POINT ( 'NONE',  ( 6.277390505771533514E-15, 50.50000000000000000, 34.17252228774368916 ) ) ;
#22047 = CARTESIAN_POINT ( 'NONE',  ( 3.880418787951140036, 8.198745712990779921, -24.49999999999999645 ) ) ;
#22048 = CARTESIAN_POINT ( 'NONE',  ( -10.37757302488623701, 51.52500000273118985, 31.93888565452638417 ) ) ;
#22049 = CARTESIAN_POINT ( 'NONE',  ( -23.41746824999999887, 12.12499999726882116, -2.867812753649727150E-15 ) ) ;
#22050 = EDGE_CURVE ( 'NONE', #12770, #31338, #21071, .T. ) ;
#22051 = EDGE_LOOP ( 'NONE', ( #33221, #14668, #16372, #7188 ) ) ;
#22052 = CARTESIAN_POINT ( 'NONE',  ( 10.37757302488624767, 63.97500000273119269, 31.93888565452638417 ) ) ;
#22053 = CARTESIAN_POINT ( 'NONE',  ( 32.50000000000000000, 17.00000000000001421, -3.980102097228898626E-15 ) ) ;
#22054 = CARTESIAN_POINT ( 'NONE',  ( 23.41746825000000243, 4.524999997268823293, 7.608796670333735079 ) ) ;
#22055 = CARTESIAN_POINT ( 'NONE',  ( 26.06988505166735592, 21.74517333425730925, 7.025853678916393896 ) ) ;
#22056 = EDGE_CURVE ( 'NONE', #18611, #27962, #3954, .T. ) ;
#22057 = ORIENTED_EDGE ( 'NONE', *, *, #25091, .T. ) ;
#22058 = CARTESIAN_POINT ( 'NONE',  ( -10.37757302488624411, 36.72500000273119980, -31.93888565452638417 ) ) ;
#22059 = CARTESIAN_POINT ( 'NONE',  ( 24.50000000000000000, 6.100000000000011191, -7.960532557706203605 ) ) ;
#22060 = ORIENTED_EDGE ( 'NONE', *, *, #6408, .F. ) ;
#22061 = CARTESIAN_POINT ( 'NONE',  ( -2.584737979205441561E-13, 53.67968750000000000, -30.02300923189239512 ) ) ;
#22062 = CARTESIAN_POINT ( 'NONE',  ( 6.486482029760649416E-15, 59.87500000273117706, 35.31076352940723240 ) ) ;
#22063 = CARTESIAN_POINT ( 'NONE',  ( -15.14183272437242067, 2.700000000000001954, -20.84094480462497856 ) ) ;
#22064 = CARTESIAN_POINT ( 'NONE',  ( 33.58253175000000113, 72.22500000273119269, -10.91162601494193751 ) ) ;
#22065 = CARTESIAN_POINT ( 'NONE',  ( 26.00068869287340334, 26.75260416666666430, -15.01150461594642316 ) ) ;
#22066 = CARTESIAN_POINT ( 'NONE',  ( -15.14183272437242600, 7.300000000000001599, 20.84094480462497856 ) ) ;
#22067 = CARTESIAN_POINT ( 'NONE',  ( 10.37757302488624767, 3.975000002731182924, 31.93888565452638417 ) ) ;
#22068 = CARTESIAN_POINT ( 'NONE',  ( -10.37757302488623701, 15.52500000273118808, 31.93888565452638417 ) ) ;
#22069 = CARTESIAN_POINT ( 'NONE',  ( 13.91746825000000065, 73.77500000273120406, 4.522059556121115875 ) ) ;
#22070 = CARTESIAN_POINT ( 'NONE',  ( 20.47846945139867003, 42.35899333240935505, -20.53372385742107653 ) ) ;
#22071 = CARTESIAN_POINT ( 'NONE',  ( 12.13525491562421088, 78.80000000000001137, 8.816778784387095058 ) ) ;
#22072 = CARTESIAN_POINT ( 'NONE',  ( -30.02300923189239867, 56.25781249999999289, 2.654126918244514854E-13 ) ) ;
#22073 = CARTESIAN_POINT ( 'NONE',  ( -7.570916362186210335, 8.349999994537615322, -23.30088464923126779 ) ) ;
#22074 = CARTESIAN_POINT ( 'NONE',  ( -19.82091636218621389, 8.949999994537632730, 14.40073868116558842 ) ) ;
#22075 = CARTESIAN_POINT ( 'NONE',  ( 10.04305231718578817, 49.90000000546238113, -30.90933677959249337 ) ) ;
#22076 = CARTESIAN_POINT ( 'NONE',  ( 2.584737979205441561E-13, 17.58593749999999645, 27.95245687107222921 ) ) ;
#22077 = CARTESIAN_POINT ( 'NONE',  ( 20.75514604977248467, 34.42500000273117422, -28.56700777964554305 ) ) ;
#22078 = AXIS2_PLACEMENT_3D ( 'NONE', #18552, #20148, #30419 ) ;
#22079 = CARTESIAN_POINT ( 'NONE',  ( 4.300734207923757602, 74.27500000273118985, -13.23629886949340673 ) ) ;
#22080 = CARTESIAN_POINT ( 'NONE',  ( -33.58253175000000113, 49.47500000273118559, 10.91162601494193929 ) ) ;
#22081 = CARTESIAN_POINT ( 'NONE',  ( -33.58253175000000113, 25.27500000273119696, -10.91162601494193041 ) ) ;
#22082 = CARTESIAN_POINT ( 'NONE',  ( 8.195098264072058214, 16.99999999999998934, 22.42925254762998932 ) ) ;
#22083 = VECTOR ( 'NONE', #31104, 1000.000000000000000 ) ;
#22084 = CARTESIAN_POINT ( 'NONE',  ( -6.988114217767819270, 34.91666666666666430, 26.07999730980490583 ) ) ;
#22085 = CARTESIAN_POINT ( 'NONE',  ( 3.880418787951102289, 12.19874571299077637, -24.50000000000000711 ) ) ;
#22086 = CARTESIAN_POINT ( 'NONE',  ( -9.270509831248423538, 79.69999999999997442, -12.75976212528059861 ) ) ;
#22087 = CARTESIAN_POINT ( 'NONE',  ( 10.04305231718578817, 67.40000000000000568, -30.90933677959249337 ) ) ;
#22088 = CARTESIAN_POINT ( 'NONE',  ( 33.58253175000000823, 6.025000002731191628, 10.91162601494192863 ) ) ;
#22089 = CARTESIAN_POINT ( 'NONE',  ( -23.41746824999999887, 13.62499999726882116, -2.867812753649727150E-15 ) ) ;
#22090 = CARTESIAN_POINT ( 'NONE',  ( -20.47846945139866648, 26.89024333240934439, 20.53372385742108008 ) ) ;
#22091 = CARTESIAN_POINT ( 'NONE',  ( 7.570916362186213000, 12.39999999999999503, -23.30088464923126423 ) ) ;
#22092 = CARTESIAN_POINT ( 'NONE',  ( -6.950374756619247307, 30.04128499907601224, 26.09010956794245217 ) ) ;
#22093 = CARTESIAN_POINT ( 'NONE',  ( -2.165007332552593587E-13, 46.50000000000000711, 32.50000000000000000 ) ) ;
#22094 = CARTESIAN_POINT ( 'NONE',  ( -33.58253175000000113, 11.02500000273117919, -10.91162601494193041 ) ) ;
#22095 = CARTESIAN_POINT ( 'NONE',  ( 23.41746825000000243, 7.224999997268826135, -7.608796670333727974 ) ) ;
#22096 = CARTESIAN_POINT ( 'NONE',  ( 6.988114217767829928, 53.82291666666666430, -26.07999730980489872 ) ) ;
#22097 = EDGE_LOOP ( 'NONE', ( #30643, #5637, #33535, #15266 ) ) ;
#22098 = CARTESIAN_POINT ( 'NONE',  ( 33.58253175000000113, 58.22500000273116427, -10.91162601494193751 ) ) ;
#22099 = CARTESIAN_POINT ( 'NONE',  ( 33.58253175000000113, 30.47500000273117493, -10.91162601494193751 ) ) ;
#22100 = ORIENTED_EDGE ( 'NONE', *, *, #841, .T. ) ;
#22101 = CARTESIAN_POINT ( 'NONE',  ( 7.505752307973351023, 27.75520833333332860, 28.01184896238290278 ) ) ;
#22102 = CARTESIAN_POINT ( 'NONE',  ( 26.02091320914851025, 21.31548583425730925, -14.97647472619946463 ) ) ;
#22103 = CARTESIAN_POINT ( 'NONE',  ( -4.223320258572819786E-15, 15.24999999453762278, 24.50000000000000000 ) ) ;
#22104 = CARTESIAN_POINT ( 'NONE',  ( 15.14183272437242245, 16.04999999453762882, -20.84094480462497856 ) ) ;
#22105 = CARTESIAN_POINT ( 'NONE',  ( -7.236395654485757944, 3.224999997268801266, -22.27133577429736988 ) ) ;
#22106 = CARTESIAN_POINT ( 'NONE',  ( 6.486482029760649416E-15, 19.87500000273119483, 35.31076352940723240 ) ) ;
#22107 = CARTESIAN_POINT ( 'NONE',  ( -2.092463501923844636E-15, 32.00000000546236834, -34.17252228774368916 ) ) ;
#22108 = SHAPE_REPRESENTATION ( 'primary mounting nut', ( #1376 ), #16210 ) ;
#22109 = CARTESIAN_POINT ( 'NONE',  ( 32.50000000000000711, 70.90000000000000568, 10.55989012756945122 ) ) ;
#22110 = CARTESIAN_POINT ( 'NONE',  ( 20.08610463437158344, 33.20000000546238539, 27.64615127144129403 ) ) ;
#22111 = CARTESIAN_POINT ( 'NONE',  ( -32.50000000000000000, 1.250000002731177506, 0.000000000000000000 ) ) ;
#22112 = CARTESIAN_POINT ( 'NONE',  ( 20.47846945139902530, 56.40663166759065206, 20.53372385742071771 ) ) ;
#22113 = CARTESIAN_POINT ( 'NONE',  ( -10.37757302488623701, 33.77500000273120406, 31.93888565452638417 ) ) ;
#22114 = CARTESIAN_POINT ( 'NONE',  ( -33.58253175000000113, 55.12500000273119838, 0.000000000000000000 ) ) ;
#22115 = CARTESIAN_POINT ( 'NONE',  ( -2.584737979205442066E-13, 22.74218749999999645, -30.02300923189239867 ) ) ;
#22116 = CARTESIAN_POINT ( 'NONE',  ( -23.41746825000000243, 10.02499999726882507, -7.608796670333730638 ) ) ;
#22117 = CARTESIAN_POINT ( 'NONE',  ( -10.04305231718579172, 13.60000000000000142, -30.90933677959248982 ) ) ;
#22118 = CARTESIAN_POINT ( 'NONE',  ( -24.50000000000001066, 9.100000000000004974, 7.960532557706201828 ) ) ;
#22119 = EDGE_CURVE ( 'NONE', #15118, #13108, #12649, .T. ) ;
#22120 = CARTESIAN_POINT ( 'NONE',  ( -19.06425588902558133, 44.07774333240935505, 19.11951029504797006 ) ) ;
#22121 = CARTESIAN_POINT ( 'NONE',  ( 33.58253175000000823, 54.02500000273118275, 10.91162601494192863 ) ) ;
#22122 = CARTESIAN_POINT ( 'NONE',  ( -33.58253175000000113, 47.47500000273119269, 10.91162601494193929 ) ) ;
#22123 = CARTESIAN_POINT ( 'NONE',  ( 18.94512977948575738, 12.42499999726881477, 13.76444248337723408 ) ) ;
#22124 = CARTESIAN_POINT ( 'NONE',  ( 19.82091636218621034, 9.800000000000002487, 14.40073868116559730 ) ) ;
#22125 = CARTESIAN_POINT ( 'NONE',  ( -20.75514604977248823, 4.825000002731171023, -28.56700777964554305 ) ) ;
#22126 = CARTESIAN_POINT ( 'NONE',  ( -26.09010956794232428, 40.36496500092396644, 6.950374756619732253 ) ) ;
#22127 = CARTESIAN_POINT ( 'NONE',  ( 10.39950962648949684, 16.99999999999998579, -20.99551648793040926 ) ) ;
#22128 = CARTESIAN_POINT ( 'NONE',  ( 1.806199397676865774E-16, -24.47487373415291145, 0.000000000000000000 ) ) ;
#22129 = CARTESIAN_POINT ( 'NONE',  ( 6.486482029760649416E-15, 25.62500000273118772, 35.31076352940723240 ) ) ;
#22130 = CARTESIAN_POINT ( 'NONE',  ( 5.779280353836490358E-15, 20.49999999999999645, 32.49999999999999289 ) ) ;
#22131 = DIRECTION ( 'NONE',  ( 1.000000000000000000, 0.000000000000000000, 0.000000000000000000 ) ) ;
#22132 = VECTOR ( 'NONE', #31329, 1000.000000000000000 ) ;
#22133 = CARTESIAN_POINT ( 'NONE',  ( 0.000000000000000000, 82.00000000000001421, 0.000000000000000000 ) ) ;
#22134 = CARTESIAN_POINT ( 'NONE',  ( -15.04653450569338524, 58.83034749907602645, -25.98046417659831775 ) ) ;
#22135 = CARTESIAN_POINT ( 'NONE',  ( -10.04305231718578462, 50.90000000546239534, 30.90933677959249337 ) ) ;
#22136 = SURFACE_SIDE_STYLE ('',( #11652 ) ) ;
#22137 = CARTESIAN_POINT ( 'NONE',  ( -6.988114217768288228, 26.03645833333333215, -26.07999730980477437 ) ) ;
#22138 = CARTESIAN_POINT ( 'NONE',  ( 27.16883889988623935, 78.32500000273120122, -19.73931689729374384 ) ) ;
#22139 = CARTESIAN_POINT ( 'NONE',  ( 7.505752307972854531, 26.32291666666666075, -28.01184896238303423 ) ) ;
#22140 = FACE_OUTER_BOUND ( 'NONE', #14434, .T. ) ;
#22141 = ORIENTED_EDGE ( 'NONE', *, *, #2535, .T. ) ;
#22142 = CARTESIAN_POINT ( 'NONE',  ( -26.02091320914849959, 50.53423583425731636, 14.97647472619947528 ) ) ;
#22143 = CARTESIAN_POINT ( 'NONE',  ( 20.08610463437158344, 13.20000000546237651, 27.64615127144129403 ) ) ;
#22144 = EDGE_CURVE ( 'NONE', #19445, #27878, #28008, .T. ) ;
#22145 = CARTESIAN_POINT ( 'NONE',  ( 30.02300923189239512, 61.41406250000000711, -2.619432448724977703E-13 ) ) ;
#22146 = CARTESIAN_POINT ( 'NONE',  ( -26.29305231718578995, 64.70000000546238539, 19.10302069950538595 ) ) ;
#22147 = CARTESIAN_POINT ( 'NONE',  ( 10.37757302488624056, 40.77500000273118275, -31.93888565452638417 ) ) ;
#22148 = CARTESIAN_POINT ( 'NONE',  ( -32.50000000000000000, 50.40000000546237402, -10.55989012756945478 ) ) ;
#22149 = CARTESIAN_POINT ( 'NONE',  ( -11.25946833292375793, 73.17500000273119554, -8.180482586598733619 ) ) ;
#22150 = CARTESIAN_POINT ( 'NONE',  ( 27.16883889988623935, 30.32500000273119412, -19.73931689729374384 ) ) ;
#22151 = CARTESIAN_POINT ( 'NONE',  ( 15.14183272437242422, 12.29999999999999183, -20.84094480462497856 ) ) ;
#22152 = TOROIDAL_SURFACE ( 'NONE', #28174, 11.45223628611452860, 2.000000000000014211 ) ;
#22153 = CARTESIAN_POINT ( 'NONE',  ( 20.75514604977248467, 56.67500000273119554, -28.56700777964554305 ) ) ;
#22154 = EDGE_CURVE ( 'NONE', #29542, #1522, #13514, .T. ) ;
#22155 = CARTESIAN_POINT ( 'NONE',  ( 32.50000000000000711, 34.89999999999999858, 10.55989012756945122 ) ) ;
#22156 = CARTESIAN_POINT ( 'NONE',  ( -26.29305231718579350, 33.79999999999999716, -19.10302069950537884 ) ) ;
#22157 = CARTESIAN_POINT ( 'NONE',  ( 18.94512977948575738, 14.42499999726881654, 13.76444248337723408 ) ) ;
#22158 = CARTESIAN_POINT ( 'NONE',  ( 33.58253175000000113, 4.475000002731183812, -10.91162601494193751 ) ) ;
#22159 = CARTESIAN_POINT ( 'NONE',  ( 1.555960095263670572E-15, 14.50000000000000178, -24.50000000000000000 ) ) ;
#22160 = CARTESIAN_POINT ( 'NONE',  ( 11.25946833292375793, 76.57500000273120122, -8.180482586598735395 ) ) ;
#22161 = CARTESIAN_POINT ( 'NONE',  ( -20.75514604977248112, 69.67500000273119554, 28.56700777964554661 ) ) ;
#22162 = CARTESIAN_POINT ( 'NONE',  ( -3.880418787951127602, 4.551254281546843750, -24.50000000000000000 ) ) ;
#22163 = ADVANCED_FACE ( 'NONE', ( #16095 ), #24310, .T. ) ;
#22164 = ORIENTED_EDGE ( 'NONE', *, *, #11443, .T. ) ;
#22165 = CARTESIAN_POINT ( 'NONE',  ( 19.82091636218621034, 5.549999994537619052, 14.40073868116559730 ) ) ;
#22166 = CARTESIAN_POINT ( 'NONE',  ( -6.950374756619716266, 10.28684000092397532, -26.09010956794232428 ) ) ;
#22167 = CARTESIAN_POINT ( 'NONE',  ( 0.000000000000000000, 80.00000000000001421, -32.50000000000000000 ) ) ;
#22168 = CARTESIAN_POINT ( 'NONE',  ( -27.16883889988623935, 47.32500000273119412, 19.73931689729374739 ) ) ;
#22169 = CARTESIAN_POINT ( 'NONE',  ( -33.58253175000000113, 7.375000002731183280, 0.000000000000000000 ) ) ;
#22170 = CARTESIAN_POINT ( 'NONE',  ( 20.75514604977249178, 60.07500000273120122, 28.56700777964553950 ) ) ;
#22171 = CARTESIAN_POINT ( 'NONE',  ( -6.988114217768288228, 46.66145833333332860, -26.07999730980477437 ) ) ;
#22172 = CARTESIAN_POINT ( 'NONE',  ( -14.97647472619946285, 41.08111083425730214, -26.02091320914851025 ) ) ;
#22173 = CARTESIAN_POINT ( 'NONE',  ( 28.00173670424535644, 28.89545166574268009, -7.543491769121920321 ) ) ;
#22174 = CARTESIAN_POINT ( 'NONE',  ( -10.04305231718578462, 68.90000000546238823, 30.90933677959249337 ) ) ;
#22175 = CARTESIAN_POINT ( 'NONE',  ( -11.25946833292375793, 77.07500000273121543, 8.180482586598737171 ) ) ;
#22176 = CARTESIAN_POINT ( 'NONE',  ( -6.950374756619247307, 54.10378499907602645, 26.09010956794245217 ) ) ;
#22177 = CARTESIAN_POINT ( 'NONE',  ( 5.779280353836490358E-15, 54.49999999999999289, 32.49999999999999289 ) ) ;
#22178 = CARTESIAN_POINT ( 'NONE',  ( 1.093617666956751375E-13, 66.00000000546238255, -32.50000000000000711 ) ) ;
#22179 = ORIENTED_EDGE ( 'NONE', *, *, #5047, .F. ) ;
#22180 = CARTESIAN_POINT ( 'NONE',  ( 10.37757302488624056, 42.77500000273119696, -31.93888565452638417 ) ) ;
#22181 = CARTESIAN_POINT ( 'NONE',  ( -10.04305231718579172, 75.59999999999999432, -30.90933677959248982 ) ) ;
#22182 = CARTESIAN_POINT ( 'NONE',  ( -26.29305231718578995, 32.70000000546237118, 19.10302069950538595 ) ) ;
#22183 = ORIENTED_EDGE ( 'NONE', *, *, #30303, .F. ) ;
#22184 = CARTESIAN_POINT ( 'NONE',  ( -2.584737979205441561E-13, 33.05468750000000000, -30.02300923189239512 ) ) ;
#22185 = VERTEX_POINT ( 'NONE', #1407 ) ;
#22186 = ORIENTED_EDGE ( 'NONE', *, *, #16781, .T. ) ;
#22187 = CARTESIAN_POINT ( 'NONE',  ( -26.29305231718578995, 56.20000000000000284, 19.10302069950538595 ) ) ;
#22188 = CARTESIAN_POINT ( 'NONE',  ( 27.16883889988624290, 49.92500000273120264, 19.73931689729373673 ) ) ;
#22189 = CARTESIAN_POINT ( 'NONE',  ( 20.50609665441005092, 54.96875000000000000, 20.50609665440969209 ) ) ;
#22190 = CARTESIAN_POINT ( 'NONE',  ( -26.29305231718578995, 14.70000000546237118, 19.10302069950538595 ) ) ;
#22191 = CYLINDRICAL_SURFACE ( 'NONE', #17417, 32.50000000000000000 ) ;
#22192 = CARTESIAN_POINT ( 'NONE',  ( -14.47279130897152299, 18.42499999726882010, 19.92008829642072243 ) ) ;
#22193 = VECTOR ( 'NONE', #16117, 1000.000000000000114 ) ;
#22194 = CARTESIAN_POINT ( 'NONE',  ( 32.50000000000000711, 52.89999999999999147, 10.55989012756945122 ) ) ;
#22195 = CARTESIAN_POINT ( 'NONE',  ( 6.486482029760649416E-15, 25.87500000273117351, 35.31076352940723240 ) ) ;
#22196 = CARTESIAN_POINT ( 'NONE',  ( 26.09010956794244507, 15.43190999907601935, 6.950374756619249084 ) ) ;
#22197 = CARTESIAN_POINT ( 'NONE',  ( -13.91746824999999887, 74.87500000273116996, 0.000000000000000000 ) ) ;
#22198 = CARTESIAN_POINT ( 'NONE',  ( -32.50000000000000000, 56.00000000000000711, 0.000000000000000000 ) ) ;
#22199 = CARTESIAN_POINT ( 'NONE',  ( 32.50000000000000000, 15.09999999999998899, -10.55989012756945833 ) ) ;
#22200 = CARTESIAN_POINT ( 'NONE',  ( -32.50000000000000000, 5.999999999999991118, 0.000000000000000000 ) ) ;
#22201 = VERTEX_POINT ( 'NONE', #16426 ) ;
#22202 = CARTESIAN_POINT ( 'NONE',  ( -18.94512977948575738, 7.924999997268811214, -13.76444248337723231 ) ) ;
#22203 = CARTESIAN_POINT ( 'NONE',  ( 0.000000000000000000, 80.00000000000001421, 0.000000000000000000 ) ) ;
#22204 = CARTESIAN_POINT ( 'NONE',  ( 13.97622843553633665, 37.92447916666666430, 24.20753774853730889 ) ) ;
#22205 = CARTESIAN_POINT ( 'NONE',  ( 20.75514604977249178, 63.82500000273119412, 28.56700777964553950 ) ) ;
#22206 = CARTESIAN_POINT ( 'NONE',  ( 10.37757302488624056, 28.77500000273118630, -31.93888565452638417 ) ) ;
#22207 = CARTESIAN_POINT ( 'NONE',  ( -10.37757302488623701, 13.77500000273117209, 31.93888565452638417 ) ) ;
#22208 = CARTESIAN_POINT ( 'NONE',  ( 33.58253175000000113, 8.475000002731173154, -10.91162601494193574 ) ) ;
#22209 = CARTESIAN_POINT ( 'NONE',  ( -7.468012846824771955, 10.28684000092397532, -28.02196122052045624 ) ) ;
#22210 = CARTESIAN_POINT ( 'NONE',  ( 15.01150461594596308, 50.52864583333333570, -26.00068869287367335 ) ) ;
#22211 = CARTESIAN_POINT ( 'NONE',  ( 3.880418787951153803, 5.551254281546845526, 24.49999999999999645 ) ) ;
#22212 = CARTESIAN_POINT ( 'NONE',  ( 4.300734207923761154, 79.97500000273119269, 13.23629886949340495 ) ) ;
#22213 = CARTESIAN_POINT ( 'NONE',  ( 32.50000000000000000, 49.09999999999999432, -10.55989012756945833 ) ) ;
#22214 = SURFACE_STYLE_FILL_AREA ( #1253 ) ;
#22215 = CARTESIAN_POINT ( 'NONE',  ( -10.37757302488624411, 50.72500000273119980, -31.93888565452638417 ) ) ;
#22216 = CARTESIAN_POINT ( 'NONE',  ( 18.94512977948576093, 4.824999997268819563, -13.76444248337722875 ) ) ;
#22217 = VERTEX_POINT ( 'NONE', #16259 ) ;
#22218 = CARTESIAN_POINT ( 'NONE',  ( 33.58253175000000823, 58.27500000273116854, 10.91162601494192863 ) ) ;
#22219 = CARTESIAN_POINT ( 'NONE',  ( 5.147494310547426899, 43.44874571845313938, -32.50000000000000000 ) ) ;
#22220 = CARTESIAN_POINT ( 'NONE',  ( 7.236395654485755280, 14.22499999726881192, 22.27133577429736988 ) ) ;
#22221 = CARTESIAN_POINT ( 'NONE',  ( 24.18731323226247554, 35.63840250092398065, 14.01125832528285997 ) ) ;
#22222 = ORIENTED_EDGE ( 'NONE', *, *, #28799, .T. ) ;
#22223 = CARTESIAN_POINT ( 'NONE',  ( -20.75514604977248823, 30.82500000273119767, -28.56700777964554305 ) ) ;
#22224 = CARTESIAN_POINT ( 'NONE',  ( -5.147494310547430452, 34.05125428700920764, -32.49999999999999289 ) ) ;
#22225 = ORIENTED_EDGE ( 'NONE', *, *, #18697, .T. ) ;
#22226 = CARTESIAN_POINT ( 'NONE',  ( -30.02300923189239512, 49.38281249999997868, 2.654126918244515359E-13 ) ) ;
#22227 = CARTESIAN_POINT ( 'NONE',  ( 10.37757302488624767, 59.97500000273120691, 31.93888565452638417 ) ) ;
#22228 = TOROIDAL_SURFACE ( 'NONE', #31553, 12.11607355459420177, 2.000000000000000000 ) ;
#22229 = CARTESIAN_POINT ( 'NONE',  ( -26.29305231718578995, 36.70000000546236407, 19.10302069950538595 ) ) ;
#22230 = CARTESIAN_POINT ( 'NONE',  ( 27.16883889988624290, 71.92500000273119554, 19.73931689729373673 ) ) ;
#22231 = VECTOR ( 'NONE', #759, 1000.000000000000000 ) ;
#22232 = CARTESIAN_POINT ( 'NONE',  ( -15.01150461594642138, 32.76822916666666430, -26.00068869287340334 ) ) ;
#22233 = CARTESIAN_POINT ( 'NONE',  ( 15.14183272437241889, 7.699999999999988631, 20.84094480462498211 ) ) ;
#22234 = CARTESIAN_POINT ( 'NONE',  ( 27.16883889988624290, 4.175000002731188431, 19.73931689729373673 ) ) ;
#22235 = CARTESIAN_POINT ( 'NONE',  ( 33.58253175000000113, 14.22500000273119625, -10.91162601494193751 ) ) ;
#22236 = CARTESIAN_POINT ( 'NONE',  ( 4.300734207923761154, 73.47500000273119269, 13.23629886949340495 ) ) ;
#22237 = CARTESIAN_POINT ( 'NONE',  ( -28.02196122052058413, 44.65065999907601935, -7.468012846824272799 ) ) ;
#22238 = CARTESIAN_POINT ( 'NONE',  ( 13.91746824999999887, 72.37500000273119838, -1.704398294459741270E-15 ) ) ;
#22239 = CARTESIAN_POINT ( 'NONE',  ( 20.50609665440969565, 54.10937499999999289, -20.50609665441004736 ) ) ;
#22240 = CARTESIAN_POINT ( 'NONE',  ( 32.50000000000000000, 53.50000000546238965, -3.980102097228898626E-15 ) ) ;
#22241 = CARTESIAN_POINT ( 'NONE',  ( 15.14183272437242245, 6.049999994537625270, -20.84094480462497856 ) ) ;
#22242 = CARTESIAN_POINT ( 'NONE',  ( -12.13525491562421088, 80.05000000546236549, -8.816778784387096835 ) ) ;
#22243 = CARTESIAN_POINT ( 'NONE',  ( 13.97622843553589966, 12.71614583333333037, -24.20753774853756113 ) ) ;
#22244 = EDGE_CURVE ( 'NONE', #5385, #14916, #25337, .T. ) ;
#22245 = CARTESIAN_POINT ( 'NONE',  ( 33.58253175000000113, 36.22500000273119980, -10.91162601494193751 ) ) ;
#22246 = CARTESIAN_POINT ( 'NONE',  ( -13.91746824999999532, 74.97500000273117848, 4.522059556121122093 ) ) ;
#22247 = CARTESIAN_POINT ( 'NONE',  ( 20.75514604977249178, 48.07500000273120122, 28.56700777964553950 ) ) ;
#22248 = CARTESIAN_POINT ( 'NONE',  ( 10.37757302488624767, 29.97500000273117848, 31.93888565452638417 ) ) ;
#22249 = CARTESIAN_POINT ( 'NONE',  ( 5.779280353836490358E-15, 8.500000000000000000, 32.49999999999999289 ) ) ;
#22250 = EDGE_CURVE ( 'NONE', #15950, #25816, #5555, .T. ) ;
#22251 = CARTESIAN_POINT ( 'NONE',  ( -24.20753774853756823, 35.91927083333332860, -13.97622843553588723 ) ) ;
#22252 = DIRECTION ( 'NONE',  ( 0.000000000000000000, 0.000000000000000000, -1.000000000000000000 ) ) ;
#22253 = CARTESIAN_POINT ( 'NONE',  ( 15.00000000000000000, 81.09999999999999432, -4.873795443493596835 ) ) ;
#22254 = CARTESIAN_POINT ( 'NONE',  ( -10.04305231718578462, 64.40000000000000568, 30.90933677959249337 ) ) ;
#22255 = CARTESIAN_POINT ( 'NONE',  ( -4.523095164977117273E-15, 12.12499999726881583, 24.62258325217400312 ) ) ;
#22256 = CARTESIAN_POINT ( 'NONE',  ( 20.53372385742108008, 22.59336833240935505, 20.47846945139866648 ) ) ;
#22257 = CARTESIAN_POINT ( 'NONE',  ( -23.41746824999999887, 4.124999997268813168, -2.867812753649727150E-15 ) ) ;
#22258 = CARTESIAN_POINT ( 'NONE',  ( 0.04044903255044120238, 40.21055583240935505, 27.95245687107223276 ) ) ;
#22259 = SURFACE_STYLE_USAGE ( .BOTH. , #17276 ) ;
#22260 = CARTESIAN_POINT ( 'NONE',  ( -33.58253175000000113, 13.02500000273117564, -10.91162601494193041 ) ) ;
#22261 = CARTESIAN_POINT ( 'NONE',  ( -14.47279130897151589, 3.824999997268816454, -19.92008829642072598 ) ) ;
#22262 = CARTESIAN_POINT ( 'NONE',  ( 2.584737979205441561E-13, 58.83593750000000000, 27.95245687107222921 ) ) ;
#22263 = ORIENTED_EDGE ( 'NONE', *, *, #3157, .T. ) ;
#22264 = CARTESIAN_POINT ( 'NONE',  ( -10.37757302488623701, 53.52500000273118275, 31.93888565452638417 ) ) ;
#22265 = CARTESIAN_POINT ( 'NONE',  ( -2.162160676586881955E-15, 28.87500000273119838, -35.31076352940723240 ) ) ;
#22266 = ORIENTED_EDGE ( 'NONE', *, *, #17135, .F. ) ;
#22267 = CARTESIAN_POINT ( 'NONE',  ( -28.01184896238304134, 25.46354166666666430, -7.505752307972844761 ) ) ;
#22268 = CARTESIAN_POINT ( 'NONE',  ( -7.543491769121417612, 26.04204833425729859, 28.00173670424549499 ) ) ;
#22269 = CARTESIAN_POINT ( 'NONE',  ( -33.58253175000000113, 1.125000002731191273, 0.000000000000000000 ) ) ;
#22270 = CARTESIAN_POINT ( 'NONE',  ( -4.732186688966233175E-15, 17.24999999453762101, 25.76082449383753925 ) ) ;
#22271 = CARTESIAN_POINT ( 'NONE',  ( 7.236395654485755280, 6.224999997268803931, 22.27133577429736988 ) ) ;
#22272 = CARTESIAN_POINT ( 'NONE',  ( -20.75514604977248823, 23.07500000273117635, -28.56700777964554305 ) ) ;
#22273 = CARTESIAN_POINT ( 'NONE',  ( 20.08610463437158344, 25.20000000546237473, 27.64615127144129403 ) ) ;
#22274 = CARTESIAN_POINT ( 'NONE',  ( 32.50000000000000000, 75.00000000000001421, -3.980102097228898626E-15 ) ) ;
#22275 = DIRECTION ( 'NONE',  ( 0.000000000000000000, 0.000000000000000000, 1.000000000000000000 ) ) ;
#22276 = CARTESIAN_POINT ( 'NONE',  ( -9.225643108219712119, 73.99999999999998579, 11.22019004876342763 ) ) ;
#22277 = CARTESIAN_POINT ( 'NONE',  ( -7.468012846824771955, 51.53684000092397355, -28.02196122052045624 ) ) ;
#22278 = CARTESIAN_POINT ( 'NONE',  ( -33.58253175000000113, 33.37500000273119127, 0.000000000000000000 ) ) ;
#22279 = CARTESIAN_POINT ( 'NONE',  ( 20.75514604977249178, 57.82500000273119412, 28.56700777964553950 ) ) ;
#22280 = CARTESIAN_POINT ( 'NONE',  ( -15.01150461594642316, 29.33072916666665719, -26.00068869287341045 ) ) ;
#22281 =( NAMED_UNIT ( * ) PLANE_ANGLE_UNIT ( ) SI_UNIT ( $, .RADIAN. ) );
#22282 = CARTESIAN_POINT ( 'NONE',  ( 18.94512977948575738, 8.924999997268812990, 13.76444248337723408 ) ) ;
#22283 = CARTESIAN_POINT ( 'NONE',  ( 20.08610463437157279, 15.29999999999998472, -27.64615127144129758 ) ) ;
#22284 = CARTESIAN_POINT ( 'NONE',  ( 7.570916362186213000, 12.39999999999999503, -23.30088464923126423 ) ) ;
#22285 = CARTESIAN_POINT ( 'NONE',  ( -19.11951029504797006, 41.49961833240934794, -19.06425588902558133 ) ) ;
#22286 = CARTESIAN_POINT ( 'NONE',  ( 20.75514604977248467, 58.42500000273119554, -28.56700777964554305 ) ) ;
#22287 = CARTESIAN_POINT ( 'NONE',  ( 33.58253175000000823, 50.27500000273118985, 10.91162601494192685 ) ) ;
#22288 = CARTESIAN_POINT ( 'NONE',  ( 23.41746824999999887, 8.724999997268806595, -7.608796670333727974 ) ) ;
#22289 = CARTESIAN_POINT ( 'NONE',  ( 3.980102097228898626E-15, 80.00000000000001421, 32.50000000000000000 ) ) ;
#22290 = CARTESIAN_POINT ( 'NONE',  ( 27.16883889988623935, 2.325000002731170134, -19.73931689729374384 ) ) ;
#22291 = CARTESIAN_POINT ( 'NONE',  ( -13.94119854578936923, 47.95611083425732346, -24.22776226481241224 ) ) ;
#22292 = CARTESIAN_POINT ( 'NONE',  ( -21.91832052488144456, 17.00000000000000355, -10.39831318017644080 ) ) ;
#22293 = CARTESIAN_POINT ( 'NONE',  ( -1.778240108872766143E-15, 41.49999999999999289, -32.49999999999999289 ) ) ;
#22294 = CARTESIAN_POINT ( 'NONE',  ( -10.37757302488623701, 19.52500000273120406, 31.93888565452638417 ) ) ;
#22295 = DIRECTION ( 'NONE',  ( -0.000000000000000000, -1.000000000000000000, -0.000000000000000000 ) ) ;
#22296 = CARTESIAN_POINT ( 'NONE',  ( -4.635254915624211769, 77.85000000546237686, -14.26584774442730286 ) ) ;
#22297 = CARTESIAN_POINT ( 'NONE',  ( -10.72870458603807720, -72.44024934668307480, 0.000000000000000000 ) ) ;
#22298 = CARTESIAN_POINT ( 'NONE',  ( -15.04653450569338524, 65.70534749907602645, -25.98046417659831775 ) ) ;
#22299 = CARTESIAN_POINT ( 'NONE',  ( -20.08610463437156923, 48.80000000546235128, 27.64615127144130113 ) ) ;
#22300 = CARTESIAN_POINT ( 'NONE',  ( 26.29305231718579350, 34.79999999999999716, 19.10302069950537529 ) ) ;
#22301 = CARTESIAN_POINT ( 'NONE',  ( 20.75514604977248467, 30.42500000273117777, -28.56700777964554305 ) ) ;
#22302 = CARTESIAN_POINT ( 'NONE',  ( -6.988114217767819270, 24.60416666666666430, 26.07999730980490583 ) ) ;
#22303 = CARTESIAN_POINT ( 'NONE',  ( -27.16883889988624290, 76.92500000273120975, -19.73931689729374028 ) ) ;
#22304 = AXIS2_PLACEMENT_3D ( 'NONE', #107, #26551, #31855 ) ;
#22305 = CARTESIAN_POINT ( 'NONE',  ( -30.02300923189239512, 39.07031249999997868, 2.654126918244515359E-13 ) ) ;
#22306 = FACE_OUTER_BOUND ( 'NONE', #5431, .T. ) ;
#22307 = VERTEX_POINT ( 'NONE', #21572 ) ;
#22308 = CARTESIAN_POINT ( 'NONE',  ( -7.468012846824771955, 48.09934000092398065, -28.02196122052045624 ) ) ;
#22309 = CARTESIAN_POINT ( 'NONE',  ( 32.50000000000000711, 13.40000000546237047, 10.55989012756945122 ) ) ;
#22310 = VECTOR ( 'NONE', #16527, 1000.000000000000000 ) ;
#22311 = CARTESIAN_POINT ( 'NONE',  ( -20.50609665440969209, 62.70312500000000000, 20.50609665441005092 ) ) ;
#22312 = FACE_OUTER_BOUND ( 'NONE', #4829, .T. ) ;
#22313 = CARTESIAN_POINT ( 'NONE',  ( 33.58253175000000823, 44.27500000273120406, 10.91162601494192863 ) ) ;
#22314 = CARTESIAN_POINT ( 'NONE',  ( -10.04305231718579172, 50.10000000546238397, -30.90933677959248982 ) ) ;
#22315 = CARTESIAN_POINT ( 'NONE',  ( -4.300734207923759378, 74.97500000273122112, -13.23629886949340495 ) ) ;
#22316 = CARTESIAN_POINT ( 'NONE',  ( 33.58253175000000113, 32.22500000273117848, -10.91162601494193751 ) ) ;
#22317 = PLANE ( 'NONE',  #600 ) ;
#22318 = CARTESIAN_POINT ( 'NONE',  ( 33.58253175000000823, 58.27500000273116854, 10.91162601494192863 ) ) ;
#22319 = SHAPE_REPRESENTATION_RELATIONSHIP ( 'NONE' , 'NONE' ,  #22108, #11923 ) ;
#22320 = CARTESIAN_POINT ( 'NONE',  ( 10.04305231718578817, 33.39999999999999858, -30.90933677959249337 ) ) ;
#22321 = CARTESIAN_POINT ( 'NONE',  ( -20.08610463437157989, 31.69999999999998508, -27.64615127144129758 ) ) ;
#22322 = CARTESIAN_POINT ( 'NONE',  ( -7.236395654485757944, 9.224999997268806595, -22.27133577429736988 ) ) ;
#22323 = CARTESIAN_POINT ( 'NONE',  ( 27.16883889988623935, 74.32500000273117280, -19.73931689729374384 ) ) ;
#22324 = CARTESIAN_POINT ( 'NONE',  ( -11.45223628611452504, -57.99999999999999289, 0.000000000000000000 ) ) ;
#22325 = CARTESIAN_POINT ( 'NONE',  ( 4.300734207923757602, 78.77500000273118985, -13.23629886949340673 ) ) ;
#22326 = CARTESIAN_POINT ( 'NONE',  ( 6.486482029760648627E-15, 69.87500000273121259, 35.31076352940722529 ) ) ;
#22327 = CARTESIAN_POINT ( 'NONE',  ( 12.13525491562420910, 77.45000000546237118, -8.816778784387098611 ) ) ;
#22328 = CARTESIAN_POINT ( 'NONE',  ( 5.779280353836490358E-15, 41.00000000546237544, 32.49999999999999289 ) ) ;
#22329 = CARTESIAN_POINT ( 'NONE',  ( -7.570916362186215665, 3.149999994537633352, 23.30088464923126423 ) ) ;
#22330 = CARTESIAN_POINT ( 'NONE',  ( -7.025853678916393008, 15.72954833425730925, 26.06988505166735592 ) ) ;
#22331 = CARTESIAN_POINT ( 'NONE',  ( 0.000000000000000000, 11.99999999999999645, 0.000000000000000000 ) ) ;
#22332 = CARTESIAN_POINT ( 'NONE',  ( -27.16883889988624290, 46.92500000273118133, -19.73931689729374028 ) ) ;
#22333 = CARTESIAN_POINT ( 'NONE',  ( -33.58253175000000113, 7.275000002731196957, -10.91162601494193218 ) ) ;
#22334 = CARTESIAN_POINT ( 'NONE',  ( 33.58253175000000823, 54.27500000273118985, 10.91162601494192685 ) ) ;
#22335 = CARTESIAN_POINT ( 'NONE',  ( 19.09188309203661049, 47.23437499999999289, -19.09188309203694445 ) ) ;
#22336 = CARTESIAN_POINT ( 'NONE',  ( -26.02091320914849959, 36.78423583425730214, 14.97647472619947528 ) ) ;
#22337 = CARTESIAN_POINT ( 'NONE',  ( 20.53372385742108008, 26.03086833240935860, 20.47846945139866648 ) ) ;
#22338 = CARTESIAN_POINT ( 'NONE',  ( -2.092463501923844636E-15, 66.00000000546239676, -34.17252228774368916 ) ) ;
#22339 = CARTESIAN_POINT ( 'NONE',  ( 13.91746825000000065, 75.77500000273117564, 4.522059556121114987 ) ) ;
#22340 = CARTESIAN_POINT ( 'NONE',  ( -27.95245687107223986, 51.38243083240936215, 0.04044903255043252877 ) ) ;
#22341 = CARTESIAN_POINT ( 'NONE',  ( 2.205017735002230837E-13, 57.49999999999999289, -32.50000000000000000 ) ) ;
#22342 = VERTEX_POINT ( 'NONE', #6105 ) ;
#22343 = CARTESIAN_POINT ( 'NONE',  ( 10.37757302488624056, 40.77500000273119696, -31.93888565452638417 ) ) ;
#22344 = CARTESIAN_POINT ( 'NONE',  ( 7.236395654485760609, 3.524999997268824181, -22.27133577429736633 ) ) ;
#22345 = CARTESIAN_POINT ( 'NONE',  ( -26.29305231718578995, 30.70000000546237118, 19.10302069950538595 ) ) ;
#22346 = ORIENTED_EDGE ( 'NONE', *, *, #14925, .F. ) ;
#22347 = CARTESIAN_POINT ( 'NONE',  ( -26.00068869287368756, 35.91927083333332860, -15.01150461594595775 ) ) ;
#22348 = VERTEX_POINT ( 'NONE', #21405 ) ;
#22349 = CARTESIAN_POINT ( 'NONE',  ( -20.08610463437156923, 74.80000000546236549, 27.64615127144130113 ) ) ;
#22350 = CARTESIAN_POINT ( 'NONE',  ( 27.16883889988623935, 50.32500000273118701, -19.73931689729374384 ) ) ;
#22351 = CARTESIAN_POINT ( 'NONE',  ( 28.01184896238290278, 61.27083333333332860, -7.505752307973347470 ) ) ;
#22352 = CARTESIAN_POINT ( 'NONE',  ( 20.08610463437158344, 13.20000000546237651, 27.64615127144129403 ) ) ;
#22353 = CARTESIAN_POINT ( 'NONE',  ( -2.375766604868048137, 78.44874571845313938, 14.99999999999999822 ) ) ;
#22354 = CARTESIAN_POINT ( 'NONE',  ( -23.41746824999999887, 16.12499999726882294, -2.867812753649727150E-15 ) ) ;
#22355 = CARTESIAN_POINT ( 'NONE',  ( -20.08610463437157989, 51.70000000000000284, -27.64615127144129758 ) ) ;
#22356 = DIRECTION ( 'NONE',  ( 0.000000000000000000, 1.000000000000000000, 0.000000000000000000 ) ) ;
#22357 = CARTESIAN_POINT ( 'NONE',  ( 33.58253175000000113, 20.37500000273118062, -4.112674001490185761E-15 ) ) ;
#22358 = CARTESIAN_POINT ( 'NONE',  ( 5.147494310547434893, 5.051254287009220079, 32.49999999999999289 ) ) ;
#22359 = CARTESIAN_POINT ( 'NONE',  ( -13.94119854578892514, 19.87201416574269075, 24.22776226481266448 ) ) ;
#22360 = CARTESIAN_POINT ( 'NONE',  ( 8.601468415847516980, 72.17500000273118133, -11.83890561707634781 ) ) ;
#22361 = CARTESIAN_POINT ( 'NONE',  ( 9.270509831248421762, 75.55000000546237970, -12.75976212528059861 ) ) ;
#22362 = CARTESIAN_POINT ( 'NONE',  ( -26.29305231718579350, 28.30000000546237260, -19.10302069950537884 ) ) ;
#22363 = CARTESIAN_POINT ( 'NONE',  ( -20.75514604977248823, 79.07500000273121543, -28.56700777964554305 ) ) ;
#22364 = ORIENTED_EDGE ( 'NONE', *, *, #15625, .F. ) ;
#22365 = CARTESIAN_POINT ( 'NONE',  ( 18.94512977948575738, 8.924999997268812990, 13.76444248337723408 ) ) ;
#22366 = CARTESIAN_POINT ( 'NONE',  ( -11.54700538379251995, 96.00000000000002842, -19.99999999999999645 ) ) ;
#22367 = CARTESIAN_POINT ( 'NONE',  ( 26.07999730980490227, 40.93229166666666430, 6.988114217767821046 ) ) ;
#22368 = EDGE_CURVE ( 'NONE', #21926, #22878, #24797, .T. ) ;
#22369 = CARTESIAN_POINT ( 'NONE',  ( 20.75514604977248467, 66.42500000273120975, -28.56700777964554305 ) ) ;
#22370 = CARTESIAN_POINT ( 'NONE',  ( -20.75514604977248112, 21.67500000273119554, 28.56700777964554661 ) ) ;
#22371 = CARTESIAN_POINT ( 'NONE',  ( 10.37757302488624767, 15.97500000273120691, 31.93888565452638417 ) ) ;
#22372 = CARTESIAN_POINT ( 'NONE',  ( 27.16883889988623935, 8.575000002731202997, -19.73931689729374384 ) ) ;
#22373 = CARTESIAN_POINT ( 'NONE',  ( 7.543491769121427382, 14.01079833425730747, -28.00173670424548433 ) ) ;
#22374 = CARTESIAN_POINT ( 'NONE',  ( 28.01184896238304134, 58.11979166666665719, 7.505752307972846538 ) ) ;
#22375 = CARTESIAN_POINT ( 'NONE',  ( 8.601468415847520532, 76.07500000273118701, 11.83890561707634603 ) ) ;
#22376 = CARTESIAN_POINT ( 'NONE',  ( -26.29305231718578995, 46.20000000000000284, 19.10302069950538595 ) ) ;
#22377 = CARTESIAN_POINT ( 'NONE',  ( 32.50000000000000711, 62.89999999999998437, 10.55989012756945122 ) ) ;
#22378 = CARTESIAN_POINT ( 'NONE',  ( -20.75514604977248112, 49.42500000273118843, 28.56700777964554661 ) ) ;
#22379 = CARTESIAN_POINT ( 'NONE',  ( 7.236395654485755280, 4.224999997268802154, 22.27133577429736988 ) ) ;
#22380 = ORIENTED_EDGE ( 'NONE', *, *, #5286, .T. ) ;
#22381 = CARTESIAN_POINT ( 'NONE',  ( -2.162160676586881955E-15, 60.87500000273116996, -35.31076352940723240 ) ) ;
#22382 = CARTESIAN_POINT ( 'NONE',  ( 0.000000000000000000, 80.00000000000001421, 0.000000000000000000 ) ) ;
#22383 = CARTESIAN_POINT ( 'NONE',  ( -18.94512977948575738, 11.42499999726881477, -13.76444248337723231 ) ) ;
#22384 = CARTESIAN_POINT ( 'NONE',  ( 14.01125832528286352, 34.77902750092397355, -24.18731323226246843 ) ) ;
#22385 = ORIENTED_EDGE ( 'NONE', *, *, #14411, .F. ) ;
#22386 = CARTESIAN_POINT ( 'NONE',  ( -33.58253175000000113, 33.02500000273118275, -10.91162601494193218 ) ) ;
#22387 = CARTESIAN_POINT ( 'NONE',  ( -9.270509831248419985, 74.29999999999999716, 12.75976212528060039 ) ) ;
#22388 = ORIENTED_EDGE ( 'NONE', *, *, #16499, .F. ) ;
#22389 = CARTESIAN_POINT ( 'NONE',  ( 28.01184896238304134, 58.11979166666665719, 7.505752307972846538 ) ) ;
#22390 = CARTESIAN_POINT ( 'NONE',  ( 6.486482029760649416E-15, 57.87500000273117706, 35.31076352940723240 ) ) ;
#22391 = CARTESIAN_POINT ( 'NONE',  ( 2.445080149700053643E-15, 76.50000000000001421, 15.00000000000000000 ) ) ;
#22392 = CARTESIAN_POINT ( 'NONE',  ( -33.58253175000000113, 67.12500000273119838, 0.000000000000000000 ) ) ;
#22393 = CARTESIAN_POINT ( 'NONE',  ( 20.50609665440969565, 26.60937499999999645, -20.50609665441004736 ) ) ;
#22394 = CARTESIAN_POINT ( 'NONE',  ( -24.50000000000001066, 15.09999999999998899, 7.960532557706201828 ) ) ;
#22395 = CARTESIAN_POINT ( 'NONE',  ( -27.16883889988624290, 5.175000002731189319, -19.73931689729374028 ) ) ;
#22396 = CARTESIAN_POINT ( 'NONE',  ( -33.58253175000000113, 13.02500000273117564, -10.91162601494193218 ) ) ;
#22397 =( BOUNDED_CURVE ( )  B_SPLINE_CURVE ( 2, ( #23552, #5693, #2440, #20982, #18066, #29021, #16002, #26458, #31260, #16171, #23382, #29188, #7754 ),
 .UNSPECIFIED., .F., .T. ) 
 B_SPLINE_CURVE_WITH_KNOTS ( ( 3, 2, 2, 2, 2, 2, 3 ),
 ( 0.3500000000000000333, 0.3599999999999999867, 0.3800000000000000044, 0.4000000000000000222, 0.4199999999999999845, 0.4400000000000000022, 0.4500000000000000111 ),
 .UNSPECIFIED. ) 
 CURVE ( )  GEOMETRIC_REPRESENTATION_ITEM ( )  RATIONAL_B_SPLINE_CURVE ( ( 0.9755282581475768211, 0.9755282581475768211, 1.000000000000000000, 0.9510565162951535312, 1.000000000000000000, 0.9510565162951535312, 1.000000000000000000, 0.9510565162951535312, 1.000000000000000000, 0.9510565162951535312, 1.000000000000000000, 0.9755282581475768211, 0.9755282581475768211 ) ) 
 REPRESENTATION_ITEM ( '' )  );
#22398 = CARTESIAN_POINT ( 'NONE',  ( -11.25946833292375793, 72.67500000273119554, -8.180482586598733619 ) ) ;
#22399 = CARTESIAN_POINT ( 'NONE',  ( -15.04653450569338524, 41.64284749907602645, -25.98046417659831775 ) ) ;
#22400 = CARTESIAN_POINT ( 'NONE',  ( -15.00000000000000000, 82.00000000000001421, 0.000000000000000000 ) ) ;
#22401 = CARTESIAN_POINT ( 'NONE',  ( 20.50609665441005092, 54.96875000000000000, 20.50609665440969209 ) ) ;
#22402 = CARTESIAN_POINT ( 'NONE',  ( 24.50000000000000355, 7.849999994537626868, -7.960532557706203605 ) ) ;
#22403 = CARTESIAN_POINT ( 'NONE',  ( -15.00000000000000000, 78.35000000546239107, 4.873795443493597723 ) ) ;
#22404 = CARTESIAN_POINT ( 'NONE',  ( 19.09188309203694800, 13.71874999999999467, 19.09188309203660694 ) ) ;
#22405 = CARTESIAN_POINT ( 'NONE',  ( 27.16883889988623935, 36.32500000273120122, -19.73931689729374384 ) ) ;
#22406 = CARTESIAN_POINT ( 'NONE',  ( 11.25946833292375793, 78.07500000273121543, -8.180482586598735395 ) ) ;
#22407 = CARTESIAN_POINT ( 'NONE',  ( 33.58253175000000823, 44.27500000273120406, 10.91162601494192863 ) ) ;
#22408 = CARTESIAN_POINT ( 'NONE',  ( 33.58253175000000823, 28.27500000273118985, 10.91162601494192685 ) ) ;
#22409 = CARTESIAN_POINT ( 'NONE',  ( -26.29305231718578995, 12.70000000546239782, 19.10302069950538595 ) ) ;
#22410 = CARTESIAN_POINT ( 'NONE',  ( 0.000000000000000000, 16.99999999999998579, 0.000000000000000000 ) ) ;
#22411 = CARTESIAN_POINT ( 'NONE',  ( 12.11607355459420887, -70.99969134886156041, 0.000000000000000000 ) ) ;
#22412 = CARTESIAN_POINT ( 'NONE',  ( 20.08610463437158344, 68.70000000000001705, 27.64615127144129403 ) ) ;
#22413 = CARTESIAN_POINT ( 'NONE',  ( -7.236395654485763274, 10.02499999726880198, 22.27133577429736633 ) ) ;
#22414 = CARTESIAN_POINT ( 'NONE',  ( 0.04044903255045854962, 23.02305583240935860, 30.02300923189239867 ) ) ;
#22415 = CARTESIAN_POINT ( 'NONE',  ( 7.236395654485755280, 4.724999997268803043, 22.27133577429736988 ) ) ;
#22416 = CARTESIAN_POINT ( 'NONE',  ( -6.950374756619247307, 36.91628499907601224, 26.09010956794245217 ) ) ;
#22417 = CARTESIAN_POINT ( 'NONE',  ( 20.75514604977248467, 14.42500000273118843, -28.56700777964554305 ) ) ;
#22418 = CARTESIAN_POINT ( 'NONE',  ( 7.236395654485755280, 14.72499999726881192, 22.27133577429736988 ) ) ;
#22419 = CARTESIAN_POINT ( 'NONE',  ( 24.20753774853756113, 65.13802083333334281, 13.97622843553589789 ) ) ;
#22420 = EDGE_LOOP ( 'NONE', ( #2848, #9142, #17846, #18924 ) ) ;
#22421 = CARTESIAN_POINT ( 'NONE',  ( -20.75514604977248823, 46.82500000273117990, -28.56700777964554305 ) ) ;
#22422 = CARTESIAN_POINT ( 'NONE',  ( -2.162160676586881955E-15, 24.87500000273117351, -35.31076352940723240 ) ) ;
#22423 = EDGE_CURVE ( 'NONE', #28216, #771, #31850, .T. ) ;
#22424 = EDGE_LOOP ( 'NONE', ( #6263, #19893, #27916 ) ) ;
#22425 = CARTESIAN_POINT ( 'NONE',  ( 26.00068869287340334, 30.19010416666665719, -15.01150461594642316 ) ) ;
#22426 = CARTESIAN_POINT ( 'NONE',  ( -7.543491769121417612, 29.47954833425730570, 28.00173670424549499 ) ) ;
#22427 = FACE_OUTER_BOUND ( 'NONE', #11570, .T. ) ;
#22428 = CARTESIAN_POINT ( 'NONE',  ( -7.570916362186215665, 13.14999999453761426, 23.30088464923126423 ) ) ;
#22429 = EDGE_CURVE ( 'NONE', #19356, #10883, #8514, .T. ) ;
#22430 = CARTESIAN_POINT ( 'NONE',  ( 18.94512977948576093, 6.824999997268821339, -13.76444248337722875 ) ) ;
#22431 = CARTESIAN_POINT ( 'NONE',  ( -2.162160676586881955E-15, 24.87500000273117351, -35.31076352940723240 ) ) ;
#22432 = CARTESIAN_POINT ( 'NONE',  ( -10.04305231718578462, 26.90000000546238823, 30.90933677959249337 ) ) ;
#22433 = CARTESIAN_POINT ( 'NONE',  ( -20.08610463437157989, 73.70000000000000284, -27.64615127144129758 ) ) ;
#22434 = FACE_OUTER_BOUND ( 'NONE', #10158, .T. ) ;
#22435 = CARTESIAN_POINT ( 'NONE',  ( -5.331399199010175671, 74.00000000000000000, 13.31861229302914928 ) ) ;
#22436 = CARTESIAN_POINT ( 'NONE',  ( -14.97647472619946285, 58.26861083425732346, -26.02091320914851025 ) ) ;
#22437 = CARTESIAN_POINT ( 'NONE',  ( 27.16883889988624290, 34.17500000273118843, 19.73931689729373673 ) ) ;
#22438 = CARTESIAN_POINT ( 'NONE',  ( -10.37757302488623701, 53.52500000273118275, 31.93888565452638417 ) ) ;
#22439 = CARTESIAN_POINT ( 'NONE',  ( -15.01150461594595775, 28.18489583333333215, 26.00068869287368756 ) ) ;
#22440 = DIRECTION ( 'NONE',  ( 1.000000000000000000, 0.000000000000000000, 0.000000000000000000 ) ) ;
#22441 = CARTESIAN_POINT ( 'NONE',  ( -7.236395654485757944, 9.724999997268806595, -22.27133577429736988 ) ) ;
#22442 = CARTESIAN_POINT ( 'NONE',  ( 20.08610463437157279, 13.29999999999998650, -27.64615127144129758 ) ) ;
#22443 = CARTESIAN_POINT ( 'NONE',  ( -24.18731323226221974, 44.22097249907603356, 14.01125832528330406 ) ) ;
#22444 = CARTESIAN_POINT ( 'NONE',  ( 20.75514604977249178, 55.82500000273119412, 28.56700777964553950 ) ) ;
#22445 = CARTESIAN_POINT ( 'NONE',  ( 27.16883889988623935, 46.57500000273117990, -19.73931689729374384 ) ) ;
#22446 = CARTESIAN_POINT ( 'NONE',  ( 5.147494310547426899, 45.44874571845313938, -32.50000000000000000 ) ) ;
#22447 = CARTESIAN_POINT ( 'NONE',  ( 5.147494310547434893, 67.05125428700921475, 32.49999999999999289 ) ) ;
#22448 = CARTESIAN_POINT ( 'NONE',  ( -26.29305231718579350, 49.80000000000001137, -19.10302069950537884 ) ) ;
#22449 = CARTESIAN_POINT ( 'NONE',  ( 26.06988505166735592, 45.80767333425730925, 7.025853678916393896 ) ) ;
#22450 = CARTESIAN_POINT ( 'NONE',  ( -1.778240108872766143E-15, 64.00000000546238255, -32.49999999999999289 ) ) ;
#22451 = CARTESIAN_POINT ( 'NONE',  ( 7.570916362186213000, 4.399999999999987033, -23.30088464923126423 ) ) ;
#22452 = CARTESIAN_POINT ( 'NONE',  ( -33.58253175000000113, 25.02500000273117209, -10.91162601494193218 ) ) ;
#22453 = CARTESIAN_POINT ( 'NONE',  ( -8.891200544363830713E-16, 77.75000000546235412, -15.00000000000000000 ) ) ;
#22454 = DIRECTION ( 'NONE',  ( -0.000000000000000000, 1.000000000000000000, -0.000000000000000000 ) ) ;
#22455 = CARTESIAN_POINT ( 'NONE',  ( -7.468012846824272799, 64.41628499907602645, 28.02196122052058413 ) ) ;
#22456 = CARTESIAN_POINT ( 'NONE',  ( -26.29305231718579350, 44.30000000546237260, -19.10302069950537884 ) ) ;
#22457 = CARTESIAN_POINT ( 'NONE',  ( 8.151180760100182884E-15, -89.55944200217849982, 0.000000000000000000 ) ) ;
#22458 = CARTESIAN_POINT ( 'NONE',  ( -20.75514604977248823, 34.82500000273118701, -28.56700777964554305 ) ) ;
#22459 = CARTESIAN_POINT ( 'NONE',  ( -19.09188309203660694, 35.20312500000000000, 19.09188309203694800 ) ) ;
#22460 = ORIENTED_EDGE ( 'NONE', *, *, #24344, .F. ) ;
#22461 = CARTESIAN_POINT ( 'NONE',  ( -20.75514604977248112, 71.42500000273119554, 28.56700777964554661 ) ) ;
#22462 = CARTESIAN_POINT ( 'NONE',  ( 28.01184896238304134, 37.49479166666666430, 7.505752307972846538 ) ) ;
#22463 = EDGE_CURVE ( 'NONE', #11212, #21883, #19774, .T. ) ;
#22464 = DIRECTION ( 'NONE',  ( 0.000000000000000000, 0.000000000000000000, 1.000000000000000000 ) ) ;
#22465 = ORIENTED_EDGE ( 'NONE', *, *, #22567, .F. ) ;
#22466 = CARTESIAN_POINT ( 'NONE',  ( 20.47846945139902530, 63.28163166759064495, 20.53372385742071771 ) ) ;
#22467 = CARTESIAN_POINT ( 'NONE',  ( -14.01125832528285109, 63.99777750092396644, 24.18731323226248264 ) ) ;
#22468 = CARTESIAN_POINT ( 'NONE',  ( 10.04305231718579705, 57.10000000546237686, 30.90933677959248982 ) ) ;
#22469 = CARTESIAN_POINT ( 'NONE',  ( 26.29305231718578995, 9.700000005462380059, -19.10302069950538240 ) ) ;
#22470 = EDGE_CURVE ( 'NONE', #26665, #20887, #29444, .T. ) ;
#22471 = CARTESIAN_POINT ( 'NONE',  ( -7.505752307973343918, 63.84895833333332860, -28.01184896238290989 ) ) ;
#22472 = CARTESIAN_POINT ( 'NONE',  ( 32.50000000000000711, 20.90000000000000924, 10.55989012756945122 ) ) ;
#22473 = CARTESIAN_POINT ( 'NONE',  ( 33.58253175000000113, 40.47500000273118559, -10.91162601494193751 ) ) ;
#22474 = CARTESIAN_POINT ( 'NONE',  ( -26.29305231718579350, 46.30000000546238681, -19.10302069950537884 ) ) ;
#22475 = CARTESIAN_POINT ( 'NONE',  ( -8.601468415847518756, 75.07500000273118701, -11.83890561707634781 ) ) ;
#22476 = CARTESIAN_POINT ( 'NONE',  ( 20.75514604977249178, 31.82500000273119056, 28.56700777964553950 ) ) ;
#22477 = CARTESIAN_POINT ( 'NONE',  ( 19.82091636218621034, 13.54999999453762527, 14.40073868116559730 ) ) ;
#22478 = CARTESIAN_POINT ( 'NONE',  ( 10.37757302488624767, 57.97500000273119980, 31.93888565452638417 ) ) ;
#22479 = CARTESIAN_POINT ( 'NONE',  ( -32.50000000000000000, 37.89999999999999858, -10.55989012756945478 ) ) ;
#22480 = CARTESIAN_POINT ( 'NONE',  ( -26.29305231718578995, 32.20000000000000284, 19.10302069950538595 ) ) ;
#22481 = CARTESIAN_POINT ( 'NONE',  ( -7.236395654485757944, 17.22499999726881370, -22.27133577429736988 ) ) ;
#22482 = CARTESIAN_POINT ( 'NONE',  ( 33.58253175000000113, 76.22500000273119269, -10.91162601494193751 ) ) ;
#22483 = DIRECTION ( 'NONE',  ( 1.224646799147353454E-16, -1.000000000000000000, 0.000000000000000000 ) ) ;
#22484 = CARTESIAN_POINT ( 'NONE',  ( 11.25946833292375793, 76.17500000273119554, 8.180482586598731842 ) ) ;
#22485 = CARTESIAN_POINT ( 'NONE',  ( 20.75514604977249178, 68.07500000273118701, 28.56700777964553950 ) ) ;
#22486 = CARTESIAN_POINT ( 'NONE',  ( -4.635254915624211769, 79.85000000546239107, -14.26584774442730286 ) ) ;
#22487 = ORIENTED_EDGE ( 'NONE', *, *, #21593, .T. ) ;
#22488 = CARTESIAN_POINT ( 'NONE',  ( -7.570916362186215665, 5.149999994537635573, 23.30088464923126423 ) ) ;
#22489 = CARTESIAN_POINT ( 'NONE',  ( 24.22776226481241224, 21.31548583425730925, -13.94119854578936923 ) ) ;
#22490 = CARTESIAN_POINT ( 'NONE',  ( 24.50000000000000000, 7.749999994537626336, 0.000000000000000000 ) ) ;
#22491 = CARTESIAN_POINT ( 'NONE',  ( 20.75514604977249178, 41.82500000273119412, 28.56700777964553950 ) ) ;
#22492 = CARTESIAN_POINT ( 'NONE',  ( 20.75514604977249178, 4.075000002731181681, 28.56700777964553950 ) ) ;
#22493 = CARTESIAN_POINT ( 'NONE',  ( 10.37757302488624056, 54.77500000273121117, -31.93888565452638417 ) ) ;
#22494 =( BOUNDED_CURVE ( )  B_SPLINE_CURVE ( 2, ( #24851, #9746, #19878, #20232, #30672, #32735, #17483, #27945, #9228, #30331, #19712, #30158, #33946 ),
 .UNSPECIFIED., .F., .T. ) 
 B_SPLINE_CURVE_WITH_KNOTS ( ( 3, 2, 2, 2, 2, 2, 3 ),
 ( 0.9423076923076922906, 0.9435897435897435681, 0.9461538461538461231, 0.9487179487179486781, 0.9512820512820512331, 0.9538461538461538991, 0.9551282051282051766 ),
 .UNSPECIFIED. ) 
 CURVE ( )  GEOMETRIC_REPRESENTATION_ITEM ( )  RATIONAL_B_SPLINE_CURVE ( ( 0.9755282581475768211, 0.9755282581475768211, 1.000000000000000000, 0.9510565162951535312, 1.000000000000000000, 0.9510565162951535312, 1.000000000000000000, 0.9510565162951535312, 1.000000000000000000, 0.9510565162951535312, 1.000000000000000000, 0.9755282581475768211, 0.9755282581475768211 ) ) 
 REPRESENTATION_ITEM ( '' )  );
#22495 = CARTESIAN_POINT ( 'NONE',  ( 7.468012846824777284, 46.38059000092397355, 28.02196122052045268 ) ) ;
#22496 = CARTESIAN_POINT ( 'NONE',  ( -14.97647472619899389, 37.05951416574268364, 26.02091320914878025 ) ) ;
#22497 = CARTESIAN_POINT ( 'NONE',  ( 10.04305231718579705, 63.10000000546238397, 30.90933677959248982 ) ) ;
#22498 = CARTESIAN_POINT ( 'NONE',  ( -13.91746824999999887, 81.37500000273118417, 0.000000000000000000 ) ) ;
#22499 =( BOUNDED_CURVE ( )  B_SPLINE_CURVE ( 2, ( #66, #10552, #31483, #18459, #12615, #31645, #906, #31812, #3497, #29068, #32146, #26838, #10723 ),
 .UNSPECIFIED., .F., .T. ) 
 B_SPLINE_CURVE_WITH_KNOTS ( ( 3, 2, 2, 2, 2, 2, 3 ),
 ( 0.1602564102564102699, 0.1615384615384615474, 0.1641025641025641024, 0.1666666666666666574, 0.1692307692307692402, 0.1717948717948717952, 0.1730769230769230727 ),
 .UNSPECIFIED. ) 
 CURVE ( )  GEOMETRIC_REPRESENTATION_ITEM ( )  RATIONAL_B_SPLINE_CURVE ( ( 0.9755282581475768211, 0.9755282581475770431, 1.000000000000000000, 0.9510565162951535312, 1.000000000000000000, 0.9510565162951535312, 1.000000000000000000, 0.9510565162951535312, 1.000000000000000000, 0.9510565162951535312, 1.000000000000000000, 0.9755282581475768211, 0.9755282581475768211 ) ) 
 REPRESENTATION_ITEM ( '' )  );
#22500 = CARTESIAN_POINT ( 'NONE',  ( -0.04044903255042732459, 65.99180583240935505, -27.95245687107223986 ) ) ;
#22501 = CARTESIAN_POINT ( 'NONE',  ( -5.147494310547430452, 53.55125428154685352, -32.49999999999999289 ) ) ;
#22502 = CARTESIAN_POINT ( 'NONE',  ( 20.50609665440969565, 12.85937500000000000, -20.50609665441004736 ) ) ;
#22503 = CARTESIAN_POINT ( 'NONE',  ( -33.58253175000000113, 39.47500000273117848, 10.91162601494193929 ) ) ;
#22504 = CARTESIAN_POINT ( 'NONE',  ( -26.29305231718579350, 75.80000000000001137, -19.10302069950537884 ) ) ;
#22505 = VERTEX_POINT ( 'NONE', #30230 ) ;
#22506 = CARTESIAN_POINT ( 'NONE',  ( -20.08610463437156923, 28.80000000546238326, 27.64615127144130113 ) ) ;
#22507 = ORIENTED_EDGE ( 'NONE', *, *, #23495, .T. ) ;
#22508 = CARTESIAN_POINT ( 'NONE',  ( -30.02300923189239512, 35.63281249999998579, 2.654126918244515359E-13 ) ) ;
#22509 = CARTESIAN_POINT ( 'NONE',  ( -10.04305231718579172, 60.10000000546239818, -30.90933677959248982 ) ) ;
#22510 = EDGE_LOOP ( 'NONE', ( #31377, #29223 ) ) ;
#22511 = CARTESIAN_POINT ( 'NONE',  ( -12.11607355459419644, -70.99969134886156041, 0.000000000000000000 ) ) ;
#22512 = VECTOR ( 'NONE', #18202, 1000.000000000000114 ) ;
#22513 = CARTESIAN_POINT ( 'NONE',  ( -20.75514604977248112, 47.42500000273118843, 28.56700777964554661 ) ) ;
#22514 = CARTESIAN_POINT ( 'NONE',  ( 10.04305231718578817, 55.90000000546238823, -30.90933677959249337 ) ) ;
#22515 = CARTESIAN_POINT ( 'NONE',  ( -20.50609665440969209, 62.70312500000000000, 20.50609665441005092 ) ) ;
#22516 = CARTESIAN_POINT ( 'NONE',  ( -20.08610463437157989, 10.20000000546238539, -27.64615127144129758 ) ) ;
#22517 = DIRECTION ( 'NONE',  ( -0.000000000000000000, 1.000000000000000000, -0.000000000000000000 ) ) ;
#22518 = CARTESIAN_POINT ( 'NONE',  ( 18.94512977948575738, 14.92499999726881654, 13.76444248337723408 ) ) ;
#22519 = CARTESIAN_POINT ( 'NONE',  ( -20.08610463437157989, 55.69999999999998863, -27.64615127144129758 ) ) ;
#22520 = CARTESIAN_POINT ( 'NONE',  ( 4.635254915624209993, 77.65000000546234560, -14.26584774442730463 ) ) ;
#22521 = CARTESIAN_POINT ( 'NONE',  ( -27.16883889988623935, 17.57500000273118346, 19.73931689729374739 ) ) ;
#22522 = CARTESIAN_POINT ( 'NONE',  ( 10.04305231718579705, 5.100000005462374197, 30.90933677959248982 ) ) ;
#22523 = CARTESIAN_POINT ( 'NONE',  ( -0.04044903255042732459, 21.30430583240935860, -27.95245687107223986 ) ) ;
#22524 = CARTESIAN_POINT ( 'NONE',  ( -4.300734207923755825, 77.27500000273118985, 13.23629886949340673 ) ) ;
#22525 = LINE ( 'NONE', #6909, #16243 ) ;
#22526 = CARTESIAN_POINT ( 'NONE',  ( 20.08610463437158344, 53.20000000546237118, 27.64615127144129403 ) ) ;
#22527 = CARTESIAN_POINT ( 'NONE',  ( -32.50000000000000000, 2.100000000000006306, 10.55989012756946366 ) ) ;
#22528 = EDGE_LOOP ( 'NONE', ( #18759, #16481, #33218, #16451 ) ) ;
#22529 = CARTESIAN_POINT ( 'NONE',  ( 23.41746825000000243, 9.224999997268820806, -7.608796670333727974 ) ) ;
#22530 = DIRECTION ( 'NONE',  ( -0.000000000000000000, -1.000000000000000000, -0.000000000000000000 ) ) ;
#22531 = AXIS2_PLACEMENT_3D ( 'NONE', #10503, #18409, #5353 ) ;
#22532 = CARTESIAN_POINT ( 'NONE',  ( -6.988114217768288228, 46.66145833333332860, -26.07999730980477437 ) ) ;
#22533 = CARTESIAN_POINT ( 'NONE',  ( 20.75514604977249178, 61.82500000273116569, 28.56700777964553950 ) ) ;
#22534 = CARTESIAN_POINT ( 'NONE',  ( 33.58253175000000113, 24.47500000273118914, -10.91162601494193751 ) ) ;
#22535 = CARTESIAN_POINT ( 'NONE',  ( 10.37757302488624767, 7.975000002731199800, 31.93888565452638417 ) ) ;
#22536 = CARTESIAN_POINT ( 'NONE',  ( 5.779280353836490358E-15, 20.49999999999999645, 32.49999999999999289 ) ) ;
#22537 = CARTESIAN_POINT ( 'NONE',  ( -7.025853678916393008, 63.85454833425732346, 26.06988505166735592 ) ) ;
#22538 = CARTESIAN_POINT ( 'NONE',  ( 15.01150461594596308, 60.84114583333332860, -26.00068869287367335 ) ) ;
#22539 = CARTESIAN_POINT ( 'NONE',  ( 13.91746825000000065, 72.27500000273118985, 4.522059556121115875 ) ) ;
#22540 = CARTESIAN_POINT ( 'NONE',  ( 32.50000000000000711, 44.90000000000001279, 10.55989012756945122 ) ) ;
#22541 = CARTESIAN_POINT ( 'NONE',  ( -33.58253175000000113, 53.12500000273118417, 0.000000000000000000 ) ) ;
#22542 = CARTESIAN_POINT ( 'NONE',  ( -7.236395654485763274, 6.024999997268825958, 22.27133577429736633 ) ) ;
#22543 = CARTESIAN_POINT ( 'NONE',  ( -19.09188309203660694, 66.14062500000000000, 19.09188309203694800 ) ) ;
#22544 = ORIENTED_EDGE ( 'NONE', *, *, #26245, .T. ) ;
#22545 = CARTESIAN_POINT ( 'NONE',  ( 6.486482029760649416E-15, 61.87500000273117706, 35.31076352940723240 ) ) ;
#22546 = CARTESIAN_POINT ( 'NONE',  ( 23.41746825000000243, 10.72499999726880127, -7.608796670333727974 ) ) ;
#22547 = CARTESIAN_POINT ( 'NONE',  ( -27.95245687107223986, 37.07069416759063785, -0.04044903254993292840 ) ) ;
#22548 = ORIENTED_EDGE ( 'NONE', *, *, #14116, .F. ) ;
#22549 = CARTESIAN_POINT ( 'NONE',  ( 20.75514604977248467, 32.42500000273116711, -28.56700777964554305 ) ) ;
#22550 = CARTESIAN_POINT ( 'NONE',  ( 15.14183272437242067, 5.699999999999993960, 20.84094480462498211 ) ) ;
#22551 = ORIENTED_EDGE ( 'NONE', *, *, #21679, .F. ) ;
#22552 = CARTESIAN_POINT ( 'NONE',  ( 20.50609665440969565, 64.42187499999998579, -20.50609665441004736 ) ) ;
#22553 = CARTESIAN_POINT ( 'NONE',  ( 33.58253175000000113, 58.47500000273118559, -10.91162601494193751 ) ) ;
#22554 = CARTESIAN_POINT ( 'NONE',  ( 26.29305231718579350, 69.30000000546237970, 19.10302069950537529 ) ) ;
#22555 = CARTESIAN_POINT ( 'NONE',  ( -33.58253175000000113, 69.22500000273117848, 10.91162601494193929 ) ) ;
#22556 = CARTESIAN_POINT ( 'NONE',  ( 7.505752307972854531, 36.63541666666666430, -28.01184896238303423 ) ) ;
#22557 = EDGE_CURVE ( 'NONE', #25888, #27023, #28547, .T. ) ;
#22558 = CARTESIAN_POINT ( 'NONE',  ( 7.570916362186207671, 15.60000000000000320, 23.30088464923126779 ) ) ;
#22559 = CARTESIAN_POINT ( 'NONE',  ( 33.58253175000000113, 2.475000002731187809, -10.91162601494193751 ) ) ;
#22560 = CARTESIAN_POINT ( 'NONE',  ( 10.37757302488624056, 8.525000002731180970, -31.93888565452638417 ) ) ;
#22561 = CARTESIAN_POINT ( 'NONE',  ( -13.91746824999999887, 74.87500000273116996, 0.000000000000000000 ) ) ;
#22562 = CARTESIAN_POINT ( 'NONE',  ( 20.47846945139867003, 49.23399333240936215, -20.53372385742107653 ) ) ;
#22563 =( GEOMETRIC_REPRESENTATION_CONTEXT ( 3 ) GLOBAL_UNCERTAINTY_ASSIGNED_CONTEXT ( ( #10193 ) ) GLOBAL_UNIT_ASSIGNED_CONTEXT ( ( #10720, #13802, #8140 ) ) REPRESENTATION_CONTEXT ( 'NONE', 'WORKASPACE' ) );
#22564 = CARTESIAN_POINT ( 'NONE',  ( -9.270509831248425314, 73.70000000000000284, -12.75976212528059861 ) ) ;
#22565 = CARTESIAN_POINT ( 'NONE',  ( 7.505752307972854531, 53.82291666666666430, -28.01184896238303423 ) ) ;
#22566 = DIRECTION ( 'NONE',  ( 0.000000000000000000, -1.000000000000000000, 0.000000000000000000 ) ) ;
#22567 = EDGE_CURVE ( 'NONE', #20505, #29467, #32803, .T. ) ;
#22568 = CARTESIAN_POINT ( 'NONE',  ( 10.04305231718578817, 23.40000000000000568, -30.90933677959249337 ) ) ;
#22569 = CARTESIAN_POINT ( 'NONE',  ( 15.14183272437241889, 9.449999994537636283, 20.84094480462498211 ) ) ;
#22570 = CARTESIAN_POINT ( 'NONE',  ( -15.00000000000000000, 78.25000000546239676, 0.000000000000000000 ) ) ;
#22571 = CARTESIAN_POINT ( 'NONE',  ( -24.20753774853730889, 18.15885416666666075, 13.97622843553633842 ) ) ;
#22572 = CARTESIAN_POINT ( 'NONE',  ( 10.37757302488624056, 38.52500000273118275, -31.93888565452638417 ) ) ;
#22573 = CARTESIAN_POINT ( 'NONE',  ( -8.601468415847518756, 72.57500000273114438, -11.83890561707634781 ) ) ;
#22574 = CARTESIAN_POINT ( 'NONE',  ( 33.58253175000000113, 40.37500000273118417, -4.112674001490185761E-15 ) ) ;
#22575 = CARTESIAN_POINT ( 'NONE',  ( 10.37757302488624767, 25.97500000273117493, 31.93888565452638417 ) ) ;
#22576 = CARTESIAN_POINT ( 'NONE',  ( 32.50000000000000711, 40.89999999999998437, 10.55989012756945122 ) ) ;
#22577 = EDGE_CURVE ( 'NONE', #5051, #601, #1537, .T. ) ;
#22578 = DIRECTION ( 'NONE',  ( -0.000000000000000000, 1.000000000000000000, -0.000000000000000000 ) ) ;
#22579 = CARTESIAN_POINT ( 'NONE',  ( -4.405589869732278832E-13, 32.49999999999997868, 32.50000000000000000 ) ) ;
#22580 = CARTESIAN_POINT ( 'NONE',  ( 6.277390505771533514E-15, 66.49999999999998579, 34.17252228774368916 ) ) ;
#22581 = CARTESIAN_POINT ( 'NONE',  ( 14.47279130897151767, 10.32499999726881335, 19.92008829642072953 ) ) ;
#22582 = CARTESIAN_POINT ( 'NONE',  ( 28.00173670424535644, 22.02045166574269075, -7.543491769121920321 ) ) ;
#22583 = CARTESIAN_POINT ( 'NONE',  ( 14.47279130897151767, 3.424999997268800112, -19.92008829642072598 ) ) ;
#22584 = CARTESIAN_POINT ( 'NONE',  ( 26.09010956794244507, 39.49440999907601224, 6.950374756619249084 ) ) ;
#22585 =( NAMED_UNIT ( * ) PLANE_ANGLE_UNIT ( ) SI_UNIT ( $, .RADIAN. ) );
#22586 = CARTESIAN_POINT ( 'NONE',  ( -20.75514604977248112, 11.42500000273116711, 28.56700777964554661 ) ) ;
#22587 = CARTESIAN_POINT ( 'NONE',  ( 23.41746824999999887, 15.12499999726882294, 0.000000000000000000 ) ) ;
#22588 = CARTESIAN_POINT ( 'NONE',  ( 19.09188309203661049, 60.98437499999999289, -19.09188309203694445 ) ) ;
#22589 = ORIENTED_EDGE ( 'NONE', *, *, #25382, .F. ) ;
#22590 = CARTESIAN_POINT ( 'NONE',  ( -10.37757302488623701, 51.52500000273117564, 31.93888565452638417 ) ) ;
#22591 = CARTESIAN_POINT ( 'NONE',  ( 10.37757302488624767, 19.97500000273118204, 31.93888565452638417 ) ) ;
#22592 =( BOUNDED_CURVE ( )  B_SPLINE_CURVE ( 2, ( #27251, #29317, #32390, #13715, #16960, #3576, #16296, #822, #8885, #14048, #653, #13884, #13553 ),
 .UNSPECIFIED., .F., .T. ) 
 B_SPLINE_CURVE_WITH_KNOTS ( ( 3, 2, 2, 2, 2, 2, 3 ),
 ( 0.8499999999999999778, 0.8599999999999999867, 0.8800000000000000044, 0.9000000000000000222, 0.9200000000000000400, 0.9399999999999999467, 0.9499999999999999556 ),
 .UNSPECIFIED. ) 
 CURVE ( )  GEOMETRIC_REPRESENTATION_ITEM ( )  RATIONAL_B_SPLINE_CURVE ( ( 0.9755282581475768211, 0.9755282581475768211, 1.000000000000000000, 0.9510565162951535312, 1.000000000000000000, 0.9510565162951535312, 1.000000000000000000, 0.9510565162951535312, 1.000000000000000000, 0.9510565162951535312, 1.000000000000000000, 0.9755282581475768211, 0.9755282581475768211 ) ) 
 REPRESENTATION_ITEM ( '' )  );
#22593 = EDGE_LOOP ( 'NONE', ( #29884, #27527, #13457, #27575 ) ) ;
#22594 = CARTESIAN_POINT ( 'NONE',  ( -20.50609665440969209, 35.20312500000000000, 20.50609665441005092 ) ) ;
#22595 = CARTESIAN_POINT ( 'NONE',  ( 30.02300923189239867, 35.35194416759064495, 0.04044903254992252006 ) ) ;
#22596 = DIRECTION ( 'NONE',  ( 0.000000000000000000, 1.000000000000000000, 0.000000000000000000 ) ) ;
#22597 = CARTESIAN_POINT ( 'NONE',  ( -15.14183272437241889, 16.44999999453761319, -20.84094480462497856 ) ) ;
#22598 = CARTESIAN_POINT ( 'NONE',  ( 23.41746824999999887, 12.62499999726882116, 0.000000000000000000 ) ) ;
#22599 = CARTESIAN_POINT ( 'NONE',  ( -10.37757302488624411, 24.97500000273117493, -31.93888565452638417 ) ) ;
#22600 = CARTESIAN_POINT ( 'NONE',  ( 32.50000000000000711, 27.40000000546239534, 10.55989012756945122 ) ) ;
#22601 = CARTESIAN_POINT ( 'NONE',  ( -2.092463501923844636E-15, 67.50000000000000000, -34.17252228774368916 ) ) ;
#22602 = DIRECTION ( 'NONE',  ( -0.000000000000000000, -1.000000000000000000, -0.000000000000000000 ) ) ;
#22603 = CARTESIAN_POINT ( 'NONE',  ( -0.3918072299880378528, 74.00000000000004263, 14.19424161045959210 ) ) ;
#22604 = CARTESIAN_POINT ( 'NONE',  ( 7.505752307972854531, 12.57291666666666252, -28.01184896238303423 ) ) ;
#22605 = CARTESIAN_POINT ( 'NONE',  ( 20.75514604977248467, 38.67500000273117422, -28.56700777964554305 ) ) ;
#22606 = CARTESIAN_POINT ( 'NONE',  ( -5.147494310547423346, 32.94874572391555034, 32.50000000000000000 ) ) ;
#22607 = CARTESIAN_POINT ( 'NONE',  ( -2.584737979205442066E-13, 26.17968750000000000, -30.02300923189239867 ) ) ;
#22608 = DIRECTION ( 'NONE',  ( 0.000000000000000000, 0.000000000000000000, 1.000000000000000000 ) ) ;
#22609 = AXIS2_PLACEMENT_3D ( 'NONE', #18106, #21023, #26162 ) ;
#22610 = CARTESIAN_POINT ( 'NONE',  ( 40.00000000000000000, 66.99999999999998579, 23.09401076758503990 ) ) ;
#22611 = CARTESIAN_POINT ( 'NONE',  ( 32.50000000000000711, 16.89999999999998437, 10.55989012756945122 ) ) ;
#22612 = CARTESIAN_POINT ( 'NONE',  ( -32.50000000000000000, 51.99999999999999289, 0.000000000000000000 ) ) ;
#22613 = CARTESIAN_POINT ( 'NONE',  ( 26.09010956794244507, 46.36940999907602645, 6.950374756619249084 ) ) ;
#22614 = CARTESIAN_POINT ( 'NONE',  ( 10.37757302488624767, 59.72500000273117848, 31.93888565452638417 ) ) ;
#22615 = CARTESIAN_POINT ( 'NONE',  ( -27.16883889988623935, 59.57500000273117990, 19.73931689729374739 ) ) ;
#22616 = CARTESIAN_POINT ( 'NONE',  ( -27.16883889988623935, 47.57500000273117990, 19.73931689729374739 ) ) ;
#22617 = CARTESIAN_POINT ( 'NONE',  ( 10.04305231718579705, 44.60000000000000142, 30.90933677959248982 ) ) ;
#22618 = CARTESIAN_POINT ( 'NONE',  ( 24.50000000000000000, 10.10000000000000142, -7.960532557706203605 ) ) ;
#22619 = CARTESIAN_POINT ( 'NONE',  ( -5.147494310547423346, 50.44874571845315359, 32.50000000000000000 ) ) ;
#22620 = CARTESIAN_POINT ( 'NONE',  ( 24.18731323226247554, 52.82590250092398065, 14.01125832528285997 ) ) ;
#22621 = ADVANCED_FACE ( 'NONE', ( #12744 ), #18072, .F. ) ;
#22622 = CARTESIAN_POINT ( 'NONE',  ( -15.14183272437242067, 4.449999994537617631, -20.84094480462497856 ) ) ;
#22623 = CARTESIAN_POINT ( 'NONE',  ( 3.880418787951150694, 4.448745718453149145, -24.49999999999999645 ) ) ;
#22624 = CARTESIAN_POINT ( 'NONE',  ( 27.16883889988623935, 22.32500000273117280, -19.73931689729374384 ) ) ;
#22625 = DIRECTION ( 'NONE',  ( -0.000000000000000000, 1.000000000000000000, -0.000000000000000000 ) ) ;
#22626 = CARTESIAN_POINT ( 'NONE',  ( 2.205017735002230837E-13, 56.00000000546238255, -32.50000000000000000 ) ) ;
#22627 = CARTESIAN_POINT ( 'NONE',  ( 5.779280353836490358E-15, 41.00000000546237544, 32.49999999999999289 ) ) ;
#22628 = CARTESIAN_POINT ( 'NONE',  ( 20.47846945139867003, 62.98399333240935505, -20.53372385742107653 ) ) ;
#22629 = CARTESIAN_POINT ( 'NONE',  ( 26.29305231718579350, 43.30000000546237260, 19.10302069950537529 ) ) ;
#22630 = CARTESIAN_POINT ( 'NONE',  ( 20.08610463437157279, 35.29999999999999716, -27.64615127144129758 ) ) ;
#22632 = CARTESIAN_POINT ( 'NONE',  ( -33.58253175000000113, 35.02500000273117564, -10.91162601494193041 ) ) ;
#22631 = AXIS2_PLACEMENT_3D ( 'NONE', #8742, #32080, #21964 ) ;
#22633 = CARTESIAN_POINT ( 'NONE',  ( 20.75514604977249178, 64.07500000273120122, 28.56700777964553950 ) ) ;
#22634 = CARTESIAN_POINT ( 'NONE',  ( -13.97622843553588901, 35.05989583333332860, 24.20753774853756823 ) ) ;
#22635 = ORIENTED_EDGE ( 'NONE', *, *, #29784, .T. ) ;
#22636 = AXIS2_PLACEMENT_3D ( 'NONE', #7973, #2140, #31144 ) ;
#22637 = CARTESIAN_POINT ( 'NONE',  ( -2.162160676586881955E-15, 68.62500000273119838, -35.31076352940723240 ) ) ;
#22638 = CARTESIAN_POINT ( 'NONE',  ( 20.50609665441005092, 41.21875000000000000, 20.50609665440969209 ) ) ;
#22639 = CARTESIAN_POINT ( 'NONE',  ( 0.000000000000000000, 74.00000000000001421, 0.000000000000000000 ) ) ;
#22640 = EDGE_LOOP ( 'NONE', ( #21223, #8459, #26868, #721 ) ) ;
#22641 = CARTESIAN_POINT ( 'NONE',  ( 26.02091320914851025, 55.69048583425730925, -14.97647472619946463 ) ) ;
#22642 = CARTESIAN_POINT ( 'NONE',  ( -19.06425588902591173, 61.56288166759063074, -19.11951029504763611 ) ) ;
#22643 = CARTESIAN_POINT ( 'NONE',  ( 27.16883889988624290, 11.92500000273118133, 19.73931689729373673 ) ) ;
#22644 = CARTESIAN_POINT ( 'NONE',  ( -14.97647472619899389, 16.43451416574268720, 26.02091320914878025 ) ) ;
#22645 = CARTESIAN_POINT ( 'NONE',  ( -33.58253175000000113, 39.47500000273117848, 10.91162601494193929 ) ) ;
#22646 = CARTESIAN_POINT ( 'NONE',  ( 20.08610463437157279, 41.80000000546237260, -27.64615127144129758 ) ) ;
#22647 = CARTESIAN_POINT ( 'NONE',  ( -13.91746824999999532, 71.47500000273119269, 4.522059556121122093 ) ) ;
#22648 = CARTESIAN_POINT ( 'NONE',  ( -33.58253175000000113, 29.22500000273118914, 10.91162601494193929 ) ) ;
#22649 = CARTESIAN_POINT ( 'NONE',  ( 3.880418787951140036, 14.19874571299077637, -24.49999999999999645 ) ) ;
#22650 = CARTESIAN_POINT ( 'NONE',  ( -27.16883889988624290, 53.17500000273117422, -19.73931689729374028 ) ) ;
#22651 = CARTESIAN_POINT ( 'NONE',  ( 20.08610463437158344, 38.70000000000000284, 27.64615127144129403 ) ) ;
#22652 = CARTESIAN_POINT ( 'NONE',  ( 32.50000000000000711, 34.89999999999999858, 10.55989012756945122 ) ) ;
#22653 = CARTESIAN_POINT ( 'NONE',  ( 18.94512977948576093, 14.82499999726880091, -13.76444248337722875 ) ) ;
#22654 = CARTESIAN_POINT ( 'NONE',  ( 10.37757302488624767, 75.72500000273119269, 31.93888565452638417 ) ) ;
#22655 = CARTESIAN_POINT ( 'NONE',  ( 0.000000000000000000, 80.00000000000001421, -32.50000000000000000 ) ) ;
#22656 = DIRECTION ( 'NONE',  ( -0.000000000000000000, 1.000000000000000000, -0.000000000000000000 ) ) ;
#22657 = CARTESIAN_POINT ( 'NONE',  ( -10.37757302488623701, 69.77500000273117564, 31.93888565452638417 ) ) ;
#22658 = CARTESIAN_POINT ( 'NONE',  ( 9.270509831248423538, 75.55000000546242234, -12.75976212528059861 ) ) ;
#22659 = AXIS2_PLACEMENT_3D ( 'NONE', #20062, #22972, #14909 ) ;
#22660 = VERTEX_POINT ( 'NONE', #9824 ) ;
#22661 = CARTESIAN_POINT ( 'NONE',  ( 33.58253175000000113, 18.12500000273117706, -4.112674001490185761E-15 ) ) ;
#22662 = CARTESIAN_POINT ( 'NONE',  ( -24.50000000000000000, 12.74999999453763166, -3.000384657911015469E-15 ) ) ;
#22663 = CARTESIAN_POINT ( 'NONE',  ( 19.11951029504763611, 24.60975666759063785, -19.06425588902591173 ) ) ;
#22664 = EDGE_CURVE ( 'NONE', #9328, #24994, #2447, .T. ) ;
#22665 = CARTESIAN_POINT ( 'NONE',  ( 5.147494310547327423, 46.55125428154685352, 32.50000000000003553 ) ) ;
#22666 = CARTESIAN_POINT ( 'NONE',  ( -33.58253175000000113, 41.02500000273118985, -10.91162601494193218 ) ) ;
#22667 = CARTESIAN_POINT ( 'NONE',  ( -27.16883889988623935, 7.575000002731188786, 19.73931689729374739 ) ) ;
#22668 = CARTESIAN_POINT ( 'NONE',  ( 10.37757302488624056, 52.77500000273120406, -31.93888565452638417 ) ) ;
#22669 = CARTESIAN_POINT ( 'NONE',  ( 26.02091320914851025, 48.81548583425731636, -14.97647472619946463 ) ) ;
#22670 = ADVANCED_FACE ( 'NONE', ( #14805 ), #23217, .F. ) ;
#22671 = CARTESIAN_POINT ( 'NONE',  ( 7.468012846824281681, 35.19753499907601935, -28.02196122052058058 ) ) ;
#22672 = CARTESIAN_POINT ( 'NONE',  ( -2.092463501923844636E-15, 60.00000000546238255, -34.17252228774368916 ) ) ;
#22673 = CARTESIAN_POINT ( 'NONE',  ( -11.25946833292375793, 75.07500000273120122, 8.180482586598737171 ) ) ;
#22674 = CARTESIAN_POINT ( 'NONE',  ( -13.94119854578892514, 67.99701416574269786, 24.22776226481266448 ) ) ;
#22675 = DIRECTION ( 'NONE',  ( 0.4999999999999996114, 0.000000000000000000, -0.8660254037844388186 ) ) ;
#22676 = CARTESIAN_POINT ( 'NONE',  ( 20.08610463437157279, 77.80000000546237970, -27.64615127144129758 ) ) ;
#22677 = CARTESIAN_POINT ( 'NONE',  ( 28.01184896238304134, 16.86979166666666075, 7.505752307972846538 ) ) ;
#22678 = CARTESIAN_POINT ( 'NONE',  ( 20.75514604977249178, 42.07500000273117990, 28.56700777964553950 ) ) ;
#22679 = CARTESIAN_POINT ( 'NONE',  ( -4.523095164977117273E-15, 8.624999997268810503, 24.62258325217400312 ) ) ;
#22680 = ORIENTED_EDGE ( 'NONE', *, *, #14537, .T. ) ;
#22681 = CARTESIAN_POINT ( 'NONE',  ( -33.58253175000000113, 73.47500000273117848, 10.91162601494193929 ) ) ;
#22682 = VECTOR ( 'NONE', #8281, 1000.000000000000000 ) ;
#22683 = CARTESIAN_POINT ( 'NONE',  ( -26.29305231718578995, 28.70000000546237118, 19.10302069950538595 ) ) ;
#22684 = VERTEX_POINT ( 'NONE', #12223 ) ;
#22685 = AXIS2_PLACEMENT_3D ( 'NONE', #6574, #27000, #32147 ) ;
#22686 = CARTESIAN_POINT ( 'NONE',  ( 20.50609665440969565, 30.04687500000000000, -20.50609665441004736 ) ) ;
#22687 = CARTESIAN_POINT ( 'NONE',  ( 32.50000000000000000, 65.50000000546238255, -3.980102097228898626E-15 ) ) ;
#22688 = VERTEX_POINT ( 'NONE', #33677 ) ;
#22689 = CARTESIAN_POINT ( 'NONE',  ( 10.04305231718579705, 26.60000000000001208, 30.90933677959248982 ) ) ;
#22690 = CARTESIAN_POINT ( 'NONE',  ( -33.58253175000000113, 47.12500000273117706, 0.000000000000000000 ) ) ;
#22691 = CARTESIAN_POINT ( 'NONE',  ( 2.375766604868043252, 73.69874572391555034, -14.99999999999999822 ) ) ;
#22692 = CARTESIAN_POINT ( 'NONE',  ( 6.277390505771533514E-15, 3.000000005462379882, 34.17252228774368916 ) ) ;
#22693 = CARTESIAN_POINT ( 'NONE',  ( -15.00000000000000000, 78.10000000000002274, 4.873795443493597723 ) ) ;
#22694 = CARTESIAN_POINT ( 'NONE',  ( 20.50609665441005092, 13.71874999999999467, 20.50609665440969209 ) ) ;
#22695 = CARTESIAN_POINT ( 'NONE',  ( -32.50000000000000000, 51.89999999999998437, -10.55989012756945478 ) ) ;
#22696 = CARTESIAN_POINT ( 'NONE',  ( 0.000000000000000000, 80.00000000000001421, -32.50000000000000000 ) ) ;
#22697 = CARTESIAN_POINT ( 'NONE',  ( 10.37757302488624767, 15.97500000273119269, 31.93888565452638417 ) ) ;
#22698 = CARTESIAN_POINT ( 'NONE',  ( -7.570916362186210335, 6.599999999999994316, -23.30088464923126779 ) ) ;
#22699 = CARTESIAN_POINT ( 'NONE',  ( -13.94119854578892514, 23.30951416574269075, 24.22776226481266448 ) ) ;
#22700 = CARTESIAN_POINT ( 'NONE',  ( 4.300734207923761154, 71.47500000273119269, 13.23629886949340495 ) ) ;
#22701 = CARTESIAN_POINT ( 'NONE',  ( -3.712076227271900841E-14, 8.499999999999994671, -24.50000000000000000 ) ) ;
#22702 = CARTESIAN_POINT ( 'NONE',  ( 26.72982461517084474, 52.00000000000001421, 20.44820386143251767 ) ) ;
#22703 =( BOUNDED_CURVE ( )  B_SPLINE_CURVE ( 2, ( #32335, #19312, #16076, #5425, #15905, #2850, #29428, #32000, #8496, #3025, #5931, #13321, #31668 ),
 .UNSPECIFIED., .F., .T. ) 
 B_SPLINE_CURVE_WITH_KNOTS ( ( 3, 2, 2, 2, 2, 2, 3 ),
 ( 0.2243589743589743668, 0.2256410256410256443, 0.2282051282051281993, 0.2307692307692307820, 0.2333333333333333370, 0.2358974358974358920, 0.2371794871794871973 ),
 .UNSPECIFIED. ) 
 CURVE ( )  GEOMETRIC_REPRESENTATION_ITEM ( )  RATIONAL_B_SPLINE_CURVE ( ( 0.9755282581475768211, 0.9755282581475768211, 1.000000000000000000, 0.9510565162951535312, 1.000000000000000000, 0.9510565162951535312, 1.000000000000000000, 0.9510565162951535312, 1.000000000000000000, 0.9510565162951535312, 1.000000000000000000, 0.9755282581475764880, 0.9755282581475768211 ) ) 
 REPRESENTATION_ITEM ( '' )  );
#22704 = CARTESIAN_POINT ( 'NONE',  ( 27.16883889988623935, 78.57500000273120122, -19.73931689729374384 ) ) ;
#22705 = ORIENTED_EDGE ( 'NONE', *, *, #11667, .T. ) ;
#22706 = CARTESIAN_POINT ( 'NONE',  ( -14.47279130897152122, 14.42499999726880056, 19.92008829642072243 ) ) ;
#22707 = LINE ( 'NONE', #30239, #8512 ) ;
#22708 = MECHANICAL_DESIGN_GEOMETRIC_PRESENTATION_REPRESENTATION (  '', ( #9540 ), #13408 ) ;
#22709 = CARTESIAN_POINT ( 'NONE',  ( -24.20753774853756823, 49.66927083333330728, -13.97622843553588723 ) ) ;
#22710 =( BOUNDED_CURVE ( )  B_SPLINE_CURVE ( 2, ( #14851, #27721, #12616, #27893, #33373, #28402, #28061, #7117, #22917, #2141, #25142, #20528, #25317 ),
 .UNSPECIFIED., .F., .F. ) 
 B_SPLINE_CURVE_WITH_KNOTS ( ( 3, 2, 2, 2, 2, 2, 3 ),
 ( 0.3141025641025640969, 0.3153846153846153744, 0.3179487179487179294, 0.3205128205128205399, 0.3230769230769230949, 0.3256410256410256499, 0.3269230769230769273 ),
 .UNSPECIFIED. ) 
 CURVE ( )  GEOMETRIC_REPRESENTATION_ITEM ( )  RATIONAL_B_SPLINE_CURVE ( ( 0.9755282581475768211, 0.9755282581475768211, 1.000000000000000000, 0.9510565162951535312, 1.000000000000000000, 0.9510565162951535312, 1.000000000000000000, 0.9510565162951535312, 1.000000000000000000, 0.9510565162951535312, 1.000000000000000000, 0.9755282581475768211, 0.9755282581475768211 ) ) 
 REPRESENTATION_ITEM ( '' )  );
#22711 = CARTESIAN_POINT ( 'NONE',  ( 33.58253175000000823, 58.02500000273117564, 10.91162601494192863 ) ) ;
#22712 = CARTESIAN_POINT ( 'NONE',  ( -33.58253175000000113, 25.27500000273119696, -10.91162601494193218 ) ) ;
#22713 = CARTESIAN_POINT ( 'NONE',  ( -27.16883889988623935, 9.575000002731190563, 19.73931689729374739 ) ) ;
#22714 = CARTESIAN_POINT ( 'NONE',  ( -10.37757302488623701, 1.775000002731175197, 31.93888565452638417 ) ) ;
#22715 = CARTESIAN_POINT ( 'NONE',  ( 28.00173670424549499, 21.74517333425730925, 7.543491769121417612 ) ) ;
#22716 = EDGE_CURVE ( 'NONE', #9595, #29888, #23042, .T. ) ;
#22717 = CARTESIAN_POINT ( 'NONE',  ( 26.00068869287367335, 61.70052083333331439, 15.01150461594596308 ) ) ;
#22718 = EDGE_CURVE ( 'NONE', #13703, #3977, #12123, .T. ) ;
#22719 = CARTESIAN_POINT ( 'NONE',  ( -20.75514604977248112, 1.425000002731191984, 28.56700777964554661 ) ) ;
#22720 = CARTESIAN_POINT ( 'NONE',  ( 26.29305231718578995, 69.19999999999998863, -19.10302069950538240 ) ) ;
#22721 = CARTESIAN_POINT ( 'NONE',  ( -10.04305231718578462, 40.40000000000000568, 30.90933677959249337 ) ) ;
#22722 = CARTESIAN_POINT ( 'NONE',  ( -2.162160676586882350E-15, 46.62500000273119127, -35.31076352940722529 ) ) ;
#22723 = CARTESIAN_POINT ( 'NONE',  ( -23.41746824999999887, 1.624999997268811169, -2.867812753649727150E-15 ) ) ;
#22724 = CARTESIAN_POINT ( 'NONE',  ( 5.147494310547426899, 21.94874572391553968, -32.50000000000000000 ) ) ;
#22725 = VERTEX_POINT ( 'NONE', #15153 ) ;
#22726 = CARTESIAN_POINT ( 'NONE',  ( 20.75514604977249178, 62.07500000273118701, 28.56700777964553950 ) ) ;
#22727 = FACE_OUTER_BOUND ( 'NONE', #2991, .T. ) ;
#22728 = CARTESIAN_POINT ( 'NONE',  ( 18.94512977948576093, 12.82499999726882578, -13.76444248337722875 ) ) ;
#22729 = CARTESIAN_POINT ( 'NONE',  ( -24.22776226481240514, 33.34673583425730214, 13.94119854578937812 ) ) ;
#22730 = ORIENTED_EDGE ( 'NONE', *, *, #2433, .T. ) ;
#22731 = CARTESIAN_POINT ( 'NONE',  ( -27.16883889988623935, 33.32500000273118701, 19.73931689729374739 ) ) ;
#22732 = DIRECTION ( 'NONE',  ( -1.000000000000000000, 0.000000000000000000, 0.000000000000000000 ) ) ;
#22733 = VERTEX_POINT ( 'NONE', #27849 ) ;
#22734 = CARTESIAN_POINT ( 'NONE',  ( -5.147494310547430452, 36.05125428700922185, -32.49999999999999289 ) ) ;
#22735 = CARTESIAN_POINT ( 'NONE',  ( -2.162160676586881955E-15, 70.62500000273118417, -35.31076352940723240 ) ) ;
#22736 = CARTESIAN_POINT ( 'NONE',  ( -15.01150461594642138, 43.08072916666666430, -26.00068869287340334 ) ) ;
#22737 = CARTESIAN_POINT ( 'NONE',  ( -7.570916362186210335, 10.59999999999999787, -23.30088464923126779 ) ) ;
#22738 = CARTESIAN_POINT ( 'NONE',  ( 7.313012447739250820E-14, 17.24999999453762456, 24.50000000000000000 ) ) ;
#22739 = CARTESIAN_POINT ( 'NONE',  ( -20.75514604977248112, 11.42500000273116711, 28.56700777964554661 ) ) ;
#22740 = CARTESIAN_POINT ( 'NONE',  ( 14.97647472619900455, 52.52826416574268364, -26.02091320914876960 ) ) ;
#22741 = CARTESIAN_POINT ( 'NONE',  ( -9.657523855033125146E-16, 75.50000000000001421, -15.77193336357400710 ) ) ;
#22742 = CARTESIAN_POINT ( 'NONE',  ( -28.01184896238290278, 56.11458333333332860, 7.505752307973363457 ) ) ;
#22743 = CARTESIAN_POINT ( 'NONE',  ( 0.000000000000000000, 11.99999999999999645, 0.000000000000000000 ) ) ;
#22744 = DIRECTION ( 'NONE',  ( 0.000000000000000000, 1.000000000000000000, 0.000000000000000000 ) ) ;
#22745 = CARTESIAN_POINT ( 'NONE',  ( -24.50000000000000000, 4.749999994537623671, -3.000384657911015469E-15 ) ) ;
#22746 = CARTESIAN_POINT ( 'NONE',  ( -9.270509831248421762, 74.55000000546239391, 12.75976212528060039 ) ) ;
#22747 = CARTESIAN_POINT ( 'NONE',  ( 27.95245687107222921, 27.03906250000000000, -2.463307335887066074E-13 ) ) ;
#22748 = CARTESIAN_POINT ( 'NONE',  ( 27.16883889988624290, 35.92500000273118843, 19.73931689729373673 ) ) ;
#22749 = CARTESIAN_POINT ( 'NONE',  ( 10.37757302488624056, 78.52500000273120406, -31.93888565452638417 ) ) ;
#22750 = CARTESIAN_POINT ( 'NONE',  ( 10.37757302488624056, 42.77500000273119696, -31.93888565452638417 ) ) ;
#22751 = CARTESIAN_POINT ( 'NONE',  ( 20.75514604977248467, 20.67500000273119554, -28.56700777964554305 ) ) ;
#22752 = CARTESIAN_POINT ( 'NONE',  ( -7.570916362186210335, 16.34999999453762243, -23.30088464923126779 ) ) ;
#22753 = CARTESIAN_POINT ( 'NONE',  ( -26.29305231718578995, 8.700000005462394270, 19.10302069950538595 ) ) ;
#22754 = VECTOR ( 'NONE', #5187, 1000.000000000000227 ) ;
#22755 = CARTESIAN_POINT ( 'NONE',  ( 10.04305231718579705, 78.60000000000000853, 30.90933677959248982 ) ) ;
#22756 = CARTESIAN_POINT ( 'NONE',  ( 32.50000000000000000, 62.99999999999998579, -3.980102097228898626E-15 ) ) ;
#22757 = CARTESIAN_POINT ( 'NONE',  ( 23.41746824999999887, 12.52499999726880375, 7.608796670333735079 ) ) ;
#22758 = CARTESIAN_POINT ( 'NONE',  ( 25.98046417659831775, 28.75222249907602290, -15.04653450569338879 ) ) ;
#22759 = CARTESIAN_POINT ( 'NONE',  ( 23.41746825000000243, 5.224999997268802154, -7.608796670333727974 ) ) ;
#22760 = CARTESIAN_POINT ( 'NONE',  ( -13.94119854578892514, 33.62201416574269075, 24.22776226481266448 ) ) ;
#22761 = PRESENTATION_STYLE_ASSIGNMENT (( #22259 ) ) ;
#22762 = CARTESIAN_POINT ( 'NONE',  ( 6.486482029760648627E-15, 11.62500000273118950, 35.31076352940722529 ) ) ;
#22763 = CARTESIAN_POINT ( 'NONE',  ( -14.47279130897152122, 10.42499999726881299, 19.92008829642072243 ) ) ;
#22764 = CARTESIAN_POINT ( 'NONE',  ( 26.07999730980490227, 64.99479166666665719, 6.988114217767821046 ) ) ;
#22765 = EDGE_LOOP ( 'NONE', ( #28022, #10451, #14538, #15003 ) ) ;
#22766 = CARTESIAN_POINT ( 'NONE',  ( -33.58253175000000113, 49.02500000273116854, -10.91162601494193218 ) ) ;
#22767 = CARTESIAN_POINT ( 'NONE',  ( -33.58253175000000113, 23.27500000273116854, -10.91162601494193218 ) ) ;
#22768 = EDGE_LOOP ( 'NONE', ( #8978, #29469, #12517, #12390 ) ) ;
#22769 = CARTESIAN_POINT ( 'NONE',  ( 2.740863092043355209E-13, 34.77343750000000000, 30.02300923189239512 ) ) ;
#22770 = CARTESIAN_POINT ( 'NONE',  ( -28.02196122052045268, 33.48996500092397355, 7.468012846824790607 ) ) ;
#22771 = DIRECTION ( 'NONE',  ( 0.000000000000000000, 1.000000000000000000, 0.000000000000000000 ) ) ;
#22772 = CARTESIAN_POINT ( 'NONE',  ( -20.08610463437157989, 72.20000000546237118, -27.64615127144129758 ) ) ;
#22773 = CARTESIAN_POINT ( 'NONE',  ( 18.94512977948576093, 5.324999997268820451, -13.76444248337722875 ) ) ;
#22774 = EDGE_CURVE ( 'NONE', #3977, #15868, #16528, .T. ) ;
#22775 = CARTESIAN_POINT ( 'NONE',  ( -14.47279130897152122, 9.924999997268825425, 19.92008829642072243 ) ) ;
#22776 = CARTESIAN_POINT ( 'NONE',  ( -27.16883889988624290, 19.17500000273120264, -19.73931689729374028 ) ) ;
#22777 = CARTESIAN_POINT ( 'NONE',  ( 26.29305231718578995, 25.70000000546238184, -19.10302069950538240 ) ) ;
#22778 = CARTESIAN_POINT ( 'NONE',  ( 6.277390505771533514E-15, 64.50000000000000000, 34.17252228774368916 ) ) ;
#22779 = LINE ( 'NONE', #25529, #30219 ) ;
#22780 = CARTESIAN_POINT ( 'NONE',  ( 3.115048150918978465, 74.00000000000002842, 13.67161610608823530 ) ) ;
#22781 = CARTESIAN_POINT ( 'NONE',  ( 26.00068869287367335, 13.57552083333332682, 15.01150461594596308 ) ) ;
#22782 = CARTESIAN_POINT ( 'NONE',  ( -10.37757302488624411, 34.97500000273118559, -31.93888565452638417 ) ) ;
#22783 = CARTESIAN_POINT ( 'NONE',  ( 20.08610463437157279, 43.80000000546236549, -27.64615127144129758 ) ) ;
#22784 = CARTESIAN_POINT ( 'NONE',  ( -28.01184896238290278, 28.61458333333333215, 7.505752307973363457 ) ) ;
#22785 =( NAMED_UNIT ( * ) PLANE_ANGLE_UNIT ( ) SI_UNIT ( $, .RADIAN. ) );
#22786 = CARTESIAN_POINT ( 'NONE',  ( 18.94512977948575738, 16.92499999726882010, 13.76444248337723408 ) ) ;
#22787 = CARTESIAN_POINT ( 'NONE',  ( 20.08610463437158344, 8.699999999999986855, 27.64615127144129403 ) ) ;
#22788 = CARTESIAN_POINT ( 'NONE',  ( 20.08610463437157279, 9.800000005462367270, -27.64615127144129758 ) ) ;
#22789 = CARTESIAN_POINT ( 'NONE',  ( 24.18731323226221974, 49.37722249907602645, -14.01125832528328985 ) ) ;
#22790 = CARTESIAN_POINT ( 'NONE',  ( 27.16883889988623935, 54.32500000273118701, -19.73931689729374384 ) ) ;
#22791 = CARTESIAN_POINT ( 'NONE',  ( -20.75514604977248112, 59.67500000273118133, 28.56700777964554661 ) ) ;
#22792 = CARTESIAN_POINT ( 'NONE',  ( 33.58253175000000113, 40.47500000273117848, -10.91162601494193574 ) ) ;
#22793 = CARTESIAN_POINT ( 'NONE',  ( -7.236395654485757944, 15.22499999726881192, -22.27133577429736988 ) ) ;
#22794 = DIRECTION ( 'NONE',  ( -0.000000000000000000, -1.000000000000000000, -0.000000000000000000 ) ) ;
#22795 = CARTESIAN_POINT ( 'NONE',  ( -2.571758278209442450E-15, -1.999999999999998224, 0.000000000000000000 ) ) ;
#22796 = CARTESIAN_POINT ( 'NONE',  ( -24.18731323226248264, 44.23215250092398065, -14.01125832528284931 ) ) ;
#22797 = CARTESIAN_POINT ( 'NONE',  ( -20.49854233591107189, 16.99999999999998579, -12.98872394473008463 ) ) ;
#22798 = DIRECTION ( 'NONE',  ( -1.000000000000000000, -1.063101997391471025E-16, 0.000000000000000000 ) ) ;
#22799 = CARTESIAN_POINT ( 'NONE',  ( -20.75514604977248823, 24.82500000273117635, -28.56700777964554305 ) ) ;
#22800 = CARTESIAN_POINT ( 'NONE',  ( 10.04305231718578817, 67.40000000000001990, -30.90933677959249337 ) ) ;
#22801 = DIRECTION ( 'NONE',  ( 0.8660254037844387076, 0.000000000000000000, 0.5000000000000001110 ) ) ;
#22802 = CARTESIAN_POINT ( 'NONE',  ( 0.000000000000000000, 70.00000000000000000, 0.000000000000000000 ) ) ;
#22803 = CARTESIAN_POINT ( 'NONE',  ( -20.47846945139866648, 68.14024333240935505, 20.53372385742108008 ) ) ;
#22804 = CARTESIAN_POINT ( 'NONE',  ( 26.29305231718579350, 39.30000000546239391, 19.10302069950537529 ) ) ;
#22805 =( BOUNDED_CURVE ( )  B_SPLINE_CURVE ( 2, ( #17433, #25663, #27894, #14852, #25318, #2142, #12617 ),
 .UNSPECIFIED., .F., .T. ) 
 B_SPLINE_CURVE_WITH_KNOTS ( ( 3, 2, 2, 3 ),
 ( 0.3525641025641025883, 0.3538461538461538658, 0.3564102564102563653, 0.3589743589743589203 ),
 .UNSPECIFIED. ) 
 CURVE ( )  GEOMETRIC_REPRESENTATION_ITEM ( )  RATIONAL_B_SPLINE_CURVE ( ( 0.9755282581475768211, 0.9755282581475772652, 1.000000000000000000, 0.9510565162951535312, 1.000000000000000000, 0.9510565162951546414, 0.9999999999999988898 ) ) 
 REPRESENTATION_ITEM ( '' )  );
#22806 = CARTESIAN_POINT ( 'NONE',  ( 33.58253175000000113, 30.22500000273118559, -10.91162601494193574 ) ) ;
#22807 = CARTESIAN_POINT ( 'NONE',  ( -24.20753774853756823, 39.35677083333331439, -13.97622843553588723 ) ) ;
#22808 = ORIENTED_EDGE ( 'NONE', *, *, #24210, .T. ) ;
#22809 = CARTESIAN_POINT ( 'NONE',  ( -10.37757302488623701, 71.52500000273118985, 31.93888565452638417 ) ) ;
#22810 = CARTESIAN_POINT ( 'NONE',  ( 15.01150461594643204, 41.36197916666666430, 26.00068869287340334 ) ) ;
#22811 = FACE_OUTER_BOUND ( 'NONE', #1561, .T. ) ;
#22812 = ORIENTED_EDGE ( 'NONE', *, *, #18413, .T. ) ;
#22813 = CARTESIAN_POINT ( 'NONE',  ( 15.04653450569292872, 55.40402750092397355, -25.98046417659857710 ) ) ;
#22814 = CARTESIAN_POINT ( 'NONE',  ( -26.09010956794232428, 60.98996500092398065, 6.950374756619732253 ) ) ;
#22815 = CARTESIAN_POINT ( 'NONE',  ( -20.75514604977248823, 10.82500000273118701, -28.56700777964554305 ) ) ;
#22816 = CARTESIAN_POINT ( 'NONE',  ( -20.53372385742107653, 13.99961833240935327, -20.47846945139867003 ) ) ;
#22817 = DIRECTION ( 'NONE',  ( 0.000000000000000000, -1.000000000000000000, 0.000000000000000000 ) ) ;
#22818 = CARTESIAN_POINT ( 'NONE',  ( -27.16883889988623935, 41.57500000273117990, 19.73931689729374739 ) ) ;
#22819 = CARTESIAN_POINT ( 'NONE',  ( -10.04305231718579172, 42.10000000546237686, -30.90933677959248982 ) ) ;
#22820 = CARTESIAN_POINT ( 'NONE',  ( -4.635254915624208216, 74.40000000000001990, 14.26584774442730463 ) ) ;
#22821 = CARTESIAN_POINT ( 'NONE',  ( -2.162160676586881955E-15, 26.62500000273118417, -35.31076352940723240 ) ) ;
#22822 = CARTESIAN_POINT ( 'NONE',  ( 15.14183272437242422, 14.04999999453763593, -20.84094480462497856 ) ) ;
#22823 = CARTESIAN_POINT ( 'NONE',  ( 6.486482029760649416E-15, 53.87500000273118417, 35.31076352940723240 ) ) ;
#22824 = CARTESIAN_POINT ( 'NONE',  ( 10.04305231718578817, 29.39999999999999503, -30.90933677959249337 ) ) ;
#22825 = CARTESIAN_POINT ( 'NONE',  ( -32.50000000000000000, 35.90000000000000568, -10.55989012756945478 ) ) ;
#22826 = CARTESIAN_POINT ( 'NONE',  ( 23.41746824999999887, 18.62499999726882649, 0.000000000000000000 ) ) ;
#22827 = CARTESIAN_POINT ( 'NONE',  ( -20.75514604977248112, 77.42500000273119554, 28.56700777964554661 ) ) ;
#22828 = DIRECTION ( 'NONE',  ( 1.000000000000000000, 1.309225264888156377E-16, 0.000000000000000000 ) ) ;
#22829 = DIRECTION ( 'NONE',  ( 0.000000000000000000, 0.000000000000000000, 1.000000000000000000 ) ) ;
#22830 = CARTESIAN_POINT ( 'NONE',  ( -20.75514604977248823, 65.07500000273118701, -28.56700777964554305 ) ) ;
#22831 = CARTESIAN_POINT ( 'NONE',  ( -4.635254915624208216, 78.65000000546234560, 14.26584774442730463 ) ) ;
#22832 = PLANE ( 'NONE',  #11724 ) ;
#22833 = CARTESIAN_POINT ( 'NONE',  ( 6.486482029760649416E-15, 15.62500000273117884, 35.31076352940723240 ) ) ;
#22834 = CARTESIAN_POINT ( 'NONE',  ( 24.50000000000000355, 7.849999994537626868, -7.960532557706203605 ) ) ;
#22835 = CARTESIAN_POINT ( 'NONE',  ( 26.09010956794232428, 18.02121500092397710, -6.950374756619718042 ) ) ;
#22836 = CARTESIAN_POINT ( 'NONE',  ( -32.50000000000000000, 25.89999999999999147, -10.55989012756945300 ) ) ;
#22837 = CARTESIAN_POINT ( 'NONE',  ( 33.58253175000000113, 44.22500000273117138, -10.91162601494193751 ) ) ;
#22838 = CARTESIAN_POINT ( 'NONE',  ( -20.75514604977248112, 7.675000002731199089, 28.56700777964554661 ) ) ;
#22839 = CARTESIAN_POINT ( 'NONE',  ( -10.37757302488623701, 55.77500000273121117, 31.93888565452638417 ) ) ;
#22840 = CARTESIAN_POINT ( 'NONE',  ( -20.47846945139902175, 51.25038166759065206, -20.53372385742072481 ) ) ;
#22841 = CARTESIAN_POINT ( 'NONE',  ( -4.934616302121927505E-14, 69.00000000546238255, 32.50000000000000000 ) ) ;
#22842 = AXIS2_PLACEMENT_3D ( 'NONE', #19217, #19383, #27433 ) ;
#22843 = CARTESIAN_POINT ( 'NONE',  ( -14.97647472619899389, 33.62201416574269075, 26.02091320914878025 ) ) ;
#22844 =( BOUNDED_CURVE ( )  B_SPLINE_CURVE ( 2, ( #65, #10551, #21032, #20701, #31482, #31308, #8142 ),
 .UNSPECIFIED., .F., .T. ) 
 B_SPLINE_CURVE_WITH_KNOTS ( ( 3, 2, 2, 3 ),
 ( 0.000000000000000000, 0.02000000000000000042, 0.04000000000000000083, 0.05000000000000000971 ),
 .UNSPECIFIED. ) 
 CURVE ( )  GEOMETRIC_REPRESENTATION_ITEM ( )  RATIONAL_B_SPLINE_CURVE ( ( 1.000000000000000000, 0.9510565162951535312, 1.000000000000000000, 0.9510565162951535312, 1.000000000000000000, 0.9755282581475768211, 0.9755282581475768211 ) ) 
 REPRESENTATION_ITEM ( '' )  );
#22845 = CARTESIAN_POINT ( 'NONE',  ( -32.50000000000000000, 62.50000000546239676, 0.000000000000000000 ) ) ;
#22846 = CARTESIAN_POINT ( 'NONE',  ( -13.91746824999999532, 81.27500000273117564, -4.522059556121115875 ) ) ;
#22847 = CARTESIAN_POINT ( 'NONE',  ( -7.025853678916861966, 62.41107666574269075, -26.06988505166722803 ) ) ;
#22848 = CARTESIAN_POINT ( 'NONE',  ( -7.236395654485757944, 1.724999997268800156, -22.27133577429736988 ) ) ;
#22849 = CONICAL_SURFACE ( 'NONE', #27231, 12.11607355459420354, 0.8042044335707554392 ) ;
#22850 = CARTESIAN_POINT ( 'NONE',  ( 20.08610463437158344, 75.20000000546241381, 27.64615127144129403 ) ) ;
#22851 = CARTESIAN_POINT ( 'NONE',  ( -2.584737979205441561E-13, 15.86718749999999645, -30.02300923189239512 ) ) ;
#22852 = CARTESIAN_POINT ( 'NONE',  ( -2.162160676586881955E-15, 34.87500000273117706, -35.31076352940723240 ) ) ;
#22853 = CARTESIAN_POINT ( 'NONE',  ( -23.41746824999999887, 6.024999997268805529, -7.608796670333730638 ) ) ;
#22854 = ORIENTED_EDGE ( 'NONE', *, *, #3804, .T. ) ;
#22855 = CARTESIAN_POINT ( 'NONE',  ( 10.37757302488624056, 72.77500000273118985, -31.93888565452638417 ) ) ;
#22856 = CARTESIAN_POINT ( 'NONE',  ( -26.29305231718578995, 24.70000000546239249, 19.10302069950538595 ) ) ;
#22857 = CARTESIAN_POINT ( 'NONE',  ( 15.01150461594643204, 41.36197916666666430, 26.00068869287340334 ) ) ;
#22858 = CARTESIAN_POINT ( 'NONE',  ( -26.29305231718579350, 64.30000000546237970, -19.10302069950537884 ) ) ;
#22860 = ORIENTED_EDGE ( 'NONE', *, *, #18514, .T. ) ;
#22859 = EDGE_CURVE ( 'NONE', #19899, #23926, #28315, .T. ) ;
#22861 = CARTESIAN_POINT ( 'NONE',  ( -26.29305231718579350, 10.30000000546238326, -19.10302069950537884 ) ) ;
#22862 = CARTESIAN_POINT ( 'NONE',  ( -20.75514604977248112, 49.42500000273118133, 28.56700777964554661 ) ) ;
#22863 = CARTESIAN_POINT ( 'NONE',  ( -18.94512977948575738, 15.42499999726881832, -13.76444248337723231 ) ) ;
#22864 = ADVANCED_FACE ( 'NONE', ( #17557 ), #31819, .T. ) ;
#22865 = CARTESIAN_POINT ( 'NONE',  ( -2.092463501923844636E-15, 6.000000005462371888, -34.17252228774368916 ) ) ;
#22866 = CARTESIAN_POINT ( 'NONE',  ( -5.147494310547423346, 8.448745718453160691, 32.50000000000000000 ) ) ;
#22867 = CARTESIAN_POINT ( 'NONE',  ( 7.505752307972854531, 16.01041666666666075, -28.01184896238303423 ) ) ;
#22868 = CARTESIAN_POINT ( 'NONE',  ( 32.50000000000000000, 54.99999999999999289, -3.980102097228898626E-15 ) ) ;
#22869 = DIRECTION ( 'NONE',  ( -1.224646799147353207E-16, -1.499759782661857882E-32, 1.000000000000000000 ) ) ;
#22870 = CARTESIAN_POINT ( 'NONE',  ( 10.37757302488624767, 19.97500000273119625, 31.93888565452638417 ) ) ;
#22871 = CARTESIAN_POINT ( 'NONE',  ( -19.82091636218621389, 7.200000000000011724, 14.40073868116558842 ) ) ;
#22872 = CARTESIAN_POINT ( 'NONE',  ( 19.11951029504797006, 22.59336833240935505, 19.06425588902558133 ) ) ;
#22873 = CARTESIAN_POINT ( 'NONE',  ( -4.300734207923759378, 76.97500000273119269, -13.23629886949340495 ) ) ;
#22874 = CARTESIAN_POINT ( 'NONE',  ( -20.08610463437157989, 55.69999999999998863, -27.64615127144129758 ) ) ;
#22875 = CARTESIAN_POINT ( 'NONE',  ( 10.04305231718579705, 53.10000000546239107, 30.90933677959248982 ) ) ;
#22876 = AXIS2_PLACEMENT_3D ( 'NONE', #18905, #15829, #29352 ) ;
#22877 = CARTESIAN_POINT ( 'NONE',  ( -10.04305231718579172, 3.599999999999992095, -30.90933677959248982 ) ) ;
#22878 = VERTEX_POINT ( 'NONE', #25017 ) ;
#22879 = CARTESIAN_POINT ( 'NONE',  ( 1.507698388325705758E-15, 15.62499999726882116, -24.62258325217400312 ) ) ;
#22880 = CARTESIAN_POINT ( 'NONE',  ( 2.067204126564591252E-14, 6.249999994537622783, -24.50000000000000000 ) ) ;
#22881 = CARTESIAN_POINT ( 'NONE',  ( -2.428612866367529427E-13, 50.24218750000000711, -27.95245687107222921 ) ) ;
#22882 = CARTESIAN_POINT ( 'NONE',  ( 10.37757302488624056, 60.52500000273118275, -31.93888565452638417 ) ) ;
#22883 = CARTESIAN_POINT ( 'NONE',  ( -20.75514604977248823, 21.07500000273118346, -28.56700777964554305 ) ) ;
#22884 = CARTESIAN_POINT ( 'NONE',  ( -33.58253175000000113, 13.27500000273118097, -10.91162601494193218 ) ) ;
#22885 = CARTESIAN_POINT ( 'NONE',  ( 6.988114217767829928, 29.76041666666666430, -26.07999730980489872 ) ) ;
#22886 = CARTESIAN_POINT ( 'NONE',  ( -20.75514604977248823, 5.075000002731193227, -28.56700777964554305 ) ) ;
#22887 = CARTESIAN_POINT ( 'NONE',  ( -14.97647472619946285, 23.89361083425731280, -26.02091320914851025 ) ) ;
#22888 = CARTESIAN_POINT ( 'NONE',  ( -26.00068869287368756, 59.98177083333332149, -15.01150461594595775 ) ) ;
#22889 = CARTESIAN_POINT ( 'NONE',  ( 27.16883889988623935, 4.325000002731186122, -19.73931689729374384 ) ) ;
#22890 = CARTESIAN_POINT ( 'NONE',  ( -11.25946833292375793, 73.17500000273119554, -8.180482586598733619 ) ) ;
#22891 = CARTESIAN_POINT ( 'NONE',  ( -32.50000000000000000, 41.99999999999999289, 0.000000000000000000 ) ) ;
#22892 = CARTESIAN_POINT ( 'NONE',  ( 20.75514604977248467, 44.42500000273120264, -28.56700777964554305 ) ) ;
#22893 = CARTESIAN_POINT ( 'NONE',  ( -4.523095164977116484E-15, 4.124999997268806951, 24.62258325217400312 ) ) ;
#22894 = DIRECTION ( 'NONE',  ( 0.000000000000000000, 1.000000000000000000, 0.000000000000000000 ) ) ;
#22895 = ORIENTED_EDGE ( 'NONE', *, *, #6221, .T. ) ;
#22896 = CARTESIAN_POINT ( 'NONE',  ( -27.16883889988624290, 51.17500000273118843, -19.73931689729374028 ) ) ;
#22897 = CARTESIAN_POINT ( 'NONE',  ( 32.50000000000000000, 43.10000000000000853, -10.55989012756945833 ) ) ;
#22898 = CARTESIAN_POINT ( 'NONE',  ( -7.025853678916393008, 32.91704833425729504, 26.06988505166735592 ) ) ;
#22899 = CARTESIAN_POINT ( 'NONE',  ( -20.75514604977248112, 77.67500000273119554, 28.56700777964554661 ) ) ;
#22900 = ORIENTED_EDGE ( 'NONE', *, *, #24875, .T. ) ;
#22901 = CARTESIAN_POINT ( 'NONE',  ( 27.16883889988623935, 32.32500000273117990, -19.73931689729374384 ) ) ;
#22902 = CARTESIAN_POINT ( 'NONE',  ( 30.02300923189239512, 16.72656249999999645, -2.619432448724977703E-13 ) ) ;
#22903 = VECTOR ( 'NONE', #22517, 1000.000000000000000 ) ;
#22904 = EDGE_CURVE ( 'NONE', #17164, #28702, #12139, .T. ) ;
#22905 = ORIENTED_EDGE ( 'NONE', *, *, #20393, .F. ) ;
#22906 = DIRECTION ( 'NONE',  ( 0.000000000000000000, 0.000000000000000000, -1.000000000000000000 ) ) ;
#22907 = CARTESIAN_POINT ( 'NONE',  ( -10.37757302488623701, 65.52500000273120406, 31.93888565452638417 ) ) ;
#22908 = CARTESIAN_POINT ( 'NONE',  ( 20.50609665441005092, 41.21875000000000000, 20.50609665440969209 ) ) ;
#22909 =( BOUNDED_SURFACE ( )  B_SPLINE_SURFACE ( 3, 2, ( 
 ( #4879, #15870, #15704, #26159, #28552, #25650, #10210, #20852, #7277, #2653, #10374, #12604, #18449, #25815, #31298, #23073, #2128, #33534, #5050, #23251, #33713, #20691, #12434, #31132, #20334, #10038, #5393, #7624, #15186, #9857, #20512, #18104, #30958, #22902, #28726, #30784, #13115, #17760, #21020, #31471, #15534, #25986, #7962, #1959, #23589, #18281, #2479, #28218, #12778, #15360, #12947, #23420, #7790, #54, #10542, #4705, #7456, #17940, #2305, #3160, #8791, #26986, #31800, #21190, #11376, #5561, #3323, #16209, #8461, #13631, #18950, #24095, #31632, #10710, #29395, #23758, #13791, #16040, #5895, #24259, #21852, #729, #26496, #32134, #8629, #19112, #16374, #26663, #11054, #2990, #563, #10882, #26827, #895, #32297, #21357, #13955, #11214, #29551, #21518, #19275, #21687, #16534, #3486, #26327, #13459, #29716, #29056, #8291, #222, #23928, #6051, #397, #6222, #5731, #24418, #2815, #18781, #13282, #8130, #18619, #29226, #31968, #32461, #3649, #30054, #22686, #25258, #11533, #25083, #30566, #30222, #11701, #14456, #16702, #17033, #4152, #1733, #12213, #19945, #1053, #33136, #1220, #6390, #24912, #32794, #9287, #22184, #3816, #6722, #3982, #1562, #30390, #8961, #14625, #19771, #6558, #17204, #4320, #27663, #14125, #9639, #24582, #14288, #12038, #22508, #32960, #22347, #27493, #9462, #19444, #11874, #24745, #6892, #17373, #22016, #27836, #16867, #29889, #20122, #14794, #32631, #27157, #27328, #9125, #19607, #1398, #15143, #23376, #2257, #18235, #23202, #33664, #17717, #10334, #15662, #4663, #12388, #20810, #28176, #25607, #5003, #2086, #12561, #23032, #22857, #20463, #28506, #26111, #25435, #31254, #4491, #12731, #13070, #33489, #15486, #7408, #20291, #7746, #8, #15312, #17546, #30914, #25940, #9991, #30739, #4832, #10161, #20643, #17894, #28347, #31086, #25771, #2434, #28681, #33315, #12901, #7583, #18061, #33837, #5179, #2609, #14967, #23546, #1911, #10497, #20975, #7063, #28005, #9814, #7231, #11006, #13237, #26620, #29015, #3116, #13745, #28848, #31923, #31588, #23711, #26944, #11173, #15996, #8586, #26786, #21644, #29351, #5687, #5515, #24216, #13588, #19070, #24051, #519, #8087, #687, #6014, #26452, #2773, #32090, #18574, #2943, #5851, #13414, #23882, #353, #177, #10837, #18904, #16489, #15828, #29510, #5347, #21476, #3444, #21315, #16330, #31756, #10667, #13914, #24381, #16165, #7918, #8247, #3278, #18740, #8415, #854, #11334, #31425, #18403, #26282, #21146, #29182, #11495, #25217, #24541, #6351, #19235, #8919, #9250, #19402, #1695, #1182, #24871, #25045, #14248, #14585, #29673, #11833, #21810, #27285, #3610, #8751, #11663, #27796, #30352, #16660, #30180, #32258, #1354, #16830, #19570, #6178, #22145, #19735, #6854, #17332, #1526, #27117, #4280, #3777, #30018, #22311, #9088, #14083, #1012, #21974, #27452, #32589, #14754, #22471, #24705, #32422, #29851, #6522, #32756, #16994, #3943, #14418, #6683, #17168, #27624, #4111, #12000, #32919, #9418, #19903, #20422, #28304, #15444, #4792, #14926, #2211 ),
 ( #22816, #7367, #23159, #2046, #4966, #30871, #20602, #31047, #12171, #25392, #23338, #4448, #9770, #9599, #33275, #15271, #20253, #22644, #4622, #17851, #7540, #17674, #10121, #30524, #25732, #33096, #28136, #1869, #7022, #25566, #20081, #17504, #12347, #18025, #27966, #25899, #12690, #28471, #30696, #33622, #7192, #15101, #12521, #22989, #2392, #33448, #12861, #9946, #6627, #24986, #1469, #3886, #29961, #32862, #30124, #17273, #22582, #1123, #6794, #11945, #22256, #9359, #30465, #22414, #6295, #17448, #16771, #6466, #19840, #27736, #4224, #14526, #19678, #30293, #24649, #4051, #16940, #14698, #25156, #27230, #1632, #9034, #11608, #17106, #3724, #12110, #14865, #1294, #33033, #9193, #22090, #9537, #1808, #27565, #19349, #32699, #20019, #27397, #6963, #27909, #4391, #25330, #12284, #22758, #8864, #29791, #32534, #14194, #19513, #14359, #24817, #11776, #31521, #23470, #18669, #21242, #5948, #13339, #614, #7842, #277, #3043, #104, #12999, #31851, #13163, #29107, #13681, #23812, #15923, #26879, #26717, #3213, #5612, #2703, #31685, #8344, #18331, #24145, #21406, #23640, #29445, #2870, #18833, #10595, #21072, #8015, #16096, #10764, #8179, #26547, #33932, #13515, #31349, #18500, #16427, #23978, #26209, #20901, #28944, #449, #5442, #10423, #5780, #28776, #16260, #5273, #32019, #8515, #10931, #29279, #19001, #15755, #11104, #21573, #26379, #21743, #9014, #14009, #946, #24633, #1106, #16920, #11590, #785, #32189, #24311, #19496, #14176, #19824, #4034, #8846, #8683, #22399, #16587, #14341, #27213, #29944, #22070, #6448, #32514, #19167, #29605, #27380, #11267, #24799, #27043, #3869, #1276, #32847, #11756, #3537, #9339, #30276, #22237, #32682, #6776, #17257, #17087, #19661, #9177, #6106, #30104, #24471, #11426, #6610, #27547, #14509, #24968, #21901, #32353, #19328, #1450, #11929, #3374, #13845, #29770, #6278, #16754, #3704, #4715, #17596, #9866, #4545, #20343, #15020, #22562, #12093, #30793, #25139, #15195, #17429, #7286, #25659, #23260, #2138, #27890, #33543, #10045, #20524, #17770, #28058, #12444, #4374, #25490, #12264, #28229, #2314, #12787, #22740, #15369, #7114, #12613, #14678, #27718, #30448, #1615, #33014, #9519, #1969, #22914, #14848, #23082, #20001, #4206, #33191, #6946, #33370, #30968, #20700, #7467, #25824, #25314, #17950, #28399, #1787, #9694, #4888, #20174, #33723, #10221, #31142, #30618, #7633, #31810, #8301, #10721, #7801, #26337, #3000, #23431, #18793, #26507, #28735, #573, #7971, #13473, #5231, #18290, #15715, #21199, #5403, #15880, #2826, #28563, #13295, #2488, #26170, #11064, #23768, #31307, #25995, #2663, #235, #13123, #5058, #10893, #12957, #21366, #33891, #23598, #31643, #18115, #18458, #5571, #26676, #13641, #29237, #10383, #3171, #63, #10550, #8141, #18630, #29066, #21031, #31481, #16053, #23938, #407, #5741, #20861, #16221, #24105, #28902, #21529, #31977, #15543, #5907, #17045, #16384, #29561, #1066, #6404, #27341, #14136, #19285, #22028, #24271, #3661, #6062, #24593, #24757, #26837, #8973 ),
 ( #1235, #11546, #19619, #32472, #19455, #19124, #11713, #27506, #16545, #13803, #22196, #26998, #3496, #16878, #13965, #24429, #905, #738, #21863, #29902, #3995, #3332, #32643, #11224, #3827, #14468, #11386, #14301, #8803, #21700, #9138, #1410, #16714, #18961, #32310, #30065, #29728, #6571, #24925, #27168, #11887, #22359, #8474, #29405, #32145, #8639, #6233, #1576, #17387, #17732, #25621, #22523, #28189, #2274, #12226, #1925, #2101, #25273, #12574, #6736, #22872, #12748, #4335, #14639, #19783, #22699, #4849, #7423, #27677, #7244, #32806, #12402, #14808, #4167, #17909, #12053, #9827, #33151, #14979, #9655, #25449, #20135, #25099, #17218, #33330, #30232, #20303, #32974, #30754, #4677, #28362, #15156, #9478, #23045, #33503, #10007, #20479, #30580, #17560, #19960, #7076, #27852, #30930, #15330, #25785, #1746, #9299, #28017, #30408, #6907, #4505, #25956, #10179, #7597, #18075, #31441, #7933, #12916, #26299, #28524, #23221, #7764, #33680, #28865, #18421, #16633, #23561, #10854, #5019, #10514, #13254, #10348, #20661, #8102, #23392, #5362, #23897, #25, #26127, #3583, #2960, #13429, #15842, #33854, #2788, #18589, #15502, #368, #31604, #20826, #6148, #13087, #29029, #31270, #18250, #28697, #23728, #20992, #194, #10681, #31101, #21162, #2450, #5194, #27089, #5532, #15678, #2624, #16013, #26467, #21329, #31770, #8725, #19208, #29646, #21946, #33066, #9571, #9223, #19707, #20048, #6995, #27767, #30326, #27593, #32397, #30153, #24680, #11636, #1326, #11807, #4084, #22285, #11472, #8892, #987, #6657, #24846, #30494, #14727, #19376, #1154, #17140, #11974, #32890, #14558, #32730, #25018, #29822, #1498, #22120, #22443, #6822, #6326, #9389, #19873, #14055, #3917, #17477, #32563, #25188, #17304, #4252, #1665, #12140, #9062, #22613, #27939, #24517, #16802, #27259, #19543, #3750, #14224, #29991, #6495, #16968, #27426, #14389, #2362, #2017, #12492, #22961, #20226, #17821, #25871, #23479, #22789, #18167, #1839, #10094, #10432, #30845, #12836, #4764, #17646, #7681, #31358, #12659, #14897, #28277, #23310, #33419, #28444, #31191, #23128, #33940, #17999, #28609, #5109, #4422, #28107, #7850, #7164, #9917, #33775, #15593, #4594, #10266, #18338, #15242, #7514, #26047, #7336, #2540, #12319, #4935, #25361, #20394, #30666, #33242, #25704, #20907, #13007, #9740, #20748, #15071, #15417, #2185, #33594, #25538, #20573, #31016, #3380, #24316, #32025, #13171, #13851, #13346, #18508, #26555, #10939, #21414, #23819, #15931, #18839, #16104, #3218, #8522, #21080, #26722, #31857, #8187, #29285, #16432, #8349, #26218, #790, #28954, #3051, #13686, #111, #19006, #24150, #5450, #11273, #18677, #621, #26387, #2879, #285, #5785, #13522, #23985, #457, #5281, #16266, #23649, #10773, #21749, #11109, #8022, #2710, #21250, #21579, #31694, #15764, #29450, #10602, #5952, #31528, #32194, #8688, #26884, #28783, #29116, #5620, #32852, #1456, #32688, #3542, #24805, #29777, #16759, #6454, #16928, #9183, #27386, #16592, #14014, #6111, #1283, #29950, #1622, #19830 ),
 ( #24477, #11762, #27049, #30112, #8852, #22243, #6616, #14685, #17094, #19333, #24974, #11935, #22404, #19667, #19502, #3875, #6283, #14348, #3711, #27553, #27725, #4213, #14181, #6784, #32521, #4041, #951, #19172, #21907, #11431, #32358, #27218, #14515, #9347, #24637, #30282, #1111, #29609, #11596, #22076, #17262, #25146, #12100, #22571, #33021, #9020, #30800, #33550, #30625, #9527, #28406, #9701, #15202, #10228, #9872, #12451, #23439, #23268, #33730, #2145, #7121, #4722, #25831, #6952, #10051, #7293, #20008, #33377, #15551, #28065, #20708, #4896, #31150, #7475, #17778, #17603, #2321, #25666, #7641, #12620, #23087, #20181, #12794, #18125, #4552, #14855, #28570, #15031, #25496, #17957, #1976, #22921, #20350, #25321, #28236, #30975, #5066, #27897, #26003, #17436, #20532, #2496, #15376, #12965, #30455, #22747, #4380, #1795, #12273, #33198, #23778, #8309, #31489, #23946, #26683, #8149, #18968, #13481, #24112, #580, #33900, #23605, #3339, #2672, #18465, #18800, #3179, #72, #29244, #13810, #13303, #3009, #13648, #26345, #11070, #7809, #415, #10391, #5410, #15723, #20869, #244, #5914, #8481, #28743, #5748, #31317, #10901, #28909, #31651, #18298, #10730, #21374, #29412, #16391, #21536, #5239, #26844, #15889, #10560, #18638, #16060, #26515, #2834, #21039, #31818, #21207, #16229, #31984, #26178, #13131, #7979, #29075, #5579, #11896, #3835, #21707, #32814, #32153, #11392, #16886, #22204, #9145, #29911, #1074, #14310, #6069, #19463, #8646, #19131, #32480, #8981, #13973, #27349, #29568, #24278, #8810, #746, #6414, #24765, #17225, #24600, #22367, #16552, #11554, #1243, #21869, #11231, #19628, #24436, #11721, #24933, #22036, #27177, #4175, #4003, #14476, #32651, #913, #30073, #6579, #27005, #1418, #17054, #32319, #6745, #14144, #27515, #19293, #29736, #6241, #9307, #19792, #30240, #27685, #3503, #16722, #3670, #4342, #31110, #9835, #27860, #22532, #1754, #20312, #12234, #25108, #7431, #32982, #17918, #9486, #33689, #10187, #30762, #7252, #20670, #7604, #28370, #30938, #28198, #19969, #17739, #25282, #22709, #1933, #12411, #4685, #22881, #12061, #30415, #1584, #15164, #25458, #18084, #15338, #20144, #6914, #28532, #14816, #25630, #4513, #2109, #33338, #12582, #23052, #17396, #33160, #33511, #9663, #10016, #30588, #20487, #4858, #14649, #25793, #7084, #2282, #12757, #23229, #17568, #14987, #28026, #28704, #2795, #23568, #21169, #13610, #24075, #32, #26642, #18428, #13438, #25964, #5027, #7771, #2458, #26135, #5202, #2632, #8109, #26306, #13261, #23737, #15512, #201, #23401, #15685, #21497, #10688, #18258, #12924, #13094, #31612, #10522, #33861, #31777, #10355, #8269, #20833, #540, #11028, #18596, #29036, #31945, #8437, #18761, #21336, #5539, #31278, #16020, #20999, #31448, #26474, #2968, #23904, #376, #7941, #28873, #5369, #10862, #15850, #18927, #5710, #29205, #16189, #3137, #8608, #6371, #19253, #11514, #6199, #21994, #16679, #24236, #13766, #32442, #26806, #16849, #19091, #8943, #27306, #24891, #3796, #29529, #1201 ),
 ( #26963, #19421, #22166, #3630, #14436, #29871, #19588, #30036, #29373, #6032, #32775, #32108, #13934, #14269, #32609, #16511, #24726, #9269, #8770, #11682, #9107, #21832, #6541, #3301, #17013, #5872, #873, #11193, #16351, #29693, #1377, #3962, #707, #27474, #21664, #11851, #24398, #27136, #3464, #14104, #22330, #11353, #32277, #24560, #1034, #4812, #4299, #30546, #12367, #7042, #14607, #4132, #1890, #17186, #30718, #9438, #22835, #7213, #15291, #17696, #19925, #25585, #2065, #12541, #33295, #20100, #4472, #30371, #17525, #14774, #9795, #28323, #25751, #25239, #7388, #33116, #28156, #6703, #19753, #22489, #27644, #25063, #1544, #27985, #14946, #6872, #20271, #12020, #30201, #1714, #32940, #25412, #4642, #12710, #15121, #17872, #17352, #23012, #33467, #27815, #12192, #9967, #22663, #20442, #30893, #2235, #9619, #33644, #23181, #331, #2750, #33818, #18382, #28995, #15466, #10817, #18550, #20790, #26600, #33983, #5495, #31235, #10312, #7727, #13214, #31404, #7898, #28828, #20623, #5326, #28488, #18215, #3097, #15806, #23357, #18044, #28659, #26262, #5155, #31065, #2923, #4985, #13392, #25919, #29158, #5664, #23691, #156, #16147, #13568, #23864, #26430, #10647, #2414, #21124, #15640, #26091, #31567, #8065, #15974, #21297, #7559, #12881, #2588, #31737, #20955, #24031, #8228, #13052, #23524, #10141, #10477, #18722, #24362, #16641, #3923, #5994, #16311, #21457, #13895, #6501, #9069, #29330, #8898, #14397, #14061, #29490, #32239, #500, #832, #21953, #19549, #29997, #3756, #18881, #16974, #19051, #24195, #8732, #27095, #3588, #16470, #21624, #24523, #21791, #19382, #14230, #26767, #32402, #993, #11312, #11478, #22126, #29830, #31900, #27432, #8395, #32067, #6332, #16809, #27265, #6155, #19216, #24686, #3258, #29652, #8567, #1161, #11642, #5832, #32569, #10984, #13728, #665, #11153, #26925, #3423, #20233, #15557, #22796, #33073, #32896, #7171, #20057, #2503, #7002, #17484, #1504, #28577, #33906, #22449, #30159, #5073, #11981, #9395, #33251, #19879, #30332, #6829, #6664, #4259, #12326, #10397, #9229, #26011, #22291, #30501, #31324, #17311, #9747, #25194, #4090, #12971, #18304, #9579, #1332, #14733, #30673, #27773, #14904, #18133, #27946, #20876, #4429, #23445, #7815, #24852, #14565, #28749, #27599, #1672, #5247, #11815, #25024, #32736, #19713, #12147, #25368, #17146, #22620, #1846, #23611, #5753, #26688, #5416, #21541, #31990, #8486, #29249, #16065, #420, #15895, #13486, #251, #31824, #24284, #753, #10736, #3347, #29080, #24118, #2679, #15729, #18472, #13137, #80, #10567, #23951, #10907, #26351, #18805, #21045, #26183, #21213, #31495, #21379, #8315, #8652, #26520, #13817, #7985, #3014, #16234, #2841, #28915, #585, #13310, #3184, #16397, #13653, #18643, #29574, #29418, #5920, #11076, #23784, #18973, #26850, #31658, #11237, #21713, #8154, #32159, #5585, #19137, #27183, #6248, #3676, #9151, #27355, #3840, #14315, #16559, #24770, #24442, #29743, #22537, #1248, #19299, #13979, #14150, #11727, #24606, #27012, #32820 ),
 ( #19633, #919, #22209, #16728, #1080, #32656, #30078, #6584, #17059, #3509, #11398, #21875, #27521, #16892, #32987, #6750, #11560, #32325, #25114, #22042, #4008, #29918, #14482, #24938, #1423, #11901, #8816, #32486, #22373, #8988, #9312, #19469, #19797, #30245, #1589, #6420, #17230, #12066, #27690, #4180, #14654, #9491, #19974, #6075, #7257, #25287, #14822, #12587, #27865, #7440, #20149, #33517, #17924, #25970, #28375, #30593, #2288, #12762, #23235, #10021, #30768, #15169, #7089, #28204, #14994, #23057, #5033, #15518, #25464, #18090, #9841, #4863, #17401, #30420, #33165, #4347, #1759, #12239, #4690, #25635, #17573, #20493, #22715, #6919, #1939, #9668, #2114, #30943, #23406, #17744, #28537, #28031, #15344, #25798, #4519, #12417, #33694, #22887, #10196, #31116, #20676, #33344, #10360, #7609, #2463, #12929, #20319, #33867, #5716, #26140, #11033, #29210, #31453, #3308, #10694, #16194, #7946, #21004, #18434, #23910, #8114, #18601, #29041, #31283, #5544, #5207, #10527, #13772, #16025, #38, #28709, #28878, #26480, #5375, #7776, #13615, #15691, #24080, #2637, #5879, #16357, #2974, #13443, #26812, #24242, #546, #3142, #381, #13100, #10867, #15855, #26311, #21341, #31782, #8274, #18766, #18263, #23573, #2800, #26648, #31617, #713, #21502, #8443, #31950, #13267, #29380, #23742, #206, #18934, #20838, #21175, #16855, #22000, #24732, #26969, #6377, #8776, #27313, #27480, #8614, #11688, #8949, #11199, #1040, #17192, #29701, #22336, #6547, #1383, #9113, #19427, #19259, #3969, #3803, #32781, #14275, #1207, #21838, #14442, #19759, #6205, #16517, #24898, #32283, #16685, #19594, #27142, #3636, #14110, #3470, #24567, #32616, #30208, #29535, #11857, #19097, #22172, #27650, #11520, #30042, #32448, #24404, #9275, #4138, #29877, #21670, #17020, #6710, #14613, #25069, #32117, #6038, #13940, #880, #11360, #20448, #1550, #14779, #12715, #27821, #33121, #25590, #23017, #25244, #2070, #12026, #27990, #30723, #9972, #7047, #33472, #19930, #17701, #22495, #17529, #4304, #9446, #4477, #32945, #30376, #1719, #30898, #6877, #12546, #14952, #7218, #17357, #4647, #28329, #12198, #22669, #9624, #25418, #20105, #28161, #33300, #7392, #17877, #4817, #15127, #20276, #25756, #15296, #30551, #1896, #2240, #12372, #22840, #9800, #22277, #14049, #19201, #11628, #4245, #6815, #27083, #6649, #12132, #11799, #27252, #29983, #32229, #32556, #19700, #17296, #27757, #1491, #16628, #14719, #16794, #21941, #6488, #14379, #24838, #3744, #19371, #32720, #19535, #17130, #11965, #24510, #30145, #1316, #22112, #9216, #19864, #27586, #29640, #25179, #6143, #29815, #4075, #14550, #25009, #3910, #9055, #22436, #982, #27419, #6318, #32883, #9382, #3577, #30318, #16961, #8718, #1657, #11467, #14216, #32391, #8886, #24672, #1146, #30836, #30658, #4928, #17812, #33767, #4756, #15233, #33233, #25864, #31182, #20218, #27930, #2354, #9732, #7155, #20564, #17638, #28099, #4587, #4414, #2008, #10085, #7673, #6987, #12828, #20041, #28270, #28601, #15063, #31009, #22953 ),
 ( #18159, #2177, #23300, #10258, #22604, #12309, #26037, #25352, #25531, #7506, #15409, #22781, #17990, #2531, #12484, #25696, #20740, #33411, #5100, #30486, #12650, #33058, #9908, #17470, #23120, #20385, #9563, #7328, #15586, #33584, #14891, #28437, #1831, #29272, #99, #5606, #13838, #32012, #2862, #26203, #16421, #10588, #8338, #21236, #13509, #8172, #23972, #18663, #2697, #15748, #442, #28770, #18828, #21066, #10925, #5774, #26873, #16254, #31515, #3207, #13675, #24139, #21399, #31679, #16088, #8009, #29101, #15917, #31845, #5940, #3368, #26373, #18995, #10758, #26710, #18324, #31343, #18494, #5266, #13157, #23632, #26541, #3036, #28937, #606, #5436, #7835, #13332, #23806, #11098, #21567, #24305, #8507, #29439, #271, #779, #11261, #8840, #21737, #6605, #21896, #27375, #22393, #22065, #24628, #1610, #1445, #11922, #14336, #11421, #29939, #17082, #27036, #32842, #30098, #32346, #4201, #11584, #27542, #19323, #29765, #6272, #24792, #9010, #19490, #6443, #32182, #16914, #6100, #16749, #14673, #3864, #941, #29598, #27207, #1271, #3698, #8677, #14504, #16581, #24963, #3531, #6771, #17252, #11751, #22232, #27712, #25133, #9333, #4029, #32676, #14171, #19656, #1101, #32509, #9172, #14003, #19819, #30271, #19159, #24465, #25819, #9514, #17764, #18108, #4541, #10041, #12438, #25309, #15365, #5054, #20338, #22556, #1964, #20517, #9689, #2133, #4883, #30788, #31137, #25654, #2309, #12782, #12088, #1781, #15538, #14843, #30613, #30963, #23255, #12259, #7461, #25990, #25485, #15190, #33718, #15014, #10215, #19995, #12608, #33009, #17591, #27885, #30443, #22908, #28557, #20695, #6941, #17944, #17424, #23077, #7109, #9861, #4368, #33365, #33538, #7628, #22736, #33186, #20170, #28053, #7281, #28223, #4710, #28394, #29060, #31475, #23593, #26500, #23762, #10886, #16215, #28730, #400, #5565, #15874, #2993, #24099, #16045, #33886, #11058, #10378, #58, #13465, #21361, #31804, #8135, #13287, #23932, #18285, #31636, #10546, #18624, #18786, #20856, #8295, #227, #2484, #26331, #8465, #21025, #13635, #29230, #26668, #5735, #3164, #567, #18453, #21523, #31971, #18954, #29399, #13119, #5899, #16378, #7967, #7795, #12952, #28895, #5398, #23425, #31302, #2657, #5226, #15708, #2819, #10715, #26164, #21194, #17038, #19448, #16539, #1058, #11706, #32138, #27498, #1226, #3490, #9291, #16706, #22189, #13959, #26991, #24422, #29894, #14130, #24586, #11538, #3327, #22021, #11218, #899, #19776, #32465, #6055, #11381, #32636, #26831, #1402, #733, #21856, #6395, #24750, #9130, #8966, #3653, #16871, #8633, #27333, #32303, #3820, #19612, #24265, #14293, #30058, #13797, #27161, #32798, #8796, #3987, #6563, #14460, #24917, #11878, #22351, #19279, #30226, #6726, #21692, #19117, #29721, #29555, #6227, #14800, #22515, #20941, #4326, #25265, #15627, #2216, #12695, #23165, #32966, #31053, #5139, #2738, #1568, #31390, #14631, #23344, #23678, #10126, #26078, #18030, #30397, #7880, #10633, #25904, #27668, #7545, #2574, #33627, #7713, #10463, #2398 ) ),
 .UNSPECIFIED., .T., .F., .T. ) 
 B_SPLINE_SURFACE_WITH_KNOTS ( ( 4, 3, 4 ),
 ( 3, 2, 2, 2, 2, 2, 2, 2, 2, 2, 2, 2, 2, 2, 2, 2, 2, 2, 2, 2, 2, 2, 2, 2, 2, 2, 2, 2, 2, 2, 2, 2, 2, 2, 2, 2, 2, 2, 2, 2, 2, 2, 2, 2, 2, 2, 2, 2, 2, 2, 2, 2, 2, 2, 2, 2, 2, 2, 2, 2, 2, 2, 2, 2, 2, 2, 2, 2, 2, 2, 2, 2, 2, 2, 2, 2, 2, 2, 2, 2, 2, 2, 2, 2, 2, 2, 2, 2, 2, 2, 2, 2, 2, 2, 2, 2, 2, 2, 2, 2, 2, 2, 2, 2, 2, 2, 2, 2, 2, 2, 2, 2, 2, 2, 2, 2, 2, 2, 2, 2, 2, 2, 2, 2, 2, 2, 2, 2, 2, 2, 2, 2, 2, 2, 2, 2, 2, 2, 2, 2, 2, 2, 2, 2, 2, 2, 2, 2, 2, 2, 2, 2, 2, 2, 2, 2, 2, 2, 2, 2, 2, 2, 2, 2, 2, 2, 2, 2, 2, 2, 2, 2, 2, 2, 2, 2, 2, 2, 2, 2, 2, 2, 2, 2, 2, 2, 2, 2, 2, 2, 2, 2, 3 ),
 ( 0.000000000000000000, 0.5000000000000000000, 1.000000000000000000 ),
 ( 0.000000000000000000, 0.005208333333333333044, 0.01041666666666666609, 0.01562500000000000000, 0.02083333333333333218, 0.02604166666666666782, 0.03125000000000000000, 0.03645833333333333565, 0.04166666666666666435, 0.04687500000000000000, 0.05208333333333333565, 0.05729166666666666435, 0.06250000000000000000, 0.06770833333333332871, 0.07291666666666667129, 0.07812500000000000000, 0.08333333333333332871, 0.08854166666666667129, 0.09375000000000000000, 0.09895833333333332871, 0.1041666666666666713, 0.1093750000000000000, 0.1145833333333333287, 0.1197916666666666713, 0.1250000000000000000, 0.1302083333333333426, 0.1354166666666666574, 0.1406250000000000000, 0.1458333333333333426, 0.1510416666666666574, 0.1562500000000000000, 0.1614583333333333426, 0.1666666666666666574, 0.1718750000000000000, 0.1770833333333333426, 0.1822916666666666574, 0.1875000000000000000, 0.1927083333333333426, 0.1979166666666666574, 0.2031250000000000000, 0.2083333333333333426, 0.2135416666666666574, 0.2187500000000000000, 0.2239583333333333426, 0.2291666666666666574, 0.2343750000000000000, 0.2395833333333333426, 0.2447916666666666574, 0.2500000000000000000, 0.2552083333333333148, 0.2604166666666666852, 0.2656250000000000000, 0.2708333333333333148, 0.2760416666666666852, 0.2812500000000000000, 0.2864583333333333148, 0.2916666666666666852, 0.2968750000000000000, 0.3020833333333333148, 0.3072916666666666852, 0.3125000000000000000, 0.3177083333333333148, 0.3229166666666666852, 0.3281250000000000000, 0.3333333333333333148, 0.3385416666666666852, 0.3437500000000000000, 0.3489583333333333148, 0.3541666666666666852, 0.3593750000000000000, 0.3645833333333333148, 0.3697916666666666852, 0.3750000000000000000, 0.3802083333333333148, 0.3854166666666666852, 0.3906250000000000000, 0.3958333333333333148, 0.4010416666666666852, 0.4062500000000000000, 0.4114583333333333148, 0.4166666666666666852, 0.4218750000000000000, 0.4270833333333333148, 0.4322916666666666852, 0.4375000000000000000, 0.4427083333333333148, 0.4479166666666666852, 0.4531250000000000000, 0.4583333333333333148, 0.4635416666666666852, 0.4687500000000000000, 0.4739583333333333148, 0.4791666666666666852, 0.4843750000000000000, 0.4895833333333333148, 0.4947916666666666852, 0.5000000000000000000, 0.5052083333333333703, 0.5104166666666666297, 0.5156250000000000000, 0.5208333333333333703, 0.5260416666666666297, 0.5312500000000000000, 0.5364583333333333703, 0.5416666666666666297, 0.5468750000000000000, 0.5520833333333333703, 0.5572916666666666297, 0.5625000000000000000, 0.5677083333333333703, 0.5729166666666666297, 0.5781250000000000000, 0.5833333333333333703, 0.5885416666666666297, 0.5937500000000000000, 0.5989583333333333703, 0.6041666666666666297, 0.6093750000000000000, 0.6145833333333333703, 0.6197916666666666297, 0.6250000000000000000, 0.6302083333333333703, 0.6354166666666666297, 0.6406250000000000000, 0.6458333333333333703, 0.6510416666666666297, 0.6562500000000000000, 0.6614583333333333703, 0.6666666666666666297, 0.6718750000000000000, 0.6770833333333333703, 0.6822916666666666297, 0.6875000000000000000, 0.6927083333333333703, 0.6979166666666666297, 0.7031250000000000000, 0.7083333333333333703, 0.7135416666666666297, 0.7187500000000000000, 0.7239583333333333703, 0.7291666666666666297, 0.7343750000000000000, 0.7395833333333333703, 0.7447916666666666297, 0.7500000000000000000, 0.7552083333333333703, 0.7604166666666666297, 0.7656250000000000000, 0.7708333333333333703, 0.7760416666666666297, 0.7812500000000000000, 0.7864583333333333703, 0.7916666666666666297, 0.7968750000000000000, 0.8020833333333333703, 0.8072916666666666297, 0.8125000000000000000, 0.8177083333333333703, 0.8229166666666666297, 0.8281250000000000000, 0.8333333333333333703, 0.8385416666666666297, 0.8437500000000000000, 0.8489583333333333703, 0.8541666666666666297, 0.8593750000000000000, 0.8645833333333333703, 0.8697916666666666297, 0.8750000000000000000, 0.8802083333333333703, 0.8854166666666666297, 0.8906250000000000000, 0.8958333333333333703, 0.9010416666666666297, 0.9062500000000000000, 0.9114583333333333703, 0.9166666666666666297, 0.9218750000000000000, 0.9270833333333333703, 0.9322916666666666297, 0.9375000000000000000, 0.9427083333333333703, 0.9479166666666666297, 0.9531250000000000000, 0.9583333333333333703, 0.9635416666666666297, 0.9687500000000000000, 0.9739583333333333703, 0.9791666666666666297, 0.9843750000000000000, 0.9895833333333333703, 0.9947916666666666297, 1.000000000000000000 ),
 .UNSPECIFIED. ) 
 GEOMETRIC_REPRESENTATION_ITEM ( )  RATIONAL_B_SPLINE_SURFACE ( (
 ( 1.000000000000000000, 0.9659258262890683122, 1.000000000000000000, 0.9659258262890683122, 1.000000000000000000, 0.9659258262890683122, 1.000000000000000000, 0.9659258262890683122, 1.000000000000000000, 0.9659258262890683122, 1.000000000000000000, 0.9659258262890683122, 1.000000000000000000, 0.9659258262890683122, 1.000000000000000000, 0.9659258262890683122, 1.000000000000000000, 0.9659258262890683122, 1.000000000000000000, 0.9659258262890683122, 1.000000000000000000, 0.9659258262890683122, 1.000000000000000000, 0.9659258262890683122, 1.000000000000000000, 0.9659258262890683122, 1.000000000000000000, 0.9659258262890683122, 1.000000000000000000, 0.9659258262890683122, 1.000000000000000000, 0.9659258262890683122, 1.000000000000000000, 0.9659258262890683122, 1.000000000000000000, 0.9659258262890683122, 1.000000000000000000, 0.9659258262890683122, 1.000000000000000000, 0.9659258262890683122, 1.000000000000000000, 0.9659258262890683122, 1.000000000000000000, 0.9659258262890683122, 1.000000000000000000, 0.9659258262890683122, 1.000000000000000000, 0.9659258262890683122, 1.000000000000000000, 0.9659258262890683122, 1.000000000000000000, 0.9659258262890683122, 1.000000000000000000, 0.9659258262890683122, 1.000000000000000000, 0.9659258262890683122, 1.000000000000000000, 0.9659258262890683122, 1.000000000000000000, 0.9659258262890683122, 1.000000000000000000, 0.9659258262890683122, 1.000000000000000000, 0.9659258262890683122, 1.000000000000000000, 0.9659258262890683122, 1.000000000000000000, 0.9659258262890683122, 1.000000000000000000, 0.9659258262890683122, 1.000000000000000000, 0.9659258262890683122, 1.000000000000000000, 0.9659258262890683122, 1.000000000000000000, 0.9659258262890683122, 1.000000000000000000, 0.9659258262890683122, 1.000000000000000000, 0.9659258262890683122, 1.000000000000000000, 0.9659258262890683122, 1.000000000000000000, 0.9659258262890683122, 1.000000000000000000, 0.9659258262890683122, 1.000000000000000000, 0.9659258262890683122, 1.000000000000000000, 0.9659258262890683122, 1.000000000000000000, 0.9659258262890683122, 1.000000000000000000, 0.9659258262890683122, 1.000000000000000000, 0.9659258262890683122, 1.000000000000000000, 0.9659258262890683122, 1.000000000000000000, 0.9659258262890683122, 1.000000000000000000, 0.9659258262890683122, 1.000000000000000000, 0.9659258262890683122, 1.000000000000000000, 0.9659258262890683122, 1.000000000000000000, 0.9659258262890683122, 1.000000000000000000, 0.9659258262890683122, 1.000000000000000000, 0.9659258262890683122, 1.000000000000000000, 0.9659258262890683122, 1.000000000000000000, 0.9659258262890683122, 1.000000000000000000, 0.9659258262890683122, 1.000000000000000000, 0.9659258262890683122, 1.000000000000000000, 0.9659258262890683122, 1.000000000000000000, 0.9659258262890683122, 1.000000000000000000, 0.9659258262890683122, 1.000000000000000000, 0.9659258262890683122, 1.000000000000000000, 0.9659258262890683122, 1.000000000000000000, 0.9659258262890683122, 1.000000000000000000, 0.9659258262890683122, 1.000000000000000000, 0.9659258262890683122, 1.000000000000000000, 0.9659258262890683122, 1.000000000000000000, 0.9659258262890683122, 1.000000000000000000, 0.9659258262890683122, 1.000000000000000000, 0.9659258262890683122, 1.000000000000000000, 0.9659258262890683122, 1.000000000000000000, 0.9659258262890683122, 1.000000000000000000, 0.9659258262890683122, 1.000000000000000000, 0.9659258262890683122, 1.000000000000000000, 0.9659258262890683122, 1.000000000000000000, 0.9659258262890683122, 1.000000000000000000, 0.9659258262890683122, 1.000000000000000000, 0.9659258262890683122, 1.000000000000000000, 0.9659258262890683122, 1.000000000000000000, 0.9659258262890683122, 1.000000000000000000, 0.9659258262890683122, 1.000000000000000000, 0.9659258262890683122, 1.000000000000000000, 0.9659258262890683122, 1.000000000000000000, 0.9659258262890683122, 1.000000000000000000, 0.9659258262890683122, 1.000000000000000000, 0.9659258262890683122, 1.000000000000000000, 0.9659258262890683122, 1.000000000000000000, 0.9659258262890683122, 1.000000000000000000, 0.9659258262890683122, 1.000000000000000000, 0.9659258262890683122, 1.000000000000000000, 0.9659258262890683122, 1.000000000000000000, 0.9659258262890683122, 1.000000000000000000, 0.9659258262890683122, 1.000000000000000000, 0.9659258262890683122, 1.000000000000000000, 0.9659258262890683122, 1.000000000000000000, 0.9659258262890683122, 1.000000000000000000, 0.9659258262890683122, 1.000000000000000000, 0.9659258262890683122, 1.000000000000000000, 0.9659258262890683122, 1.000000000000000000, 0.9659258262890683122, 1.000000000000000000, 0.9659258262890683122, 1.000000000000000000, 0.9659258262890683122, 1.000000000000000000, 0.9659258262890683122, 1.000000000000000000, 0.9659258262890683122, 1.000000000000000000, 0.9659258262890683122, 1.000000000000000000, 0.9659258262890683122, 1.000000000000000000, 0.9659258262890683122, 1.000000000000000000, 0.9659258262890683122, 1.000000000000000000, 0.9659258262890683122, 1.000000000000000000, 0.9659258262890683122, 1.000000000000000000, 0.9659258262890683122, 1.000000000000000000, 0.9659258262890683122, 1.000000000000000000, 0.9659258262890683122, 1.000000000000000000, 0.9659258262890683122, 1.000000000000000000, 0.9659258262890683122, 1.000000000000000000, 0.9659258262890683122, 1.000000000000000000, 0.9659258262890683122, 1.000000000000000000, 0.9659258262890683122, 1.000000000000000000, 0.9659258262890683122, 1.000000000000000000, 0.9659258262890683122, 1.000000000000000000, 0.9659258262890683122, 1.000000000000000000, 0.9659258262890683122, 1.000000000000000000, 0.9659258262890683122, 1.000000000000000000, 0.9659258262890683122, 1.000000000000000000, 0.9659258262890683122, 1.000000000000000000, 0.9659258262890683122, 1.000000000000000000, 0.9659258262890683122, 1.000000000000000000, 0.9659258262890683122, 1.000000000000000000, 0.9659258262890683122, 1.000000000000000000, 0.9659258262890683122, 1.000000000000000000, 0.9659258262890683122, 1.000000000000000000, 0.9659258262890683122, 1.000000000000000000, 0.9659258262890683122, 1.000000000000000000, 0.9659258262890683122, 1.000000000000000000, 0.9659258262890683122, 1.000000000000000000, 0.9659258262890683122, 1.000000000000000000, 0.9659258262890683122, 1.000000000000000000, 0.9659258262890683122, 1.000000000000000000, 0.9659258262890683122, 1.000000000000000000, 0.9659258262890683122, 1.000000000000000000, 0.9659258262890683122, 1.000000000000000000, 0.9659258262890683122, 1.000000000000000000, 0.9659258262890683122, 1.000000000000000000, 0.9659258262890683122, 1.000000000000000000, 0.9659258262890683122, 1.000000000000000000, 0.9659258262890683122, 1.000000000000000000, 0.9659258262890683122, 1.000000000000000000, 0.9659258262890683122, 1.000000000000000000, 0.9659258262890683122, 1.000000000000000000, 0.9659258262890683122, 1.000000000000000000, 0.9659258262890683122, 1.000000000000000000, 0.9659258262890683122, 1.000000000000000000, 0.9659258262890683122, 1.000000000000000000, 0.9659258262890683122, 1.000000000000000000, 0.9659258262890683122, 1.000000000000000000, 0.9659258262890683122, 1.000000000000000000, 0.9659258262890683122, 1.000000000000000000, 0.9659258262890683122, 1.000000000000000000, 0.9659258262890683122, 1.000000000000000000, 0.9659258262890683122, 1.000000000000000000, 0.9659258262890683122, 1.000000000000000000, 0.9659258262890683122, 1.000000000000000000, 0.9659258262890683122, 1.000000000000000000, 0.9659258262890683122, 1.000000000000000000, 0.9659258262890683122, 1.000000000000000000, 0.9659258262890683122, 1.000000000000000000, 0.9659258262890683122, 1.000000000000000000, 0.9659258262890683122, 1.000000000000000000, 0.9659258262890683122, 1.000000000000000000, 0.9659258262890683122, 1.000000000000000000, 0.9659258262890683122, 1.000000000000000000, 0.9659258262890683122, 1.000000000000000000, 0.9659258262890683122, 1.000000000000000000, 0.9659258262890683122, 1.000000000000000000, 0.9659258262890683122, 1.000000000000000000, 0.9659258262890683122, 1.000000000000000000, 0.9659258262890683122, 1.000000000000000000, 0.9659258262890683122, 1.000000000000000000, 0.9659258262890683122, 1.000000000000000000, 0.9659258262890683122, 1.000000000000000000, 0.9659258262890683122, 1.000000000000000000, 0.9659258262890683122, 1.000000000000000000, 0.9659258262890683122, 1.000000000000000000, 0.9659258262890683122, 1.000000000000000000, 0.9659258262890683122, 1.000000000000000000, 0.9659258262890683122, 1.000000000000000000, 0.9659258262890683122, 1.000000000000000000, 0.9659258262890683122, 1.000000000000000000, 0.9659258262890683122, 1.000000000000000000, 0.9659258262890683122, 1.000000000000000000),
 ( 0.3333333333333333703, 0.3219752754296894559, 0.3333333333333333703, 0.3219752754296894559, 0.3333333333333333703, 0.3219752754296894559, 0.3333333333333333703, 0.3219752754296894559, 0.3333333333333333703, 0.3219752754296894559, 0.3333333333333333703, 0.3219752754296894559, 0.3333333333333333703, 0.3219752754296894559, 0.3333333333333333703, 0.3219752754296894559, 0.3333333333333333703, 0.3219752754296894559, 0.3333333333333333703, 0.3219752754296894559, 0.3333333333333333703, 0.3219752754296894559, 0.3333333333333333703, 0.3219752754296894559, 0.3333333333333333703, 0.3219752754296894559, 0.3333333333333333703, 0.3219752754296894559, 0.3333333333333333703, 0.3219752754296894559, 0.3333333333333333703, 0.3219752754296894559, 0.3333333333333333703, 0.3219752754296894559, 0.3333333333333333703, 0.3219752754296894559, 0.3333333333333333703, 0.3219752754296894559, 0.3333333333333333703, 0.3219752754296894559, 0.3333333333333333703, 0.3219752754296894559, 0.3333333333333333703, 0.3219752754296894559, 0.3333333333333333703, 0.3219752754296894559, 0.3333333333333333703, 0.3219752754296894559, 0.3333333333333333703, 0.3219752754296894559, 0.3333333333333333703, 0.3219752754296894559, 0.3333333333333333703, 0.3219752754296894559, 0.3333333333333333703, 0.3219752754296894559, 0.3333333333333333703, 0.3219752754296894559, 0.3333333333333333703, 0.3219752754296894559, 0.3333333333333333703, 0.3219752754296894559, 0.3333333333333333703, 0.3219752754296894559, 0.3333333333333333703, 0.3219752754296894559, 0.3333333333333333703, 0.3219752754296894559, 0.3333333333333333703, 0.3219752754296894559, 0.3333333333333333703, 0.3219752754296894559, 0.3333333333333333703, 0.3219752754296894559, 0.3333333333333333703, 0.3219752754296894559, 0.3333333333333333703, 0.3219752754296894559, 0.3333333333333333703, 0.3219752754296894559, 0.3333333333333333703, 0.3219752754296894559, 0.3333333333333333703, 0.3219752754296894559, 0.3333333333333333703, 0.3219752754296894559, 0.3333333333333333703, 0.3219752754296894559, 0.3333333333333333703, 0.3219752754296894559, 0.3333333333333333703, 0.3219752754296894559, 0.3333333333333333703, 0.3219752754296894559, 0.3333333333333333703, 0.3219752754296894559, 0.3333333333333333703, 0.3219752754296894559, 0.3333333333333333703, 0.3219752754296894559, 0.3333333333333333703, 0.3219752754296894559, 0.3333333333333333703, 0.3219752754296894559, 0.3333333333333333703, 0.3219752754296894559, 0.3333333333333333703, 0.3219752754296894559, 0.3333333333333333703, 0.3219752754296894559, 0.3333333333333333703, 0.3219752754296894559, 0.3333333333333333703, 0.3219752754296894559, 0.3333333333333333703, 0.3219752754296894559, 0.3333333333333333703, 0.3219752754296894559, 0.3333333333333333703, 0.3219752754296894559, 0.3333333333333333703, 0.3219752754296894559, 0.3333333333333333703, 0.3219752754296894559, 0.3333333333333333703, 0.3219752754296894559, 0.3333333333333333703, 0.3219752754296894559, 0.3333333333333333703, 0.3219752754296894559, 0.3333333333333333703, 0.3219752754296894559, 0.3333333333333333703, 0.3219752754296894559, 0.3333333333333333703, 0.3219752754296894559, 0.3333333333333333703, 0.3219752754296894559, 0.3333333333333333703, 0.3219752754296894559, 0.3333333333333333703, 0.3219752754296894559, 0.3333333333333333703, 0.3219752754296894559, 0.3333333333333333703, 0.3219752754296894559, 0.3333333333333333703, 0.3219752754296894559, 0.3333333333333333703, 0.3219752754296894559, 0.3333333333333333703, 0.3219752754296894559, 0.3333333333333333703, 0.3219752754296894559, 0.3333333333333333703, 0.3219752754296894559, 0.3333333333333333703, 0.3219752754296894559, 0.3333333333333333703, 0.3219752754296894559, 0.3333333333333333703, 0.3219752754296894559, 0.3333333333333333703, 0.3219752754296894559, 0.3333333333333333703, 0.3219752754296894559, 0.3333333333333333703, 0.3219752754296894559, 0.3333333333333333703, 0.3219752754296894559, 0.3333333333333333703, 0.3219752754296894559, 0.3333333333333333703, 0.3219752754296894559, 0.3333333333333333703, 0.3219752754296894559, 0.3333333333333333703, 0.3219752754296894559, 0.3333333333333333703, 0.3219752754296894559, 0.3333333333333333703, 0.3219752754296894559, 0.3333333333333333703, 0.3219752754296894559, 0.3333333333333333703, 0.3219752754296894559, 0.3333333333333333703, 0.3219752754296894559, 0.3333333333333333703, 0.3219752754296894559, 0.3333333333333333703, 0.3219752754296894559, 0.3333333333333333703, 0.3219752754296894559, 0.3333333333333333703, 0.3219752754296894559, 0.3333333333333333703, 0.3219752754296894559, 0.3333333333333333703, 0.3219752754296894559, 0.3333333333333333703, 0.3219752754296894559, 0.3333333333333333703, 0.3219752754296894559, 0.3333333333333333703, 0.3219752754296894559, 0.3333333333333333703, 0.3219752754296894559, 0.3333333333333333703, 0.3219752754296894559, 0.3333333333333333703, 0.3219752754296894559, 0.3333333333333333703, 0.3219752754296894559, 0.3333333333333333703, 0.3219752754296894559, 0.3333333333333333703, 0.3219752754296894559, 0.3333333333333333703, 0.3219752754296894559, 0.3333333333333333703, 0.3219752754296894559, 0.3333333333333333703, 0.3219752754296894559, 0.3333333333333333703, 0.3219752754296894559, 0.3333333333333333703, 0.3219752754296894559, 0.3333333333333333703, 0.3219752754296894559, 0.3333333333333333703, 0.3219752754296894559, 0.3333333333333333703, 0.3219752754296894559, 0.3333333333333333703, 0.3219752754296894559, 0.3333333333333333703, 0.3219752754296894559, 0.3333333333333333703, 0.3219752754296894559, 0.3333333333333333703, 0.3219752754296894559, 0.3333333333333333703, 0.3219752754296894559, 0.3333333333333333703, 0.3219752754296894559, 0.3333333333333333703, 0.3219752754296894559, 0.3333333333333333703, 0.3219752754296894559, 0.3333333333333333703, 0.3219752754296894559, 0.3333333333333333703, 0.3219752754296894559, 0.3333333333333333703, 0.3219752754296894559, 0.3333333333333333703, 0.3219752754296894559, 0.3333333333333333703, 0.3219752754296894559, 0.3333333333333333703, 0.3219752754296894559, 0.3333333333333333703, 0.3219752754296894559, 0.3333333333333333703, 0.3219752754296894559, 0.3333333333333333703, 0.3219752754296894559, 0.3333333333333333703, 0.3219752754296894559, 0.3333333333333333703, 0.3219752754296894559, 0.3333333333333333703, 0.3219752754296894559, 0.3333333333333333703, 0.3219752754296894559, 0.3333333333333333703, 0.3219752754296894559, 0.3333333333333333703, 0.3219752754296894559, 0.3333333333333333703, 0.3219752754296894559, 0.3333333333333333703, 0.3219752754296894559, 0.3333333333333333703, 0.3219752754296894559, 0.3333333333333333703, 0.3219752754296894559, 0.3333333333333333703, 0.3219752754296894559, 0.3333333333333333703, 0.3219752754296894559, 0.3333333333333333703, 0.3219752754296894559, 0.3333333333333333703, 0.3219752754296894559, 0.3333333333333333703, 0.3219752754296894559, 0.3333333333333333703, 0.3219752754296894559, 0.3333333333333333703, 0.3219752754296894559, 0.3333333333333333703, 0.3219752754296894559, 0.3333333333333333703, 0.3219752754296894559, 0.3333333333333333703, 0.3219752754296894559, 0.3333333333333333703, 0.3219752754296894559, 0.3333333333333333703, 0.3219752754296894559, 0.3333333333333333703, 0.3219752754296894559, 0.3333333333333333703, 0.3219752754296894559, 0.3333333333333333703, 0.3219752754296894559, 0.3333333333333333703, 0.3219752754296894559, 0.3333333333333333703, 0.3219752754296894559, 0.3333333333333333703, 0.3219752754296894559, 0.3333333333333333703, 0.3219752754296894559, 0.3333333333333333703, 0.3219752754296894559, 0.3333333333333333703, 0.3219752754296894559, 0.3333333333333333703, 0.3219752754296894559, 0.3333333333333333703, 0.3219752754296894559, 0.3333333333333333703, 0.3219752754296894559, 0.3333333333333333703, 0.3219752754296894559, 0.3333333333333333703, 0.3219752754296894559, 0.3333333333333333703, 0.3219752754296894559, 0.3333333333333333703, 0.3219752754296894559, 0.3333333333333333703, 0.3219752754296894559, 0.3333333333333333703, 0.3219752754296894559, 0.3333333333333333703, 0.3219752754296894559, 0.3333333333333333703, 0.3219752754296894559, 0.3333333333333333703, 0.3219752754296894559, 0.3333333333333333703, 0.3219752754296894559, 0.3333333333333333703, 0.3219752754296894559, 0.3333333333333333703, 0.3219752754296894559, 0.3333333333333333703, 0.3219752754296894559, 0.3333333333333333703, 0.3219752754296894559, 0.3333333333333333703, 0.3219752754296894559, 0.3333333333333333703, 0.3219752754296894559, 0.3333333333333333703, 0.3219752754296894559, 0.3333333333333333703, 0.3219752754296894559, 0.3333333333333333703, 0.3219752754296894559, 0.3333333333333333703, 0.3219752754296894559, 0.3333333333333333703, 0.3219752754296894559, 0.3333333333333333703, 0.3219752754296894559, 0.3333333333333333703, 0.3219752754296894559, 0.3333333333333333703, 0.3219752754296894559, 0.3333333333333333703),
 ( 0.3333333333333333703, 0.3219752754296894559, 0.3333333333333333703, 0.3219752754296894559, 0.3333333333333333703, 0.3219752754296894559, 0.3333333333333333703, 0.3219752754296894559, 0.3333333333333333703, 0.3219752754296894559, 0.3333333333333333703, 0.3219752754296894559, 0.3333333333333333703, 0.3219752754296894559, 0.3333333333333333703, 0.3219752754296894559, 0.3333333333333333703, 0.3219752754296894559, 0.3333333333333333703, 0.3219752754296894559, 0.3333333333333333703, 0.3219752754296894559, 0.3333333333333333703, 0.3219752754296894559, 0.3333333333333333703, 0.3219752754296894559, 0.3333333333333333703, 0.3219752754296894559, 0.3333333333333333703, 0.3219752754296894559, 0.3333333333333333703, 0.3219752754296894559, 0.3333333333333333703, 0.3219752754296894559, 0.3333333333333333703, 0.3219752754296894559, 0.3333333333333333703, 0.3219752754296894559, 0.3333333333333333703, 0.3219752754296894559, 0.3333333333333333703, 0.3219752754296894559, 0.3333333333333333703, 0.3219752754296894559, 0.3333333333333333703, 0.3219752754296894559, 0.3333333333333333703, 0.3219752754296894559, 0.3333333333333333703, 0.3219752754296894559, 0.3333333333333333703, 0.3219752754296894559, 0.3333333333333333703, 0.3219752754296894559, 0.3333333333333333703, 0.3219752754296894559, 0.3333333333333333703, 0.3219752754296894559, 0.3333333333333333703, 0.3219752754296894559, 0.3333333333333333703, 0.3219752754296894559, 0.3333333333333333703, 0.3219752754296894559, 0.3333333333333333703, 0.3219752754296894559, 0.3333333333333333703, 0.3219752754296894559, 0.3333333333333333703, 0.3219752754296894559, 0.3333333333333333703, 0.3219752754296894559, 0.3333333333333333703, 0.3219752754296894559, 0.3333333333333333703, 0.3219752754296894559, 0.3333333333333333703, 0.3219752754296894559, 0.3333333333333333703, 0.3219752754296894559, 0.3333333333333333703, 0.3219752754296894559, 0.3333333333333333703, 0.3219752754296894559, 0.3333333333333333703, 0.3219752754296894559, 0.3333333333333333703, 0.3219752754296894559, 0.3333333333333333703, 0.3219752754296894559, 0.3333333333333333703, 0.3219752754296894559, 0.3333333333333333703, 0.3219752754296894559, 0.3333333333333333703, 0.3219752754296894559, 0.3333333333333333703, 0.3219752754296894559, 0.3333333333333333703, 0.3219752754296894559, 0.3333333333333333703, 0.3219752754296894559, 0.3333333333333333703, 0.3219752754296894559, 0.3333333333333333703, 0.3219752754296894559, 0.3333333333333333703, 0.3219752754296894559, 0.3333333333333333703, 0.3219752754296894559, 0.3333333333333333703, 0.3219752754296894559, 0.3333333333333333703, 0.3219752754296894559, 0.3333333333333333703, 0.3219752754296894559, 0.3333333333333333703, 0.3219752754296894559, 0.3333333333333333703, 0.3219752754296894559, 0.3333333333333333703, 0.3219752754296894559, 0.3333333333333333703, 0.3219752754296894559, 0.3333333333333333703, 0.3219752754296894559, 0.3333333333333333703, 0.3219752754296894559, 0.3333333333333333703, 0.3219752754296894559, 0.3333333333333333703, 0.3219752754296894559, 0.3333333333333333703, 0.3219752754296894559, 0.3333333333333333703, 0.3219752754296894559, 0.3333333333333333703, 0.3219752754296894559, 0.3333333333333333703, 0.3219752754296894559, 0.3333333333333333703, 0.3219752754296894559, 0.3333333333333333703, 0.3219752754296894559, 0.3333333333333333703, 0.3219752754296894559, 0.3333333333333333703, 0.3219752754296894559, 0.3333333333333333703, 0.3219752754296894559, 0.3333333333333333703, 0.3219752754296894559, 0.3333333333333333703, 0.3219752754296894559, 0.3333333333333333703, 0.3219752754296894559, 0.3333333333333333703, 0.3219752754296894559, 0.3333333333333333703, 0.3219752754296894559, 0.3333333333333333703, 0.3219752754296894559, 0.3333333333333333703, 0.3219752754296894559, 0.3333333333333333703, 0.3219752754296894559, 0.3333333333333333703, 0.3219752754296894559, 0.3333333333333333703, 0.3219752754296894559, 0.3333333333333333703, 0.3219752754296894559, 0.3333333333333333703, 0.3219752754296894559, 0.3333333333333333703, 0.3219752754296894559, 0.3333333333333333703, 0.3219752754296894559, 0.3333333333333333703, 0.3219752754296894559, 0.3333333333333333703, 0.3219752754296894559, 0.3333333333333333703, 0.3219752754296894559, 0.3333333333333333703, 0.3219752754296894559, 0.3333333333333333703, 0.3219752754296894559, 0.3333333333333333703, 0.3219752754296894559, 0.3333333333333333703, 0.3219752754296894559, 0.3333333333333333703, 0.3219752754296894559, 0.3333333333333333703, 0.3219752754296894559, 0.3333333333333333703, 0.3219752754296894559, 0.3333333333333333703, 0.3219752754296894559, 0.3333333333333333703, 0.3219752754296894559, 0.3333333333333333703, 0.3219752754296894559, 0.3333333333333333703, 0.3219752754296894559, 0.3333333333333333703, 0.3219752754296894559, 0.3333333333333333703, 0.3219752754296894559, 0.3333333333333333703, 0.3219752754296894559, 0.3333333333333333703, 0.3219752754296894559, 0.3333333333333333703, 0.3219752754296894559, 0.3333333333333333703, 0.3219752754296894559, 0.3333333333333333703, 0.3219752754296894559, 0.3333333333333333703, 0.3219752754296894559, 0.3333333333333333703, 0.3219752754296894559, 0.3333333333333333703, 0.3219752754296894559, 0.3333333333333333703, 0.3219752754296894559, 0.3333333333333333703, 0.3219752754296894559, 0.3333333333333333703, 0.3219752754296894559, 0.3333333333333333703, 0.3219752754296894559, 0.3333333333333333703, 0.3219752754296894559, 0.3333333333333333703, 0.3219752754296894559, 0.3333333333333333703, 0.3219752754296894559, 0.3333333333333333703, 0.3219752754296894559, 0.3333333333333333703, 0.3219752754296894559, 0.3333333333333333703, 0.3219752754296894559, 0.3333333333333333703, 0.3219752754296894559, 0.3333333333333333703, 0.3219752754296894559, 0.3333333333333333703, 0.3219752754296894559, 0.3333333333333333703, 0.3219752754296894559, 0.3333333333333333703, 0.3219752754296894559, 0.3333333333333333703, 0.3219752754296894559, 0.3333333333333333703, 0.3219752754296894559, 0.3333333333333333703, 0.3219752754296894559, 0.3333333333333333703, 0.3219752754296894559, 0.3333333333333333703, 0.3219752754296894559, 0.3333333333333333703, 0.3219752754296894559, 0.3333333333333333703, 0.3219752754296894559, 0.3333333333333333703, 0.3219752754296894559, 0.3333333333333333703, 0.3219752754296894559, 0.3333333333333333703, 0.3219752754296894559, 0.3333333333333333703, 0.3219752754296894559, 0.3333333333333333703, 0.3219752754296894559, 0.3333333333333333703, 0.3219752754296894559, 0.3333333333333333703, 0.3219752754296894559, 0.3333333333333333703, 0.3219752754296894559, 0.3333333333333333703, 0.3219752754296894559, 0.3333333333333333703, 0.3219752754296894559, 0.3333333333333333703, 0.3219752754296894559, 0.3333333333333333703, 0.3219752754296894559, 0.3333333333333333703, 0.3219752754296894559, 0.3333333333333333703, 0.3219752754296894559, 0.3333333333333333703, 0.3219752754296894559, 0.3333333333333333703, 0.3219752754296894559, 0.3333333333333333703, 0.3219752754296894559, 0.3333333333333333703, 0.3219752754296894559, 0.3333333333333333703, 0.3219752754296894559, 0.3333333333333333703, 0.3219752754296894559, 0.3333333333333333703, 0.3219752754296894559, 0.3333333333333333703, 0.3219752754296894559, 0.3333333333333333703, 0.3219752754296894559, 0.3333333333333333703, 0.3219752754296894559, 0.3333333333333333703, 0.3219752754296894559, 0.3333333333333333703, 0.3219752754296894559, 0.3333333333333333703, 0.3219752754296894559, 0.3333333333333333703, 0.3219752754296894559, 0.3333333333333333703, 0.3219752754296894559, 0.3333333333333333703, 0.3219752754296894559, 0.3333333333333333703, 0.3219752754296894559, 0.3333333333333333703, 0.3219752754296894559, 0.3333333333333333703, 0.3219752754296894559, 0.3333333333333333703, 0.3219752754296894559, 0.3333333333333333703, 0.3219752754296894559, 0.3333333333333333703, 0.3219752754296894559, 0.3333333333333333703, 0.3219752754296894559, 0.3333333333333333703, 0.3219752754296894559, 0.3333333333333333703, 0.3219752754296894559, 0.3333333333333333703, 0.3219752754296894559, 0.3333333333333333703, 0.3219752754296894559, 0.3333333333333333703, 0.3219752754296894559, 0.3333333333333333703, 0.3219752754296894559, 0.3333333333333333703, 0.3219752754296894559, 0.3333333333333333703, 0.3219752754296894559, 0.3333333333333333703, 0.3219752754296894559, 0.3333333333333333703, 0.3219752754296894559, 0.3333333333333333703, 0.3219752754296894559, 0.3333333333333333703, 0.3219752754296894559, 0.3333333333333333703, 0.3219752754296894559, 0.3333333333333333703, 0.3219752754296894559, 0.3333333333333333703, 0.3219752754296894559, 0.3333333333333333703, 0.3219752754296894559, 0.3333333333333333703, 0.3219752754296894559, 0.3333333333333333703, 0.3219752754296894559, 0.3333333333333333703, 0.3219752754296894559, 0.3333333333333333703, 0.3219752754296894559, 0.3333333333333333703),
 ( 1.000000000000000000, 0.9659258262890683122, 1.000000000000000000, 0.9659258262890683122, 1.000000000000000000, 0.9659258262890683122, 1.000000000000000000, 0.9659258262890683122, 1.000000000000000000, 0.9659258262890683122, 1.000000000000000000, 0.9659258262890683122, 1.000000000000000000, 0.9659258262890683122, 1.000000000000000000, 0.9659258262890683122, 1.000000000000000000, 0.9659258262890683122, 1.000000000000000000, 0.9659258262890683122, 1.000000000000000000, 0.9659258262890683122, 1.000000000000000000, 0.9659258262890683122, 1.000000000000000000, 0.9659258262890683122, 1.000000000000000000, 0.9659258262890683122, 1.000000000000000000, 0.9659258262890683122, 1.000000000000000000, 0.9659258262890683122, 1.000000000000000000, 0.9659258262890683122, 1.000000000000000000, 0.9659258262890683122, 1.000000000000000000, 0.9659258262890683122, 1.000000000000000000, 0.9659258262890683122, 1.000000000000000000, 0.9659258262890683122, 1.000000000000000000, 0.9659258262890683122, 1.000000000000000000, 0.9659258262890683122, 1.000000000000000000, 0.9659258262890683122, 1.000000000000000000, 0.9659258262890683122, 1.000000000000000000, 0.9659258262890683122, 1.000000000000000000, 0.9659258262890683122, 1.000000000000000000, 0.9659258262890683122, 1.000000000000000000, 0.9659258262890683122, 1.000000000000000000, 0.9659258262890683122, 1.000000000000000000, 0.9659258262890683122, 1.000000000000000000, 0.9659258262890683122, 1.000000000000000000, 0.9659258262890683122, 1.000000000000000000, 0.9659258262890683122, 1.000000000000000000, 0.9659258262890683122, 1.000000000000000000, 0.9659258262890683122, 1.000000000000000000, 0.9659258262890683122, 1.000000000000000000, 0.9659258262890683122, 1.000000000000000000, 0.9659258262890683122, 1.000000000000000000, 0.9659258262890683122, 1.000000000000000000, 0.9659258262890683122, 1.000000000000000000, 0.9659258262890683122, 1.000000000000000000, 0.9659258262890683122, 1.000000000000000000, 0.9659258262890683122, 1.000000000000000000, 0.9659258262890683122, 1.000000000000000000, 0.9659258262890683122, 1.000000000000000000, 0.9659258262890683122, 1.000000000000000000, 0.9659258262890683122, 1.000000000000000000, 0.9659258262890683122, 1.000000000000000000, 0.9659258262890683122, 1.000000000000000000, 0.9659258262890683122, 1.000000000000000000, 0.9659258262890683122, 1.000000000000000000, 0.9659258262890683122, 1.000000000000000000, 0.9659258262890683122, 1.000000000000000000, 0.9659258262890683122, 1.000000000000000000, 0.9659258262890683122, 1.000000000000000000, 0.9659258262890683122, 1.000000000000000000, 0.9659258262890683122, 1.000000000000000000, 0.9659258262890683122, 1.000000000000000000, 0.9659258262890683122, 1.000000000000000000, 0.9659258262890683122, 1.000000000000000000, 0.9659258262890683122, 1.000000000000000000, 0.9659258262890683122, 1.000000000000000000, 0.9659258262890683122, 1.000000000000000000, 0.9659258262890683122, 1.000000000000000000, 0.9659258262890683122, 1.000000000000000000, 0.9659258262890683122, 1.000000000000000000, 0.9659258262890683122, 1.000000000000000000, 0.9659258262890683122, 1.000000000000000000, 0.9659258262890683122, 1.000000000000000000, 0.9659258262890683122, 1.000000000000000000, 0.9659258262890683122, 1.000000000000000000, 0.9659258262890683122, 1.000000000000000000, 0.9659258262890683122, 1.000000000000000000, 0.9659258262890683122, 1.000000000000000000, 0.9659258262890683122, 1.000000000000000000, 0.9659258262890683122, 1.000000000000000000, 0.9659258262890683122, 1.000000000000000000, 0.9659258262890683122, 1.000000000000000000, 0.9659258262890683122, 1.000000000000000000, 0.9659258262890683122, 1.000000000000000000, 0.9659258262890683122, 1.000000000000000000, 0.9659258262890683122, 1.000000000000000000, 0.9659258262890683122, 1.000000000000000000, 0.9659258262890683122, 1.000000000000000000, 0.9659258262890683122, 1.000000000000000000, 0.9659258262890683122, 1.000000000000000000, 0.9659258262890683122, 1.000000000000000000, 0.9659258262890683122, 1.000000000000000000, 0.9659258262890683122, 1.000000000000000000, 0.9659258262890683122, 1.000000000000000000, 0.9659258262890683122, 1.000000000000000000, 0.9659258262890683122, 1.000000000000000000, 0.9659258262890683122, 1.000000000000000000, 0.9659258262890683122, 1.000000000000000000, 0.9659258262890683122, 1.000000000000000000, 0.9659258262890683122, 1.000000000000000000, 0.9659258262890683122, 1.000000000000000000, 0.9659258262890683122, 1.000000000000000000, 0.9659258262890683122, 1.000000000000000000, 0.9659258262890683122, 1.000000000000000000, 0.9659258262890683122, 1.000000000000000000, 0.9659258262890683122, 1.000000000000000000, 0.9659258262890683122, 1.000000000000000000, 0.9659258262890683122, 1.000000000000000000, 0.9659258262890683122, 1.000000000000000000, 0.9659258262890683122, 1.000000000000000000, 0.9659258262890683122, 1.000000000000000000, 0.9659258262890683122, 1.000000000000000000, 0.9659258262890683122, 1.000000000000000000, 0.9659258262890683122, 1.000000000000000000, 0.9659258262890683122, 1.000000000000000000, 0.9659258262890683122, 1.000000000000000000, 0.9659258262890683122, 1.000000000000000000, 0.9659258262890683122, 1.000000000000000000, 0.9659258262890683122, 1.000000000000000000, 0.9659258262890683122, 1.000000000000000000, 0.9659258262890683122, 1.000000000000000000, 0.9659258262890683122, 1.000000000000000000, 0.9659258262890683122, 1.000000000000000000, 0.9659258262890683122, 1.000000000000000000, 0.9659258262890683122, 1.000000000000000000, 0.9659258262890683122, 1.000000000000000000, 0.9659258262890683122, 1.000000000000000000, 0.9659258262890683122, 1.000000000000000000, 0.9659258262890683122, 1.000000000000000000, 0.9659258262890683122, 1.000000000000000000, 0.9659258262890683122, 1.000000000000000000, 0.9659258262890683122, 1.000000000000000000, 0.9659258262890683122, 1.000000000000000000, 0.9659258262890683122, 1.000000000000000000, 0.9659258262890683122, 1.000000000000000000, 0.9659258262890683122, 1.000000000000000000, 0.9659258262890683122, 1.000000000000000000, 0.9659258262890683122, 1.000000000000000000, 0.9659258262890683122, 1.000000000000000000, 0.9659258262890683122, 1.000000000000000000, 0.9659258262890683122, 1.000000000000000000, 0.9659258262890683122, 1.000000000000000000, 0.9659258262890683122, 1.000000000000000000, 0.9659258262890683122, 1.000000000000000000, 0.9659258262890683122, 1.000000000000000000, 0.9659258262890683122, 1.000000000000000000, 0.9659258262890683122, 1.000000000000000000, 0.9659258262890683122, 1.000000000000000000, 0.9659258262890683122, 1.000000000000000000, 0.9659258262890683122, 1.000000000000000000, 0.9659258262890683122, 1.000000000000000000, 0.9659258262890683122, 1.000000000000000000, 0.9659258262890683122, 1.000000000000000000, 0.9659258262890683122, 1.000000000000000000, 0.9659258262890683122, 1.000000000000000000, 0.9659258262890683122, 1.000000000000000000, 0.9659258262890683122, 1.000000000000000000, 0.9659258262890683122, 1.000000000000000000, 0.9659258262890683122, 1.000000000000000000, 0.9659258262890683122, 1.000000000000000000, 0.9659258262890683122, 1.000000000000000000, 0.9659258262890683122, 1.000000000000000000, 0.9659258262890683122, 1.000000000000000000, 0.9659258262890683122, 1.000000000000000000, 0.9659258262890683122, 1.000000000000000000, 0.9659258262890683122, 1.000000000000000000, 0.9659258262890683122, 1.000000000000000000, 0.9659258262890683122, 1.000000000000000000, 0.9659258262890683122, 1.000000000000000000, 0.9659258262890683122, 1.000000000000000000, 0.9659258262890683122, 1.000000000000000000, 0.9659258262890683122, 1.000000000000000000, 0.9659258262890683122, 1.000000000000000000, 0.9659258262890683122, 1.000000000000000000, 0.9659258262890683122, 1.000000000000000000, 0.9659258262890683122, 1.000000000000000000, 0.9659258262890683122, 1.000000000000000000, 0.9659258262890683122, 1.000000000000000000, 0.9659258262890683122, 1.000000000000000000, 0.9659258262890683122, 1.000000000000000000, 0.9659258262890683122, 1.000000000000000000, 0.9659258262890683122, 1.000000000000000000, 0.9659258262890683122, 1.000000000000000000, 0.9659258262890683122, 1.000000000000000000, 0.9659258262890683122, 1.000000000000000000, 0.9659258262890683122, 1.000000000000000000, 0.9659258262890683122, 1.000000000000000000, 0.9659258262890683122, 1.000000000000000000, 0.9659258262890683122, 1.000000000000000000, 0.9659258262890683122, 1.000000000000000000, 0.9659258262890683122, 1.000000000000000000, 0.9659258262890683122, 1.000000000000000000, 0.9659258262890683122, 1.000000000000000000, 0.9659258262890683122, 1.000000000000000000, 0.9659258262890683122, 1.000000000000000000),
 ( 0.3333333333333333703, 0.3219752754296894559, 0.3333333333333333703, 0.3219752754296894559, 0.3333333333333333703, 0.3219752754296894559, 0.3333333333333333703, 0.3219752754296894559, 0.3333333333333333703, 0.3219752754296894559, 0.3333333333333333703, 0.3219752754296894559, 0.3333333333333333703, 0.3219752754296894559, 0.3333333333333333703, 0.3219752754296894559, 0.3333333333333333703, 0.3219752754296894559, 0.3333333333333333703, 0.3219752754296894559, 0.3333333333333333703, 0.3219752754296894559, 0.3333333333333333703, 0.3219752754296894559, 0.3333333333333333703, 0.3219752754296894559, 0.3333333333333333703, 0.3219752754296894559, 0.3333333333333333703, 0.3219752754296894559, 0.3333333333333333703, 0.3219752754296894559, 0.3333333333333333703, 0.3219752754296894559, 0.3333333333333333703, 0.3219752754296894559, 0.3333333333333333703, 0.3219752754296894559, 0.3333333333333333703, 0.3219752754296894559, 0.3333333333333333703, 0.3219752754296894559, 0.3333333333333333703, 0.3219752754296894559, 0.3333333333333333703, 0.3219752754296894559, 0.3333333333333333703, 0.3219752754296894559, 0.3333333333333333703, 0.3219752754296894559, 0.3333333333333333703, 0.3219752754296894559, 0.3333333333333333703, 0.3219752754296894559, 0.3333333333333333703, 0.3219752754296894559, 0.3333333333333333703, 0.3219752754296894559, 0.3333333333333333703, 0.3219752754296894559, 0.3333333333333333703, 0.3219752754296894559, 0.3333333333333333703, 0.3219752754296894559, 0.3333333333333333703, 0.3219752754296894559, 0.3333333333333333703, 0.3219752754296894559, 0.3333333333333333703, 0.3219752754296894559, 0.3333333333333333703, 0.3219752754296894559, 0.3333333333333333703, 0.3219752754296894559, 0.3333333333333333703, 0.3219752754296894559, 0.3333333333333333703, 0.3219752754296894559, 0.3333333333333333703, 0.3219752754296894559, 0.3333333333333333703, 0.3219752754296894559, 0.3333333333333333703, 0.3219752754296894559, 0.3333333333333333703, 0.3219752754296894559, 0.3333333333333333703, 0.3219752754296894559, 0.3333333333333333703, 0.3219752754296894559, 0.3333333333333333703, 0.3219752754296894559, 0.3333333333333333703, 0.3219752754296894559, 0.3333333333333333703, 0.3219752754296894559, 0.3333333333333333703, 0.3219752754296894559, 0.3333333333333333703, 0.3219752754296894559, 0.3333333333333333703, 0.3219752754296894559, 0.3333333333333333703, 0.3219752754296894559, 0.3333333333333333703, 0.3219752754296894559, 0.3333333333333333703, 0.3219752754296894559, 0.3333333333333333703, 0.3219752754296894559, 0.3333333333333333703, 0.3219752754296894559, 0.3333333333333333703, 0.3219752754296894559, 0.3333333333333333703, 0.3219752754296894559, 0.3333333333333333703, 0.3219752754296894559, 0.3333333333333333703, 0.3219752754296894559, 0.3333333333333333703, 0.3219752754296894559, 0.3333333333333333703, 0.3219752754296894559, 0.3333333333333333703, 0.3219752754296894559, 0.3333333333333333703, 0.3219752754296894559, 0.3333333333333333703, 0.3219752754296894559, 0.3333333333333333703, 0.3219752754296894559, 0.3333333333333333703, 0.3219752754296894559, 0.3333333333333333703, 0.3219752754296894559, 0.3333333333333333703, 0.3219752754296894559, 0.3333333333333333703, 0.3219752754296894559, 0.3333333333333333703, 0.3219752754296894559, 0.3333333333333333703, 0.3219752754296894559, 0.3333333333333333703, 0.3219752754296894559, 0.3333333333333333703, 0.3219752754296894559, 0.3333333333333333703, 0.3219752754296894559, 0.3333333333333333703, 0.3219752754296894559, 0.3333333333333333703, 0.3219752754296894559, 0.3333333333333333703, 0.3219752754296894559, 0.3333333333333333703, 0.3219752754296894559, 0.3333333333333333703, 0.3219752754296894559, 0.3333333333333333703, 0.3219752754296894559, 0.3333333333333333703, 0.3219752754296894559, 0.3333333333333333703, 0.3219752754296894559, 0.3333333333333333703, 0.3219752754296894559, 0.3333333333333333703, 0.3219752754296894559, 0.3333333333333333703, 0.3219752754296894559, 0.3333333333333333703, 0.3219752754296894559, 0.3333333333333333703, 0.3219752754296894559, 0.3333333333333333703, 0.3219752754296894559, 0.3333333333333333703, 0.3219752754296894559, 0.3333333333333333703, 0.3219752754296894559, 0.3333333333333333703, 0.3219752754296894559, 0.3333333333333333703, 0.3219752754296894559, 0.3333333333333333703, 0.3219752754296894559, 0.3333333333333333703, 0.3219752754296894559, 0.3333333333333333703, 0.3219752754296894559, 0.3333333333333333703, 0.3219752754296894559, 0.3333333333333333703, 0.3219752754296894559, 0.3333333333333333703, 0.3219752754296894559, 0.3333333333333333703, 0.3219752754296894559, 0.3333333333333333703, 0.3219752754296894559, 0.3333333333333333703, 0.3219752754296894559, 0.3333333333333333703, 0.3219752754296894559, 0.3333333333333333703, 0.3219752754296894559, 0.3333333333333333703, 0.3219752754296894559, 0.3333333333333333703, 0.3219752754296894559, 0.3333333333333333703, 0.3219752754296894559, 0.3333333333333333703, 0.3219752754296894559, 0.3333333333333333703, 0.3219752754296894559, 0.3333333333333333703, 0.3219752754296894559, 0.3333333333333333703, 0.3219752754296894559, 0.3333333333333333703, 0.3219752754296894559, 0.3333333333333333703, 0.3219752754296894559, 0.3333333333333333703, 0.3219752754296894559, 0.3333333333333333703, 0.3219752754296894559, 0.3333333333333333703, 0.3219752754296894559, 0.3333333333333333703, 0.3219752754296894559, 0.3333333333333333703, 0.3219752754296894559, 0.3333333333333333703, 0.3219752754296894559, 0.3333333333333333703, 0.3219752754296894559, 0.3333333333333333703, 0.3219752754296894559, 0.3333333333333333703, 0.3219752754296894559, 0.3333333333333333703, 0.3219752754296894559, 0.3333333333333333703, 0.3219752754296894559, 0.3333333333333333703, 0.3219752754296894559, 0.3333333333333333703, 0.3219752754296894559, 0.3333333333333333703, 0.3219752754296894559, 0.3333333333333333703, 0.3219752754296894559, 0.3333333333333333703, 0.3219752754296894559, 0.3333333333333333703, 0.3219752754296894559, 0.3333333333333333703, 0.3219752754296894559, 0.3333333333333333703, 0.3219752754296894559, 0.3333333333333333703, 0.3219752754296894559, 0.3333333333333333703, 0.3219752754296894559, 0.3333333333333333703, 0.3219752754296894559, 0.3333333333333333703, 0.3219752754296894559, 0.3333333333333333703, 0.3219752754296894559, 0.3333333333333333703, 0.3219752754296894559, 0.3333333333333333703, 0.3219752754296894559, 0.3333333333333333703, 0.3219752754296894559, 0.3333333333333333703, 0.3219752754296894559, 0.3333333333333333703, 0.3219752754296894559, 0.3333333333333333703, 0.3219752754296894559, 0.3333333333333333703, 0.3219752754296894559, 0.3333333333333333703, 0.3219752754296894559, 0.3333333333333333703, 0.3219752754296894559, 0.3333333333333333703, 0.3219752754296894559, 0.3333333333333333703, 0.3219752754296894559, 0.3333333333333333703, 0.3219752754296894559, 0.3333333333333333703, 0.3219752754296894559, 0.3333333333333333703, 0.3219752754296894559, 0.3333333333333333703, 0.3219752754296894559, 0.3333333333333333703, 0.3219752754296894559, 0.3333333333333333703, 0.3219752754296894559, 0.3333333333333333703, 0.3219752754296894559, 0.3333333333333333703, 0.3219752754296894559, 0.3333333333333333703, 0.3219752754296894559, 0.3333333333333333703, 0.3219752754296894559, 0.3333333333333333703, 0.3219752754296894559, 0.3333333333333333703, 0.3219752754296894559, 0.3333333333333333703, 0.3219752754296894559, 0.3333333333333333703, 0.3219752754296894559, 0.3333333333333333703, 0.3219752754296894559, 0.3333333333333333703, 0.3219752754296894559, 0.3333333333333333703, 0.3219752754296894559, 0.3333333333333333703, 0.3219752754296894559, 0.3333333333333333703, 0.3219752754296894559, 0.3333333333333333703, 0.3219752754296894559, 0.3333333333333333703, 0.3219752754296894559, 0.3333333333333333703, 0.3219752754296894559, 0.3333333333333333703, 0.3219752754296894559, 0.3333333333333333703, 0.3219752754296894559, 0.3333333333333333703, 0.3219752754296894559, 0.3333333333333333703, 0.3219752754296894559, 0.3333333333333333703, 0.3219752754296894559, 0.3333333333333333703, 0.3219752754296894559, 0.3333333333333333703, 0.3219752754296894559, 0.3333333333333333703, 0.3219752754296894559, 0.3333333333333333703, 0.3219752754296894559, 0.3333333333333333703, 0.3219752754296894559, 0.3333333333333333703, 0.3219752754296894559, 0.3333333333333333703, 0.3219752754296894559, 0.3333333333333333703, 0.3219752754296894559, 0.3333333333333333703, 0.3219752754296894559, 0.3333333333333333703, 0.3219752754296894559, 0.3333333333333333703, 0.3219752754296894559, 0.3333333333333333703, 0.3219752754296894559, 0.3333333333333333703, 0.3219752754296894559, 0.3333333333333333703, 0.3219752754296894559, 0.3333333333333333703, 0.3219752754296894559, 0.3333333333333333703, 0.3219752754296894559, 0.3333333333333333703, 0.3219752754296894559, 0.3333333333333333703),
 ( 0.3333333333333333703, 0.3219752754296894559, 0.3333333333333333703, 0.3219752754296894559, 0.3333333333333333703, 0.3219752754296894559, 0.3333333333333333703, 0.3219752754296894559, 0.3333333333333333703, 0.3219752754296894559, 0.3333333333333333703, 0.3219752754296894559, 0.3333333333333333703, 0.3219752754296894559, 0.3333333333333333703, 0.3219752754296894559, 0.3333333333333333703, 0.3219752754296894559, 0.3333333333333333703, 0.3219752754296894559, 0.3333333333333333703, 0.3219752754296894559, 0.3333333333333333703, 0.3219752754296894559, 0.3333333333333333703, 0.3219752754296894559, 0.3333333333333333703, 0.3219752754296894559, 0.3333333333333333703, 0.3219752754296894559, 0.3333333333333333703, 0.3219752754296894559, 0.3333333333333333703, 0.3219752754296894559, 0.3333333333333333703, 0.3219752754296894559, 0.3333333333333333703, 0.3219752754296894559, 0.3333333333333333703, 0.3219752754296894559, 0.3333333333333333703, 0.3219752754296894559, 0.3333333333333333703, 0.3219752754296894559, 0.3333333333333333703, 0.3219752754296894559, 0.3333333333333333703, 0.3219752754296894559, 0.3333333333333333703, 0.3219752754296894559, 0.3333333333333333703, 0.3219752754296894559, 0.3333333333333333703, 0.3219752754296894559, 0.3333333333333333703, 0.3219752754296894559, 0.3333333333333333703, 0.3219752754296894559, 0.3333333333333333703, 0.3219752754296894559, 0.3333333333333333703, 0.3219752754296894559, 0.3333333333333333703, 0.3219752754296894559, 0.3333333333333333703, 0.3219752754296894559, 0.3333333333333333703, 0.3219752754296894559, 0.3333333333333333703, 0.3219752754296894559, 0.3333333333333333703, 0.3219752754296894559, 0.3333333333333333703, 0.3219752754296894559, 0.3333333333333333703, 0.3219752754296894559, 0.3333333333333333703, 0.3219752754296894559, 0.3333333333333333703, 0.3219752754296894559, 0.3333333333333333703, 0.3219752754296894559, 0.3333333333333333703, 0.3219752754296894559, 0.3333333333333333703, 0.3219752754296894559, 0.3333333333333333703, 0.3219752754296894559, 0.3333333333333333703, 0.3219752754296894559, 0.3333333333333333703, 0.3219752754296894559, 0.3333333333333333703, 0.3219752754296894559, 0.3333333333333333703, 0.3219752754296894559, 0.3333333333333333703, 0.3219752754296894559, 0.3333333333333333703, 0.3219752754296894559, 0.3333333333333333703, 0.3219752754296894559, 0.3333333333333333703, 0.3219752754296894559, 0.3333333333333333703, 0.3219752754296894559, 0.3333333333333333703, 0.3219752754296894559, 0.3333333333333333703, 0.3219752754296894559, 0.3333333333333333703, 0.3219752754296894559, 0.3333333333333333703, 0.3219752754296894559, 0.3333333333333333703, 0.3219752754296894559, 0.3333333333333333703, 0.3219752754296894559, 0.3333333333333333703, 0.3219752754296894559, 0.3333333333333333703, 0.3219752754296894559, 0.3333333333333333703, 0.3219752754296894559, 0.3333333333333333703, 0.3219752754296894559, 0.3333333333333333703, 0.3219752754296894559, 0.3333333333333333703, 0.3219752754296894559, 0.3333333333333333703, 0.3219752754296894559, 0.3333333333333333703, 0.3219752754296894559, 0.3333333333333333703, 0.3219752754296894559, 0.3333333333333333703, 0.3219752754296894559, 0.3333333333333333703, 0.3219752754296894559, 0.3333333333333333703, 0.3219752754296894559, 0.3333333333333333703, 0.3219752754296894559, 0.3333333333333333703, 0.3219752754296894559, 0.3333333333333333703, 0.3219752754296894559, 0.3333333333333333703, 0.3219752754296894559, 0.3333333333333333703, 0.3219752754296894559, 0.3333333333333333703, 0.3219752754296894559, 0.3333333333333333703, 0.3219752754296894559, 0.3333333333333333703, 0.3219752754296894559, 0.3333333333333333703, 0.3219752754296894559, 0.3333333333333333703, 0.3219752754296894559, 0.3333333333333333703, 0.3219752754296894559, 0.3333333333333333703, 0.3219752754296894559, 0.3333333333333333703, 0.3219752754296894559, 0.3333333333333333703, 0.3219752754296894559, 0.3333333333333333703, 0.3219752754296894559, 0.3333333333333333703, 0.3219752754296894559, 0.3333333333333333703, 0.3219752754296894559, 0.3333333333333333703, 0.3219752754296894559, 0.3333333333333333703, 0.3219752754296894559, 0.3333333333333333703, 0.3219752754296894559, 0.3333333333333333703, 0.3219752754296894559, 0.3333333333333333703, 0.3219752754296894559, 0.3333333333333333703, 0.3219752754296894559, 0.3333333333333333703, 0.3219752754296894559, 0.3333333333333333703, 0.3219752754296894559, 0.3333333333333333703, 0.3219752754296894559, 0.3333333333333333703, 0.3219752754296894559, 0.3333333333333333703, 0.3219752754296894559, 0.3333333333333333703, 0.3219752754296894559, 0.3333333333333333703, 0.3219752754296894559, 0.3333333333333333703, 0.3219752754296894559, 0.3333333333333333703, 0.3219752754296894559, 0.3333333333333333703, 0.3219752754296894559, 0.3333333333333333703, 0.3219752754296894559, 0.3333333333333333703, 0.3219752754296894559, 0.3333333333333333703, 0.3219752754296894559, 0.3333333333333333703, 0.3219752754296894559, 0.3333333333333333703, 0.3219752754296894559, 0.3333333333333333703, 0.3219752754296894559, 0.3333333333333333703, 0.3219752754296894559, 0.3333333333333333703, 0.3219752754296894559, 0.3333333333333333703, 0.3219752754296894559, 0.3333333333333333703, 0.3219752754296894559, 0.3333333333333333703, 0.3219752754296894559, 0.3333333333333333703, 0.3219752754296894559, 0.3333333333333333703, 0.3219752754296894559, 0.3333333333333333703, 0.3219752754296894559, 0.3333333333333333703, 0.3219752754296894559, 0.3333333333333333703, 0.3219752754296894559, 0.3333333333333333703, 0.3219752754296894559, 0.3333333333333333703, 0.3219752754296894559, 0.3333333333333333703, 0.3219752754296894559, 0.3333333333333333703, 0.3219752754296894559, 0.3333333333333333703, 0.3219752754296894559, 0.3333333333333333703, 0.3219752754296894559, 0.3333333333333333703, 0.3219752754296894559, 0.3333333333333333703, 0.3219752754296894559, 0.3333333333333333703, 0.3219752754296894559, 0.3333333333333333703, 0.3219752754296894559, 0.3333333333333333703, 0.3219752754296894559, 0.3333333333333333703, 0.3219752754296894559, 0.3333333333333333703, 0.3219752754296894559, 0.3333333333333333703, 0.3219752754296894559, 0.3333333333333333703, 0.3219752754296894559, 0.3333333333333333703, 0.3219752754296894559, 0.3333333333333333703, 0.3219752754296894559, 0.3333333333333333703, 0.3219752754296894559, 0.3333333333333333703, 0.3219752754296894559, 0.3333333333333333703, 0.3219752754296894559, 0.3333333333333333703, 0.3219752754296894559, 0.3333333333333333703, 0.3219752754296894559, 0.3333333333333333703, 0.3219752754296894559, 0.3333333333333333703, 0.3219752754296894559, 0.3333333333333333703, 0.3219752754296894559, 0.3333333333333333703, 0.3219752754296894559, 0.3333333333333333703, 0.3219752754296894559, 0.3333333333333333703, 0.3219752754296894559, 0.3333333333333333703, 0.3219752754296894559, 0.3333333333333333703, 0.3219752754296894559, 0.3333333333333333703, 0.3219752754296894559, 0.3333333333333333703, 0.3219752754296894559, 0.3333333333333333703, 0.3219752754296894559, 0.3333333333333333703, 0.3219752754296894559, 0.3333333333333333703, 0.3219752754296894559, 0.3333333333333333703, 0.3219752754296894559, 0.3333333333333333703, 0.3219752754296894559, 0.3333333333333333703, 0.3219752754296894559, 0.3333333333333333703, 0.3219752754296894559, 0.3333333333333333703, 0.3219752754296894559, 0.3333333333333333703, 0.3219752754296894559, 0.3333333333333333703, 0.3219752754296894559, 0.3333333333333333703, 0.3219752754296894559, 0.3333333333333333703, 0.3219752754296894559, 0.3333333333333333703, 0.3219752754296894559, 0.3333333333333333703, 0.3219752754296894559, 0.3333333333333333703, 0.3219752754296894559, 0.3333333333333333703, 0.3219752754296894559, 0.3333333333333333703, 0.3219752754296894559, 0.3333333333333333703, 0.3219752754296894559, 0.3333333333333333703, 0.3219752754296894559, 0.3333333333333333703, 0.3219752754296894559, 0.3333333333333333703, 0.3219752754296894559, 0.3333333333333333703, 0.3219752754296894559, 0.3333333333333333703, 0.3219752754296894559, 0.3333333333333333703, 0.3219752754296894559, 0.3333333333333333703, 0.3219752754296894559, 0.3333333333333333703, 0.3219752754296894559, 0.3333333333333333703, 0.3219752754296894559, 0.3333333333333333703, 0.3219752754296894559, 0.3333333333333333703, 0.3219752754296894559, 0.3333333333333333703, 0.3219752754296894559, 0.3333333333333333703, 0.3219752754296894559, 0.3333333333333333703, 0.3219752754296894559, 0.3333333333333333703, 0.3219752754296894559, 0.3333333333333333703, 0.3219752754296894559, 0.3333333333333333703, 0.3219752754296894559, 0.3333333333333333703, 0.3219752754296894559, 0.3333333333333333703, 0.3219752754296894559, 0.3333333333333333703, 0.3219752754296894559, 0.3333333333333333703, 0.3219752754296894559, 0.3333333333333333703, 0.3219752754296894559, 0.3333333333333333703),
 ( 1.000000000000000000, 0.9659258262890683122, 1.000000000000000000, 0.9659258262890683122, 1.000000000000000000, 0.9659258262890683122, 1.000000000000000000, 0.9659258262890683122, 1.000000000000000000, 0.9659258262890683122, 1.000000000000000000, 0.9659258262890683122, 1.000000000000000000, 0.9659258262890683122, 1.000000000000000000, 0.9659258262890683122, 1.000000000000000000, 0.9659258262890683122, 1.000000000000000000, 0.9659258262890683122, 1.000000000000000000, 0.9659258262890683122, 1.000000000000000000, 0.9659258262890683122, 1.000000000000000000, 0.9659258262890683122, 1.000000000000000000, 0.9659258262890683122, 1.000000000000000000, 0.9659258262890683122, 1.000000000000000000, 0.9659258262890683122, 1.000000000000000000, 0.9659258262890683122, 1.000000000000000000, 0.9659258262890683122, 1.000000000000000000, 0.9659258262890683122, 1.000000000000000000, 0.9659258262890683122, 1.000000000000000000, 0.9659258262890683122, 1.000000000000000000, 0.9659258262890683122, 1.000000000000000000, 0.9659258262890683122, 1.000000000000000000, 0.9659258262890683122, 1.000000000000000000, 0.9659258262890683122, 1.000000000000000000, 0.9659258262890683122, 1.000000000000000000, 0.9659258262890683122, 1.000000000000000000, 0.9659258262890683122, 1.000000000000000000, 0.9659258262890683122, 1.000000000000000000, 0.9659258262890683122, 1.000000000000000000, 0.9659258262890683122, 1.000000000000000000, 0.9659258262890683122, 1.000000000000000000, 0.9659258262890683122, 1.000000000000000000, 0.9659258262890683122, 1.000000000000000000, 0.9659258262890683122, 1.000000000000000000, 0.9659258262890683122, 1.000000000000000000, 0.9659258262890683122, 1.000000000000000000, 0.9659258262890683122, 1.000000000000000000, 0.9659258262890683122, 1.000000000000000000, 0.9659258262890683122, 1.000000000000000000, 0.9659258262890683122, 1.000000000000000000, 0.9659258262890683122, 1.000000000000000000, 0.9659258262890683122, 1.000000000000000000, 0.9659258262890683122, 1.000000000000000000, 0.9659258262890683122, 1.000000000000000000, 0.9659258262890683122, 1.000000000000000000, 0.9659258262890683122, 1.000000000000000000, 0.9659258262890683122, 1.000000000000000000, 0.9659258262890683122, 1.000000000000000000, 0.9659258262890683122, 1.000000000000000000, 0.9659258262890683122, 1.000000000000000000, 0.9659258262890683122, 1.000000000000000000, 0.9659258262890683122, 1.000000000000000000, 0.9659258262890683122, 1.000000000000000000, 0.9659258262890683122, 1.000000000000000000, 0.9659258262890683122, 1.000000000000000000, 0.9659258262890683122, 1.000000000000000000, 0.9659258262890683122, 1.000000000000000000, 0.9659258262890683122, 1.000000000000000000, 0.9659258262890683122, 1.000000000000000000, 0.9659258262890683122, 1.000000000000000000, 0.9659258262890683122, 1.000000000000000000, 0.9659258262890683122, 1.000000000000000000, 0.9659258262890683122, 1.000000000000000000, 0.9659258262890683122, 1.000000000000000000, 0.9659258262890683122, 1.000000000000000000, 0.9659258262890683122, 1.000000000000000000, 0.9659258262890683122, 1.000000000000000000, 0.9659258262890683122, 1.000000000000000000, 0.9659258262890683122, 1.000000000000000000, 0.9659258262890683122, 1.000000000000000000, 0.9659258262890683122, 1.000000000000000000, 0.9659258262890683122, 1.000000000000000000, 0.9659258262890683122, 1.000000000000000000, 0.9659258262890683122, 1.000000000000000000, 0.9659258262890683122, 1.000000000000000000, 0.9659258262890683122, 1.000000000000000000, 0.9659258262890683122, 1.000000000000000000, 0.9659258262890683122, 1.000000000000000000, 0.9659258262890683122, 1.000000000000000000, 0.9659258262890683122, 1.000000000000000000, 0.9659258262890683122, 1.000000000000000000, 0.9659258262890683122, 1.000000000000000000, 0.9659258262890683122, 1.000000000000000000, 0.9659258262890683122, 1.000000000000000000, 0.9659258262890683122, 1.000000000000000000, 0.9659258262890683122, 1.000000000000000000, 0.9659258262890683122, 1.000000000000000000, 0.9659258262890683122, 1.000000000000000000, 0.9659258262890683122, 1.000000000000000000, 0.9659258262890683122, 1.000000000000000000, 0.9659258262890683122, 1.000000000000000000, 0.9659258262890683122, 1.000000000000000000, 0.9659258262890683122, 1.000000000000000000, 0.9659258262890683122, 1.000000000000000000, 0.9659258262890683122, 1.000000000000000000, 0.9659258262890683122, 1.000000000000000000, 0.9659258262890683122, 1.000000000000000000, 0.9659258262890683122, 1.000000000000000000, 0.9659258262890683122, 1.000000000000000000, 0.9659258262890683122, 1.000000000000000000, 0.9659258262890683122, 1.000000000000000000, 0.9659258262890683122, 1.000000000000000000, 0.9659258262890683122, 1.000000000000000000, 0.9659258262890683122, 1.000000000000000000, 0.9659258262890683122, 1.000000000000000000, 0.9659258262890683122, 1.000000000000000000, 0.9659258262890683122, 1.000000000000000000, 0.9659258262890683122, 1.000000000000000000, 0.9659258262890683122, 1.000000000000000000, 0.9659258262890683122, 1.000000000000000000, 0.9659258262890683122, 1.000000000000000000, 0.9659258262890683122, 1.000000000000000000, 0.9659258262890683122, 1.000000000000000000, 0.9659258262890683122, 1.000000000000000000, 0.9659258262890683122, 1.000000000000000000, 0.9659258262890683122, 1.000000000000000000, 0.9659258262890683122, 1.000000000000000000, 0.9659258262890683122, 1.000000000000000000, 0.9659258262890683122, 1.000000000000000000, 0.9659258262890683122, 1.000000000000000000, 0.9659258262890683122, 1.000000000000000000, 0.9659258262890683122, 1.000000000000000000, 0.9659258262890683122, 1.000000000000000000, 0.9659258262890683122, 1.000000000000000000, 0.9659258262890683122, 1.000000000000000000, 0.9659258262890683122, 1.000000000000000000, 0.9659258262890683122, 1.000000000000000000, 0.9659258262890683122, 1.000000000000000000, 0.9659258262890683122, 1.000000000000000000, 0.9659258262890683122, 1.000000000000000000, 0.9659258262890683122, 1.000000000000000000, 0.9659258262890683122, 1.000000000000000000, 0.9659258262890683122, 1.000000000000000000, 0.9659258262890683122, 1.000000000000000000, 0.9659258262890683122, 1.000000000000000000, 0.9659258262890683122, 1.000000000000000000, 0.9659258262890683122, 1.000000000000000000, 0.9659258262890683122, 1.000000000000000000, 0.9659258262890683122, 1.000000000000000000, 0.9659258262890683122, 1.000000000000000000, 0.9659258262890683122, 1.000000000000000000, 0.9659258262890683122, 1.000000000000000000, 0.9659258262890683122, 1.000000000000000000, 0.9659258262890683122, 1.000000000000000000, 0.9659258262890683122, 1.000000000000000000, 0.9659258262890683122, 1.000000000000000000, 0.9659258262890683122, 1.000000000000000000, 0.9659258262890683122, 1.000000000000000000, 0.9659258262890683122, 1.000000000000000000, 0.9659258262890683122, 1.000000000000000000, 0.9659258262890683122, 1.000000000000000000, 0.9659258262890683122, 1.000000000000000000, 0.9659258262890683122, 1.000000000000000000, 0.9659258262890683122, 1.000000000000000000, 0.9659258262890683122, 1.000000000000000000, 0.9659258262890683122, 1.000000000000000000, 0.9659258262890683122, 1.000000000000000000, 0.9659258262890683122, 1.000000000000000000, 0.9659258262890683122, 1.000000000000000000, 0.9659258262890683122, 1.000000000000000000, 0.9659258262890683122, 1.000000000000000000, 0.9659258262890683122, 1.000000000000000000, 0.9659258262890683122, 1.000000000000000000, 0.9659258262890683122, 1.000000000000000000, 0.9659258262890683122, 1.000000000000000000, 0.9659258262890683122, 1.000000000000000000, 0.9659258262890683122, 1.000000000000000000, 0.9659258262890683122, 1.000000000000000000, 0.9659258262890683122, 1.000000000000000000, 0.9659258262890683122, 1.000000000000000000, 0.9659258262890683122, 1.000000000000000000, 0.9659258262890683122, 1.000000000000000000, 0.9659258262890683122, 1.000000000000000000, 0.9659258262890683122, 1.000000000000000000, 0.9659258262890683122, 1.000000000000000000, 0.9659258262890683122, 1.000000000000000000, 0.9659258262890683122, 1.000000000000000000, 0.9659258262890683122, 1.000000000000000000, 0.9659258262890683122, 1.000000000000000000, 0.9659258262890683122, 1.000000000000000000, 0.9659258262890683122, 1.000000000000000000, 0.9659258262890683122, 1.000000000000000000, 0.9659258262890683122, 1.000000000000000000, 0.9659258262890683122, 1.000000000000000000, 0.9659258262890683122, 1.000000000000000000, 0.9659258262890683122, 1.000000000000000000, 0.9659258262890683122, 1.000000000000000000, 0.9659258262890683122, 1.000000000000000000, 0.9659258262890683122, 1.000000000000000000, 0.9659258262890683122, 1.000000000000000000, 0.9659258262890683122, 1.000000000000000000) ) ) 
 REPRESENTATION_ITEM ( '' )  SURFACE ( )  );
#22910 = CARTESIAN_POINT ( 'NONE',  ( -15.14183272437242600, 13.29999999999998650, 20.84094480462497856 ) ) ;
#22911 = CARTESIAN_POINT ( 'NONE',  ( -4.523095164977117273E-15, 2.624999997268825602, 24.62258325217400312 ) ) ;
#22912 = CARTESIAN_POINT ( 'NONE',  ( 10.37757302488624056, 12.52500000273118452, -31.93888565452638417 ) ) ;
#22913 = CARTESIAN_POINT ( 'NONE',  ( 26.29305231718578995, 29.20000000000000284, -19.10302069950538240 ) ) ;
#22914 = CARTESIAN_POINT ( 'NONE',  ( -7.468012846824272799, 54.10378499907602645, 28.02196122052058413 ) ) ;
#22915 = CARTESIAN_POINT ( 'NONE',  ( 15.00000000000000000, 77.09999999999998010, -4.873795443493596835 ) ) ;
#22916 = CARTESIAN_POINT ( 'NONE',  ( 12.13525491562420910, 81.19999999999998863, -8.816778784387098611 ) ) ;
#22917 = CARTESIAN_POINT ( 'NONE',  ( 26.29305231718579350, 54.80000000000000426, 19.10302069950537529 ) ) ;
#22918 = CARTESIAN_POINT ( 'NONE',  ( -15.00000000000000000, 74.25000000546239676, 0.000000000000000000 ) ) ;
#22919 = CARTESIAN_POINT ( 'NONE',  ( -19.82091636218621034, 12.54999999453762527, -14.40073868116559552 ) ) ;
#22920 = CARTESIAN_POINT ( 'NONE',  ( 15.00000000000000000, 79.25000000546239676, -1.836970198721029589E-15 ) ) ;
#22921 = CARTESIAN_POINT ( 'NONE',  ( -24.20753774853730889, 25.03385416666666785, 13.97622843553633842 ) ) ;
#22922 = CARTESIAN_POINT ( 'NONE',  ( -27.16883889988624290, 30.92500000273118488, -19.73931689729374028 ) ) ;
#22923 = CARTESIAN_POINT ( 'NONE',  ( 12.13525491562420910, 75.19999999999998863, -8.816778784387098611 ) ) ;
#22924 = CARTESIAN_POINT ( 'NONE',  ( 33.58253175000000823, 42.27500000273118275, 10.91162601494192863 ) ) ;
#22925 = CARTESIAN_POINT ( 'NONE',  ( 10.37757302488624056, 18.77500000273118985, -31.93888565452638417 ) ) ;
#22926 = CARTESIAN_POINT ( 'NONE',  ( 33.58253175000000113, 74.12500000273119838, -4.112674001490185761E-15 ) ) ;
#22927 = AXIS2_PLACEMENT_3D ( 'NONE', #19836, #22578, #17102 ) ;
#22928 = CARTESIAN_POINT ( 'NONE',  ( 15.00000000000000355, 80.89999999999997726, 4.873795443493592394 ) ) ;
#22929 = CARTESIAN_POINT ( 'NONE',  ( 10.04305231718578817, 59.39999999999999147, -30.90933677959249337 ) ) ;
#22930 = CARTESIAN_POINT ( 'NONE',  ( 0.000000000000000000, 80.00000000000001421, 0.000000000000000000 ) ) ;
#22931 = CARTESIAN_POINT ( 'NONE',  ( 6.486482029760648627E-15, 63.62500000273117706, 35.31076352940722529 ) ) ;
#22932 = CARTESIAN_POINT ( 'NONE',  ( -7.236395654485763274, 2.524999997268823293, 22.27133577429736633 ) ) ;
#22933 = CARTESIAN_POINT ( 'NONE',  ( -7.025853678916861966, 38.34857666574267654, -26.06988505166722803 ) ) ;
#22934 = CARTESIAN_POINT ( 'NONE',  ( -20.75514604977248823, 79.07500000273121543, -28.56700777964554305 ) ) ;
#22935 = CARTESIAN_POINT ( 'NONE',  ( 33.58253175000000113, 4.225000002731190918, -10.91162601494193574 ) ) ;
#22936 = CARTESIAN_POINT ( 'NONE',  ( -7.236395654485763274, 10.52499999726880198, 22.27133577429736633 ) ) ;
#22937 = CARTESIAN_POINT ( 'NONE',  ( -13.97622843553632421, 60.26822916666665009, -24.20753774853731599 ) ) ;
#22938 = ORIENTED_EDGE ( 'NONE', *, *, #16089, .F. ) ;
#22939 = CARTESIAN_POINT ( 'NONE',  ( -2.162160676586881955E-15, 48.62500000273118417, -35.31076352940723240 ) ) ;
#22940 = CARTESIAN_POINT ( 'NONE',  ( -33.58253175000000113, 21.47500000273119980, 10.91162601494193929 ) ) ;
#22941 = ORIENTED_EDGE ( 'NONE', *, *, #8724, .T. ) ;
#22942 = CARTESIAN_POINT ( 'NONE',  ( -15.01150461594642138, 36.20572916666666430, -26.00068869287340334 ) ) ;
#22943 = CARTESIAN_POINT ( 'NONE',  ( 25.98046417659858420, 28.76340250092398065, 15.04653450569292872 ) ) ;
#22944 = CARTESIAN_POINT ( 'NONE',  ( 5.878266837044421923E-15, -70.99969134886156041, 0.000000000000000000 ) ) ;
#22945 = CARTESIAN_POINT ( 'NONE',  ( 3.245314017740486554E-15, -20.99999999999998934, 26.50000000000000355 ) ) ;
#22946 = CARTESIAN_POINT ( 'NONE',  ( 1.507698388325705758E-15, 3.624999997268822938, -24.62258325217400312 ) ) ;
#22947 = CARTESIAN_POINT ( 'NONE',  ( -7.236395654485757944, 13.22499999726881015, -22.27133577429736988 ) ) ;
#22948 = CARTESIAN_POINT ( 'NONE',  ( 20.75514604977248467, 18.67500000273120264, -28.56700777964554305 ) ) ;
#22949 = CARTESIAN_POINT ( 'NONE',  ( 32.50000000000000000, 23.50000000546237544, -3.980102097228898626E-15 ) ) ;
#22950 = CARTESIAN_POINT ( 'NONE',  ( 26.29305231718578995, 67.19999999999998863, -19.10302069950538240 ) ) ;
#22951 = CARTESIAN_POINT ( 'NONE',  ( 2.375766604868043252, 77.69874572391552192, -14.99999999999999822 ) ) ;
#22952 = CARTESIAN_POINT ( 'NONE',  ( -14.93337011119329993, 67.00000000000000000, -30.15969763299878892 ) ) ;
#22953 = CARTESIAN_POINT ( 'NONE',  ( -20.47846945139902175, 65.00038166759063074, -20.53372385742072481 ) ) ;
#22954 = CARTESIAN_POINT ( 'NONE',  ( -10.37757302488624411, 26.97500000273117493, -31.93888565452638417 ) ) ;
#22955 = CARTESIAN_POINT ( 'NONE',  ( 32.50000000000000000, 43.50000000546238965, -3.980102097228898626E-15 ) ) ;
#22956 = CARTESIAN_POINT ( 'NONE',  ( 20.50609665440969565, 26.60937499999999645, -20.50609665441004736 ) ) ;
#22957 = SURFACE_STYLE_USAGE ( .BOTH. , #20045 ) ;
#22958 = CARTESIAN_POINT ( 'NONE',  ( 14.47279130897151767, 17.42499999726882365, -19.92008829642072598 ) ) ;
#22959 = CARTESIAN_POINT ( 'NONE',  ( -20.08610463437157989, 7.699999999999988631, -27.64615127144129758 ) ) ;
#22960 = CARTESIAN_POINT ( 'NONE',  ( 7.570916362186207671, 17.60000000000000497, 23.30088464923126779 ) ) ;
#22961 = CARTESIAN_POINT ( 'NONE',  ( -7.025853678916861966, 48.66107666574268364, -26.06988505166722803 ) ) ;
#22962 = CARTESIAN_POINT ( 'NONE',  ( 20.75514604977249178, 47.82500000273117990, 28.56700777964553950 ) ) ;
#22963 = CARTESIAN_POINT ( 'NONE',  ( -33.58253175000000113, 63.47500000273117138, 10.91162601494193929 ) ) ;
#22964 = CARTESIAN_POINT ( 'NONE',  ( -33.58253175000000113, 43.27500000273117564, -10.91162601494193041 ) ) ;
#22965 = CYLINDRICAL_SURFACE ( 'NONE', #17839, 32.50000000000000000 ) ;
#22966 = CARTESIAN_POINT ( 'NONE',  ( -14.45873412499999944, 81.68750000136559208, 0.000000000000000000 ) ) ;
#22967 = LINE ( 'NONE', #9923, #23477 ) ;
#22968 = CARTESIAN_POINT ( 'NONE',  ( 5.147494310547380714, 63.05125428700923607, 32.50000000000002132 ) ) ;
#22969 = CARTESIAN_POINT ( 'NONE',  ( 4.445600272181915325E-13, 27.50000000000000355, -32.50000000000000000 ) ) ;
#22970 = CARTESIAN_POINT ( 'NONE',  ( -33.58253175000000113, 23.22500000273117138, 10.91162601494193929 ) ) ;
#22971 = CARTESIAN_POINT ( 'NONE',  ( -20.08610463437157989, 62.20000000546237118, -27.64615127144129758 ) ) ;
#22972 = DIRECTION ( 'NONE',  ( 0.000000000000000000, -1.000000000000000000, 0.000000000000000000 ) ) ;
#22973 = DIRECTION ( 'NONE',  ( 0.000000000000000000, -1.000000000000000000, 0.000000000000000000 ) ) ;
#22974 = CARTESIAN_POINT ( 'NONE',  ( 26.02091320914876960, 67.13763916574266943, 14.97647472619900455 ) ) ;
#22975 = CARTESIAN_POINT ( 'NONE',  ( -32.50000000000000000, 40.50000000546237544, 0.000000000000000000 ) ) ;
#22976 = CARTESIAN_POINT ( 'NONE',  ( 9.270509831248421762, 71.55000000546239391, -12.75976212528059861 ) ) ;
#22977 = CARTESIAN_POINT ( 'NONE',  ( 20.75514604977248467, 34.42500000273116711, -28.56700777964554305 ) ) ;
#22978 = CARTESIAN_POINT ( 'NONE',  ( 27.16883889988623935, 64.57500000273120122, -19.73931689729374384 ) ) ;
#22979 = CARTESIAN_POINT ( 'NONE',  ( -24.20753774853756823, 32.48177083333332860, -13.97622843553588723 ) ) ;
#22980 = VERTEX_POINT ( 'NONE', #11973 ) ;
#22981 = CARTESIAN_POINT ( 'NONE',  ( 33.58253175000000113, 72.12500000273118417, -4.112674001490185761E-15 ) ) ;
#22982 = CARTESIAN_POINT ( 'NONE',  ( 28.01184896238290278, 37.20833333333332860, -7.505752307973347470 ) ) ;
#22983 = CARTESIAN_POINT ( 'NONE',  ( -32.50000000000000000, 16.40000000546239178, -10.55989012756945300 ) ) ;
#22984 = ORIENTED_EDGE ( 'NONE', *, *, #29234, .F. ) ;
#22985 = CARTESIAN_POINT ( 'NONE',  ( 7.543491769121427382, 58.69829833425730925, -28.00173670424548433 ) ) ;
#22986 = CARTESIAN_POINT ( 'NONE',  ( 27.95245687107223986, 62.85194416759064495, 0.04044903254993640479 ) ) ;
#22987 = ORIENTED_EDGE ( 'NONE', *, *, #22423, .T. ) ;
#22988 = CARTESIAN_POINT ( 'NONE',  ( 33.58253175000000823, 10.02500000273118275, 10.91162601494192863 ) ) ;
#22989 = CARTESIAN_POINT ( 'NONE',  ( -25.98046417659831420, 20.15847249907602290, 15.04653450569339945 ) ) ;
#22990 = CARTESIAN_POINT ( 'NONE',  ( 12.13525491562421088, 79.05000000546236549, 8.816778784387095058 ) ) ;
#22991 = CARTESIAN_POINT ( 'NONE',  ( -20.75514604977248112, 31.67500000273119909, 28.56700777964554661 ) ) ;
#22992 = CARTESIAN_POINT ( 'NONE',  ( -32.50000000000000000, 44.50000000546238965, 0.000000000000000000 ) ) ;
#22993 = CARTESIAN_POINT ( 'NONE',  ( -4.635254915624211769, 75.59999999999999432, -14.26584774442730286 ) ) ;
#22994 = CARTESIAN_POINT ( 'NONE',  ( -10.37757302488623701, 25.52500000273119696, 31.93888565452638417 ) ) ;
#22995 = CARTESIAN_POINT ( 'NONE',  ( -1.778240108872766143E-15, 32.00000000546237544, -32.49999999999999289 ) ) ;
#22996 = CARTESIAN_POINT ( 'NONE',  ( 10.37757302488624056, 48.77500000273118985, -31.93888565452638417 ) ) ;
#22997 = ADVANCED_BREP_SHAPE_REPRESENTATION ( '', ( #9552, #1376 ), #21134 ) ;
#22998 = EDGE_CURVE ( 'NONE', #7660, #18399, #1333, .T. ) ;
#22999 = CARTESIAN_POINT ( 'NONE',  ( 20.08610463437157279, 31.30000000000000071, -27.64615127144129758 ) ) ;
#23000 = CARTESIAN_POINT ( 'NONE',  ( -20.08610463437157989, 25.70000000000000284, -27.64615127144129758 ) ) ;
#23001 = CARTESIAN_POINT ( 'NONE',  ( 23.41746825000000243, 18.52499999726881441, 7.608796670333735079 ) ) ;
#23002 = CARTESIAN_POINT ( 'NONE',  ( -2.162160676586881955E-15, 74.62500000273116996, -35.31076352940723240 ) ) ;
#23003 = CARTESIAN_POINT ( 'NONE',  ( -5.147494310547430452, 70.05125428700921475, -32.49999999999999289 ) ) ;
#23004 = CARTESIAN_POINT ( 'NONE',  ( -15.14183272437242778, 15.30000000000001137, 20.84094480462497856 ) ) ;
#23005 = CARTESIAN_POINT ( 'NONE',  ( -10.37757302488623701, 59.77500000273119696, 31.93888565452638417 ) ) ;
#23006 = CARTESIAN_POINT ( 'NONE',  ( -9.270509831248421762, 74.55000000546239391, 12.75976212528060039 ) ) ;
#23007 = EDGE_CURVE ( 'NONE', #22660, #1605, #27006, .T. ) ;
#23008 = ADVANCED_FACE ( 'NONE', ( #25537 ), #2016, .T. ) ;
#23009 = DIRECTION ( 'NONE',  ( 0.000000000000000000, -1.000000000000000000, 0.000000000000000000 ) ) ;
#23010 = CARTESIAN_POINT ( 'NONE',  ( 27.16883889988624290, 17.92500000273117422, 19.73931689729373673 ) ) ;
#23011 = CARTESIAN_POINT ( 'NONE',  ( 1.577395562988744260E-15, 10.24999999453763877, -25.76082449383753925 ) ) ;
#23012 = CARTESIAN_POINT ( 'NONE',  ( -13.94119854578936923, 23.89361083425731280, -24.22776226481241224 ) ) ;
#23013 =( BOUNDED_CURVE ( )  B_SPLINE_CURVE ( 2, ( #26056, #30675, #17829, #20235, #20755, #13016, #4943, #5290, #10440, #15079, #20401, #15772, #22969 ),
 .UNSPECIFIED., .F., .T. ) 
 B_SPLINE_CURVE_WITH_KNOTS ( ( 3, 2, 2, 2, 2, 2, 3 ),
 ( 0.6602564102564102422, 0.6615384615384615197, 0.6641025641025640747, 0.6666666666666666297, 0.6692307692307691847, 0.6717948717948717396, 0.6730769230769231282 ),
 .UNSPECIFIED. ) 
 CURVE ( )  GEOMETRIC_REPRESENTATION_ITEM ( )  RATIONAL_B_SPLINE_CURVE ( ( 0.9755282581475768211, 0.9755282581475768211, 1.000000000000000000, 0.9510565162951535312, 1.000000000000000000, 0.9510565162951535312, 1.000000000000000000, 0.9510565162951535312, 1.000000000000000000, 0.9510565162951535312, 1.000000000000000000, 0.9755282581475757109, 0.9755282581475768211 ) ) 
 REPRESENTATION_ITEM ( '' )  );
#23014 = CARTESIAN_POINT ( 'NONE',  ( 33.58253175000000113, 44.12500000273119127, -4.112674001490185761E-15 ) ) ;
#23015 = CARTESIAN_POINT ( 'NONE',  ( 23.95873412499999944, 0.3124999986344190184, 0.000000000000000000 ) ) ;
#23016 = CARTESIAN_POINT ( 'NONE',  ( 6.486482029760648627E-15, 53.87500000273119127, 35.31076352940722529 ) ) ;
#23017 = CARTESIAN_POINT ( 'NONE',  ( 0.04044903254992426173, 44.80506916759064495, -30.02300923189239867 ) ) ;
#23018 = CARTESIAN_POINT ( 'NONE',  ( 0.000000000000000000, 122.0000000000000000, 10.64101615137753676 ) ) ;
#23019 = CARTESIAN_POINT ( 'NONE',  ( 28.02196122052058413, 39.49440999907601224, 7.468012846824272799 ) ) ;
#23020 = CARTESIAN_POINT ( 'NONE',  ( 10.04305231718578817, 59.90000000546237402, -30.90933677959249337 ) ) ;
#23021 = CARTESIAN_POINT ( 'NONE',  ( -8.960552108402742093E-16, 74.37500000273121259, -14.63369212191046387 ) ) ;
#23022 = CARTESIAN_POINT ( 'NONE',  ( 7.570916362186213000, 8.149999994537637349, -23.30088464923126423 ) ) ;
#23023 = CARTESIAN_POINT ( 'NONE',  ( -19.06425588902558133, 61.26524333240935505, 19.11951029504797006 ) ) ;
#23024 = CYLINDRICAL_SURFACE ( 'NONE', #24185, 32.50000000000000000 ) ;
#23025 = CARTESIAN_POINT ( 'NONE',  ( -27.16883889988623935, 1.325000002731169246, 19.73931689729374739 ) ) ;
#23026 = DIRECTION ( 'NONE',  ( -0.000000000000000000, 1.000000000000000000, -0.000000000000000000 ) ) ;
#23027 = CARTESIAN_POINT ( 'NONE',  ( 10.37757302488624767, 37.97500000273119980, 31.93888565452638417 ) ) ;
#23028 = CARTESIAN_POINT ( 'NONE',  ( 23.41746824999999887, 9.124999997268817609, 0.000000000000000000 ) ) ;
#23029 = VERTEX_POINT ( 'NONE', #20572 ) ;
#23030 = CARTESIAN_POINT ( 'NONE',  ( 27.16883889988623935, 74.57500000273120122, -19.73931689729374384 ) ) ;
#23031 = CARTESIAN_POINT ( 'NONE',  ( -32.50000000000000000, 22.40000000546237402, -10.55989012756945478 ) ) ;
#23032 = CARTESIAN_POINT ( 'NONE',  ( 20.50609665441005092, 41.21875000000000000, 20.50609665440969209 ) ) ;
#23033 = CARTESIAN_POINT ( 'NONE',  ( 26.29305231718579350, 61.30000000546237260, 19.10302069950537529 ) ) ;
#23034 = ORIENTED_EDGE ( 'NONE', *, *, #16178, .F. ) ;
#23035 = CARTESIAN_POINT ( 'NONE',  ( -32.50000000000000000, 10.50000000546236123, 0.000000000000000000 ) ) ;
#23036 = CARTESIAN_POINT ( 'NONE',  ( 6.486482029760649416E-15, 39.62500000273117706, 35.31076352940723240 ) ) ;
#23037 = CARTESIAN_POINT ( 'NONE',  ( 0.000000000000000000, 80.00000000000001421, 0.000000000000000000 ) ) ;
#23038 = CARTESIAN_POINT ( 'NONE',  ( 20.08610463437158344, 5.200000005462368513, 27.64615127144129403 ) ) ;
#23039 = CARTESIAN_POINT ( 'NONE',  ( -1.778240108872766143E-15, 7.500000000000001776, -32.49999999999999289 ) ) ;
#23040 = CARTESIAN_POINT ( 'NONE',  ( -7.505752307972844761, 14.29166666666666430, 28.01184896238304134 ) ) ;
#23041 = CARTESIAN_POINT ( 'NONE',  ( 32.50000000000000000, 49.09999999999999432, -10.55989012756945833 ) ) ;
#23042 = LINE ( 'NONE', #22696, #13785 ) ;
#23043 = CARTESIAN_POINT ( 'NONE',  ( 33.58253175000000823, 18.27500000273118275, 10.91162601494192863 ) ) ;
#23044 = CARTESIAN_POINT ( 'NONE',  ( -24.50000000000000000, 7.000000000000006217, -3.000384657911015469E-15 ) ) ;
#23045 = CARTESIAN_POINT ( 'NONE',  ( -27.95245687107223986, 27.31993083240935505, 0.04044903255043252877 ) ) ;
#23046 = CARTESIAN_POINT ( 'NONE',  ( 4.300734207923757602, 78.77500000273118985, -13.23629886949340673 ) ) ;
#23047 = CARTESIAN_POINT ( 'NONE',  ( 0.000000000000000000, 80.00000000000001421, 0.000000000000000000 ) ) ;
#23048 = CARTESIAN_POINT ( 'NONE',  ( 33.58253175000000823, 76.27500000273118985, 10.91162601494192863 ) ) ;
#23049 = ORIENTED_EDGE ( 'NONE', *, *, #17973, .T. ) ;
#23050 = CARTESIAN_POINT ( 'NONE',  ( 23.41746825000000243, 13.22499999726881192, -7.608796670333727974 ) ) ;
#23051 = CARTESIAN_POINT ( 'NONE',  ( 18.94512977948575738, 6.424999997268809437, 13.76444248337723408 ) ) ;
#23052 = CARTESIAN_POINT ( 'NONE',  ( -26.07999730980477437, 52.67708333333333570, 6.988114217768305103 ) ) ;
#23053 = CARTESIAN_POINT ( 'NONE',  ( -33.58253175000000113, 61.12500000273117706, 0.000000000000000000 ) ) ;
#23054 = CARTESIAN_POINT ( 'NONE',  ( 27.16883889988623935, 26.57500000273120477, -19.73931689729374384 ) ) ;
#23055 = CARTESIAN_POINT ( 'NONE',  ( 10.37757302488624767, 9.975000002731201576, 31.93888565452638417 ) ) ;
#23056 = CARTESIAN_POINT ( 'NONE',  ( -19.09188309203694445, 32.62500000000000000, -19.09188309203661049 ) ) ;
#23057 = CARTESIAN_POINT ( 'NONE',  ( -15.04653450569291984, 19.31027750092397710, 25.98046417659859486 ) ) ;
#23058 = CARTESIAN_POINT ( 'NONE',  ( 20.50609665441005092, 65.28125000000000000, 20.50609665440969209 ) ) ;
#23059 = CARTESIAN_POINT ( 'NONE',  ( -33.58253175000000113, 3.125000002731193049, 0.000000000000000000 ) ) ;
#23060 = EDGE_CURVE ( 'NONE', #13703, #24826, #1707, .T. ) ;
#23061 = CARTESIAN_POINT ( 'NONE',  ( 4.300734207923761154, 73.97500000273119269, 13.23629886949340495 ) ) ;
#23062 = CARTESIAN_POINT ( 'NONE',  ( 32.50000000000000000, 39.10000000000002274, -10.55989012756945833 ) ) ;
#23063 = CARTESIAN_POINT ( 'NONE',  ( 33.58253175000000113, 48.12500000273117706, -4.112674001490185761E-15 ) ) ;
#23064 = CARTESIAN_POINT ( 'NONE',  ( 23.41746825000000243, 6.524999997268818852, 7.608796670333735079 ) ) ;
#23065 = CARTESIAN_POINT ( 'NONE',  ( -27.95245687107223276, 66.57031250000000000, 2.498001805406602216E-13 ) ) ;
#23066 = VERTEX_POINT ( 'NONE', #26554 ) ;
#23067 = CARTESIAN_POINT ( 'NONE',  ( 27.16883889988624290, 56.17500000273119554, 19.73931689729373673 ) ) ;
#23068 = CARTESIAN_POINT ( 'NONE',  ( -32.50000000000000000, 4.600000005462387520, 10.55989012756946366 ) ) ;
#23069 = CARTESIAN_POINT ( 'NONE',  ( 19.11951029504763611, 45.23475666759063785, -19.06425588902591173 ) ) ;
#23070 = CARTESIAN_POINT ( 'NONE',  ( 20.75514604977249178, 78.07500000273117280, 28.56700777964553950 ) ) ;
#23071 = EDGE_LOOP ( 'NONE', ( #18528, #18571, #18102, #13116 ) ) ;
#23072 = CARTESIAN_POINT ( 'NONE',  ( 33.58253175000000823, 26.02500000273120406, 10.91162601494192863 ) ) ;
#23073 = CARTESIAN_POINT ( 'NONE',  ( 2.740863092043355209E-13, 14.14843749999999289, 30.02300923189239512 ) ) ;
#23074 = EDGE_LOOP ( 'NONE', ( #31544, #15335, #23845, #7964, #20097, #23108, #20513, #15396, #12212, #5708, #10331, #11492, #20466, #23543, #18695, #20551, #16080, #23960 ) ) ;
#23075 = CARTESIAN_POINT ( 'NONE',  ( 20.08610463437158344, 29.20000000546237118, 27.64615127144129403 ) ) ;
#23076 = CARTESIAN_POINT ( 'NONE',  ( 10.37757302488624056, 68.52500000273120406, -31.93888565452638417 ) ) ;
#23077 = CARTESIAN_POINT ( 'NONE',  ( -20.50609665440969209, 42.07812499999999289, 20.50609665441005092 ) ) ;
#23078 = CARTESIAN_POINT ( 'NONE',  ( 1.577395562988744260E-15, 14.50000000000000888, -25.76082449383753925 ) ) ;
#23079 = CARTESIAN_POINT ( 'NONE',  ( 23.09401076758502569, 96.00000000000002842, -6.857326241137392698E-15 ) ) ;
#23080 = CARTESIAN_POINT ( 'NONE',  ( -27.16883889988623935, 11.32500000273117813, 19.73931689729374739 ) ) ;
#23081 = FILL_AREA_STYLE ('',( #19495 ) ) ;
#23082 = CARTESIAN_POINT ( 'NONE',  ( -20.47846945139866648, 54.39024333240934794, 20.53372385742108008 ) ) ;
#23083 = CARTESIAN_POINT ( 'NONE',  ( -9.270509831248421762, 74.30000000000001137, 12.75976212528060039 ) ) ;
#23084 = CARTESIAN_POINT ( 'NONE',  ( -4.000000000000003553, 3.673940397442059967E-15, -30.00000000000000000 ) ) ;
#23085 = CARTESIAN_POINT ( 'NONE',  ( 24.50000000000000000, 15.74999999453763344, 0.000000000000000000 ) ) ;
#23086 = CARTESIAN_POINT ( 'NONE',  ( -9.657523855033125146E-16, 71.75000000546239676, -15.77193336357400710 ) ) ;
#23087 = CARTESIAN_POINT ( 'NONE',  ( 26.07999730980477437, 23.45833333333333215, -6.988114217768290004 ) ) ;
#23088 = CARTESIAN_POINT ( 'NONE',  ( 33.58253175000000113, 28.12500000273118772, -4.112674001490185761E-15 ) ) ;
#23089 = CARTESIAN_POINT ( 'NONE',  ( 6.486482029760649416E-15, 77.62500000273121259, 35.31076352940723240 ) ) ;
#23090 = AXIS2_PLACEMENT_3D ( 'NONE', #9764, #7187, #2041 ) ;
#23091 = CARTESIAN_POINT ( 'NONE',  ( 27.16883889988624290, 42.17500000273118133, 19.73931689729373673 ) ) ;
#23092 = CARTESIAN_POINT ( 'NONE',  ( -27.16883889988623935, 19.57500000273118701, 19.73931689729374739 ) ) ;
#23093 = CARTESIAN_POINT ( 'NONE',  ( -24.50000000000000000, 16.74999999453763522, -3.000384657911015469E-15 ) ) ;
#23094 = CARTESIAN_POINT ( 'NONE',  ( 33.58253175000000823, 78.02500000273118985, 10.91162601494192685 ) ) ;
#23095 = EDGE_CURVE ( 'NONE', #33570, #26901, #18908, .T. ) ;
#23096 = CARTESIAN_POINT ( 'NONE',  ( 4.023268246324634798E-14, 8.499999999999992895, -24.50000000000000355 ) ) ;
#23097 = CARTESIAN_POINT ( 'NONE',  ( -26.29305231718578995, 62.20000000000001705, 19.10302069950538595 ) ) ;
#23098 = CARTESIAN_POINT ( 'NONE',  ( -1.778240108872766143E-15, 52.00000000546237544, -32.49999999999999289 ) ) ;
#23099 = CARTESIAN_POINT ( 'NONE',  ( -2.162160676586882350E-15, 64.62500000273121259, -35.31076352940722529 ) ) ;
#23100 = EDGE_CURVE ( 'NONE', #3977, #6976, #24199, .T. ) ;
#23101 = CARTESIAN_POINT ( 'NONE',  ( 23.41746824999999887, 11.12499999726881938, 0.000000000000000000 ) ) ;
#23102 = CARTESIAN_POINT ( 'NONE',  ( 33.58253175000000113, 70.47500000273117848, -10.91162601494193751 ) ) ;
#23103 = CARTESIAN_POINT ( 'NONE',  ( -33.58253175000000113, 9.225000002731178483, 10.91162601494193929 ) ) ;
#23104 = CARTESIAN_POINT ( 'NONE',  ( 18.94512977948575738, 12.92499999726881654, 13.76444248337723408 ) ) ;
#23105 = CARTESIAN_POINT ( 'NONE',  ( 6.950374756619721595, 12.00559000092397532, 26.09010956794232428 ) ) ;
#23106 = VERTEX_POINT ( 'NONE', #23478 ) ;
#23107 = CARTESIAN_POINT ( 'NONE',  ( -33.58253175000000113, 47.22500000273117138, 10.91162601494193929 ) ) ;
#23108 = ORIENTED_EDGE ( 'NONE', *, *, #13369, .T. ) ;
#23109 = CARTESIAN_POINT ( 'NONE',  ( -7.505752307972844761, 31.47916666666666075, 28.01184896238304134 ) ) ;
#23110 = CARTESIAN_POINT ( 'NONE',  ( 5.814984965855610735E-15, -70.48295565631028126, 0.000000000000000000 ) ) ;
#23111 = CARTESIAN_POINT ( 'NONE',  ( -20.08610463437156923, 2.800000005462385477, 27.64615127144130113 ) ) ;
#23112 = AXIS2_PLACEMENT_3D ( 'NONE', #12612, #33369, #9865 ) ;
#23113 = CARTESIAN_POINT ( 'NONE',  ( -4.223320258572819786E-15, 11.24999999453762456, 24.50000000000000000 ) ) ;
#23114 = CARTESIAN_POINT ( 'NONE',  ( 24.50000000000000355, 19.64999999453763024, 7.960532557706212486 ) ) ;
#23115 = CARTESIAN_POINT ( 'NONE',  ( -18.94512977948575738, 13.42499999726881654, -13.76444248337723231 ) ) ;
#23116 = CARTESIAN_POINT ( 'NONE',  ( -2.162160676586881955E-15, 14.87500000273120193, -35.31076352940723240 ) ) ;
#23117 = CARTESIAN_POINT ( 'NONE',  ( -26.29305231718579350, 20.30000000546239391, -19.10302069950537884 ) ) ;
#23118 = CARTESIAN_POINT ( 'NONE',  ( -2.092463501923844636E-15, 65.49999999999998579, -34.17252228774368916 ) ) ;
#23119 = CARTESIAN_POINT ( 'NONE',  ( 5.779280353836490358E-15, 24.50000000000000711, 32.49999999999999289 ) ) ;
#23120 = CARTESIAN_POINT ( 'NONE',  ( -20.50609665441004736, 15.43749999999999645, -20.50609665440969565 ) ) ;
#23121 = CARTESIAN_POINT ( 'NONE',  ( 27.16883889988624290, 30.17500000273118488, 19.73931689729373673 ) ) ;
#23122 = CARTESIAN_POINT ( 'NONE',  ( -13.91746824999999532, 79.47500000273117848, 4.522059556121122093 ) ) ;
#23123 = CARTESIAN_POINT ( 'NONE',  ( -2.584737979205442066E-13, 39.92968750000000000, -30.02300923189239867 ) ) ;
#23124 = CARTESIAN_POINT ( 'NONE',  ( 0.000000000000000000, -20.00000000000000000, 0.000000000000000000 ) ) ;
#23125 = CARTESIAN_POINT ( 'NONE',  ( -23.41746824999999887, 16.12499999726882294, -2.867812753649727150E-15 ) ) ;
#23126 = CARTESIAN_POINT ( 'NONE',  ( 32.50000000000000000, 11.09999999999999964, -10.55989012756945833 ) ) ;
#23127 = CARTESIAN_POINT ( 'NONE',  ( -20.08610463437156923, 52.30000000000000426, 27.64615127144130113 ) ) ;
#23128 = CARTESIAN_POINT ( 'NONE',  ( -14.01125832528328985, 51.95534749907602645, -24.18731323226223040 ) ) ;
#23129 = CARTESIAN_POINT ( 'NONE',  ( -33.58253175000000113, 53.02500000273118985, -10.91162601494193218 ) ) ;
#23130 = CARTESIAN_POINT ( 'NONE',  ( -33.58253175000000113, 61.27500000273118985, -10.91162601494193218 ) ) ;
#23131 = CARTESIAN_POINT ( 'NONE',  ( -27.16883889988623935, 41.57500000273117990, 19.73931689729374739 ) ) ;
#23132 = CARTESIAN_POINT ( 'NONE',  ( -23.41746824999999887, 15.52499999726882507, -7.608796670333730638 ) ) ;
#23133 = CARTESIAN_POINT ( 'NONE',  ( 19.09188309203694800, 13.71874999999999467, 19.09188309203660694 ) ) ;
#23134 = CARTESIAN_POINT ( 'NONE',  ( 5.147494310547426899, 15.94874572391552903, -32.50000000000000000 ) ) ;
#23135 = CARTESIAN_POINT ( 'NONE',  ( 32.50000000000000000, 51.50000000546239676, -3.980102097228898626E-15 ) ) ;
#23136 = CARTESIAN_POINT ( 'NONE',  ( 20.08610463437158344, 78.70000000000000284, 27.64615127144129403 ) ) ;
#23137 = CARTESIAN_POINT ( 'NONE',  ( 33.58253175000000113, 18.22500000273118559, -10.91162601494193751 ) ) ;
#23138 = CARTESIAN_POINT ( 'NONE',  ( 3.306546357697853733E-15, -12.99999999999999822, -27.00000000000000000 ) ) ;
#23139 = CARTESIAN_POINT ( 'NONE',  ( 3.000384657911015469E-15, 16.99999999999998579, 24.50000000000000000 ) ) ;
#23140 = CYLINDRICAL_SURFACE ( 'NONE', #12666, 32.50000000000000000 ) ;
#23141 = CARTESIAN_POINT ( 'NONE',  ( -6.950374756619247307, 19.72878499907601935, 26.09010956794245217 ) ) ;
#23142 = EDGE_CURVE ( 'NONE', #1179, #17842, #26115, .T. ) ;
#23143 = CARTESIAN_POINT ( 'NONE',  ( -10.04305231718579172, 40.10000000546236265, -30.90933677959248982 ) ) ;
#23144 = CARTESIAN_POINT ( 'NONE',  ( 5.779280353836490358E-15, 66.49999999999998579, 32.49999999999999289 ) ) ;
#23145 = CARTESIAN_POINT ( 'NONE',  ( 33.58253175000000113, 28.12500000273118772, -4.112674001490185761E-15 ) ) ;
#23146 = CARTESIAN_POINT ( 'NONE',  ( 27.16883889988624290, 66.17500000273118133, 19.73931689729373673 ) ) ;
#23147 = CARTESIAN_POINT ( 'NONE',  ( 6.988114217768294445, 34.63020833333332860, 26.07999730980477437 ) ) ;
#23148 = VERTEX_POINT ( 'NONE', #23648 ) ;
#23149 = CARTESIAN_POINT ( 'NONE',  ( -33.58253175000000113, 67.02500000273117564, -10.91162601494193218 ) ) ;
#23150 = CARTESIAN_POINT ( 'NONE',  ( 2.740863092043355209E-13, 48.52343750000000000, 30.02300923189239512 ) ) ;
#23151 = CARTESIAN_POINT ( 'NONE',  ( 0.000000000000000000, -10.99999999999999645, -33.00000000000000000 ) ) ;
#23152 = VERTEX_POINT ( 'NONE', #15592 ) ;
#23153 = CARTESIAN_POINT ( 'NONE',  ( -28.02196122052045268, 60.98996500092398065, 7.468012846824790607 ) ) ;
#23154 = CARTESIAN_POINT ( 'NONE',  ( 26.09010956794232428, 59.27121500092397355, -6.950374756619718042 ) ) ;
#23155 = AXIS2_PLACEMENT_3D ( 'NONE', #22802, #22973, #12153 ) ;
#23156 = ORIENTED_EDGE ( 'NONE', *, *, #27079, .T. ) ;
#23157 = CARTESIAN_POINT ( 'NONE',  ( -33.58253175000000113, 9.125000002731184168, 0.000000000000000000 ) ) ;
#23158 = AXIS2_PLACEMENT_3D ( 'NONE', #27159, #24584, #1914 ) ;
#23159 = CARTESIAN_POINT ( 'NONE',  ( -7.543491769121917656, 14.28607666574268720, -28.00173670424536354 ) ) ;
#23160 = CARTESIAN_POINT ( 'NONE',  ( 12.13525491562420910, 79.45000000546237118, -8.816778784387098611 ) ) ;
#23161 = CARTESIAN_POINT ( 'NONE',  ( -2.162160676586881955E-15, 36.87500000273116996, -35.31076352940723240 ) ) ;
#23162 = CARTESIAN_POINT ( 'NONE',  ( -10.04305231718578462, 42.90000000546237402, 30.90933677959249337 ) ) ;
#23163 = ADVANCED_FACE ( 'NONE', ( #12834 ), #10265, .T. ) ;
#23164 = CARTESIAN_POINT ( 'NONE',  ( 15.00000000000000000, 79.00000000000001421, -1.836970198721029589E-15 ) ) ;
#23165 = CARTESIAN_POINT ( 'NONE',  ( -15.01150461594642138, 63.70572916666667140, -26.00068869287340334 ) ) ;
#23166 = CARTESIAN_POINT ( 'NONE',  ( 27.16883889988623935, 24.32500000273119056, -19.73931689729374384 ) ) ;
#23167 = CARTESIAN_POINT ( 'NONE',  ( -32.50000000000000000, 52.60000000546235555, 10.55989012756946366 ) ) ;
#23168 = CARTESIAN_POINT ( 'NONE',  ( -33.58253175000000113, 49.37500000273120548, 0.000000000000000000 ) ) ;
#23169 =( NAMED_UNIT ( * ) SI_UNIT ( $, .STERADIAN. ) SOLID_ANGLE_UNIT ( ) );
#23170 = CARTESIAN_POINT ( 'NONE',  ( -26.29305231718579350, 31.80000000000000782, -19.10302069950537884 ) ) ;
#23171 = CARTESIAN_POINT ( 'NONE',  ( 10.04305231718578817, 25.40000000000000568, -30.90933677959249337 ) ) ;
#23172 = CARTESIAN_POINT ( 'NONE',  ( -15.14183272437242600, 1.299999999999988054, 20.84094480462497856 ) ) ;
#23173 = CARTESIAN_POINT ( 'NONE',  ( 6.486482029760649416E-15, 71.62500000273119838, 35.31076352940723240 ) ) ;
#23174 = CARTESIAN_POINT ( 'NONE',  ( 5.147494310547426899, 63.44874571845314648, -32.50000000000000000 ) ) ;
#23175 = CARTESIAN_POINT ( 'NONE',  ( -5.147494310547423346, 20.94874572391552547, 32.50000000000000000 ) ) ;
#23176 = CARTESIAN_POINT ( 'NONE',  ( 27.16883889988624290, 60.17500000273118133, 19.73931689729373673 ) ) ;
#23177 = CARTESIAN_POINT ( 'NONE',  ( -11.25946833292375793, 79.07500000273121543, 8.180482586598737171 ) ) ;
#23178 = CARTESIAN_POINT ( 'NONE',  ( 26.29305231718578995, 7.700000005462392494, -19.10302069950538240 ) ) ;
#23179 = CARTESIAN_POINT ( 'NONE',  ( -33.58253175000000113, 9.025000002731184523, -10.91162601494193218 ) ) ;
#23180 = CARTESIAN_POINT ( 'NONE',  ( 15.14183272437242245, 12.04999999453764126, -20.84094480462497856 ) ) ;
#23181 = CARTESIAN_POINT ( 'NONE',  ( 19.06425588902592239, 25.46913166759064140, 19.11951029504763611 ) ) ;
#23182 = CARTESIAN_POINT ( 'NONE',  ( 4.374313548017275011, 67.00000000000000000, -33.03144926559789241 ) ) ;
#23183 = VECTOR ( 'NONE', #29657, 1000.000000000000000 ) ;
#23184 = CARTESIAN_POINT ( 'NONE',  ( 6.486482029760649416E-15, 43.62500000273116285, 35.31076352940723240 ) ) ;
#23185 = FACE_OUTER_BOUND ( 'NONE', #9044, .T. ) ;
#23186 = CARTESIAN_POINT ( 'NONE',  ( 32.50000000000000000, 19.10000000000000497, -10.55989012756945833 ) ) ;
#23187 = CARTESIAN_POINT ( 'NONE',  ( -12.13525491562421088, 81.79999999999998295, -8.816778784387096835 ) ) ;
#23188 = CARTESIAN_POINT ( 'NONE',  ( -0.04044903255044120238, 41.92930583240936215, -30.02300923189239867 ) ) ;
#23189 = CARTESIAN_POINT ( 'NONE',  ( -32.50000000000000000, 62.40000000546235981, -10.55989012756945478 ) ) ;
#23190 = CARTESIAN_POINT ( 'NONE',  ( 13.91746825000000065, 74.27500000273120406, 4.522059556121114987 ) ) ;
#23191 = CARTESIAN_POINT ( 'NONE',  ( -24.50000000000000711, 2.849999994537638859, 7.960532557706201828 ) ) ;
#23192 = CARTESIAN_POINT ( 'NONE',  ( -26.06988505166722803, 68.42670166574269786, 7.025853678916877953 ) ) ;
#23193 = CARTESIAN_POINT ( 'NONE',  ( 5.779280353836490358E-15, 54.49999999999999289, 32.49999999999999289 ) ) ;
#23194 = CARTESIAN_POINT ( 'NONE',  ( -26.29305231718578995, 74.70000000546239960, 19.10302069950538595 ) ) ;
#23195 = CARTESIAN_POINT ( 'NONE',  ( -26.00068869287340334, 14.72135416666666607, 15.01150461594643382 ) ) ;
#23196 = CARTESIAN_POINT ( 'NONE',  ( 33.58253175000000113, 34.47500000273119980, -10.91162601494193751 ) ) ;
#23197 = CARTESIAN_POINT ( 'NONE',  ( 14.47279130897151944, 9.424999997268814766, -19.92008829642072598 ) ) ;
#23198 = EDGE_LOOP ( 'NONE', ( #15436, #23587 ) ) ;
#23199 = CARTESIAN_POINT ( 'NONE',  ( 27.16883889988624290, 76.17500000273119554, 19.73931689729373673 ) ) ;
#23200 = CARTESIAN_POINT ( 'NONE',  ( -26.29305231718578995, 22.70000000546239249, 19.10302069950538595 ) ) ;
#23201 = EDGE_CURVE ( 'NONE', #15184, #31380, #9372, .T. ) ;
#23202 = CARTESIAN_POINT ( 'NONE',  ( -26.00068869287368756, 39.35677083333331439, -15.01150461594595775 ) ) ;
#23203 = CARTESIAN_POINT ( 'NONE',  ( 7.505752307972854531, 60.69791666666667140, -28.01184896238303423 ) ) ;
#23204 = CARTESIAN_POINT ( 'NONE',  ( -10.37757302488624411, 56.97500000273119980, -31.93888565452638417 ) ) ;
#23205 = CARTESIAN_POINT ( 'NONE',  ( 32.50000000000000000, 61.60000000546236976, -10.55989012756945833 ) ) ;
#23206 = EDGE_LOOP ( 'NONE', ( #29347, #12944, #1957, #10035 ) ) ;
#23207 = CARTESIAN_POINT ( 'NONE',  ( -3.880418787951104953, 13.19874571299077459, 24.50000000000000711 ) ) ;
#23208 = CARTESIAN_POINT ( 'NONE',  ( 6.486482029760649416E-15, 43.62500000273116285, 35.31076352940723240 ) ) ;
#23209 = CARTESIAN_POINT ( 'NONE',  ( -4.523095164977116484E-15, 18.12499999726880517, 24.62258325217400312 ) ) ;
#23210 = CARTESIAN_POINT ( 'NONE',  ( 6.486482029760649416E-15, 65.87500000273119838, 35.31076352940723240 ) ) ;
#23211 = CARTESIAN_POINT ( 'NONE',  ( -2.092463501923844636E-15, 8.000000005462366559, -34.17252228774368916 ) ) ;
#23212 = VECTOR ( 'NONE', #29748, 1000.000000000000227 ) ;
#23213 = EDGE_CURVE ( 'NONE', #30412, #19806, #14880, .T. ) ;
#23214 = CARTESIAN_POINT ( 'NONE',  ( 27.16883889988623935, 58.32500000273120833, -19.73931689729374384 ) ) ;
#23215 = CARTESIAN_POINT ( 'NONE',  ( 15.01150461594596486, 12.71614583333333037, -26.00068869287367690 ) ) ;
#23216 = CARTESIAN_POINT ( 'NONE',  ( -26.29305231718578995, 48.19999999999999574, 19.10302069950538595 ) ) ;
#23217 = CYLINDRICAL_SURFACE ( 'NONE', #75, 15.00000000000000000 ) ;
#23218 =( BOUNDED_CURVE ( )  B_SPLINE_CURVE ( 2, ( #19884, #9752, #1852, #25199, #1338, #12152, #1509, #4095, #20238, #11984, #22296, #32741, #22453 ),
 .UNSPECIFIED., .F., .T. ) 
 B_SPLINE_CURVE_WITH_KNOTS ( ( 3, 2, 2, 2, 2, 2, 3 ),
 ( 0.1500000000000000222, 0.1600000000000000033, 0.1799999999999999933, 0.2000000000000000111, 0.2200000000000000011, 0.2399999999999999911, 0.2500000000000000000 ),
 .UNSPECIFIED. ) 
 CURVE ( )  GEOMETRIC_REPRESENTATION_ITEM ( )  RATIONAL_B_SPLINE_CURVE ( ( 0.9755282581475768211, 0.9755282581475768211, 1.000000000000000000, 0.9510565162951535312, 1.000000000000000000, 0.9510565162951535312, 1.000000000000000000, 0.9510565162951535312, 1.000000000000000000, 0.9510565162951535312, 1.000000000000000000, 0.9755282581475768211, 0.9755282581475768211 ) ) 
 REPRESENTATION_ITEM ( '' )  );
#23219 = CARTESIAN_POINT ( 'NONE',  ( -10.37757302488623701, 11.77500000273118452, 31.93888565452638417 ) ) ;
#23220 = CARTESIAN_POINT ( 'NONE',  ( -10.04305231718579172, 73.59999999999999432, -30.90933677959248982 ) ) ;
#23221 = CARTESIAN_POINT ( 'NONE',  ( -19.11951029504797006, 31.18711833240935150, -19.06425588902558133 ) ) ;
#23222 = CARTESIAN_POINT ( 'NONE',  ( -13.91746824999999532, 70.97500000273116427, 4.522059556121122093 ) ) ;
#23223 = CARTESIAN_POINT ( 'NONE',  ( -10.37757302488624411, 76.97500000273119269, -31.93888565452638417 ) ) ;
#23224 = DIRECTION ( 'NONE',  ( 0.000000000000000000, 0.000000000000000000, 1.000000000000000000 ) ) ;
#23225 = CARTESIAN_POINT ( 'NONE',  ( 10.37757302488624767, 71.97500000273120691, 31.93888565452638417 ) ) ;
#23226 = VERTEX_POINT ( 'NONE', #10601 ) ;
#23227 = CARTESIAN_POINT ( 'NONE',  ( 23.41746825000000243, 13.02499999726881619, 7.608796670333735079 ) ) ;
#23228 = CARTESIAN_POINT ( 'NONE',  ( 18.94512977948575738, 2.424999997268806329, 13.76444248337723408 ) ) ;
#23229 = CARTESIAN_POINT ( 'NONE',  ( 26.07999730980490227, 54.68229166666665719, 6.988114217767821046 ) ) ;
#23230 = CARTESIAN_POINT ( 'NONE',  ( -20.75514604977248112, 57.42500000273118843, 28.56700777964554661 ) ) ;
#23231 = CARTESIAN_POINT ( 'NONE',  ( -27.16883889988624290, 17.17500000273118488, -19.73931689729374028 ) ) ;
#23232 = CARTESIAN_POINT ( 'NONE',  ( -20.75514604977248823, 9.075000002731183457, -28.56700777964554305 ) ) ;
#23233 = CARTESIAN_POINT ( 'NONE',  ( -24.20753774853756823, 32.48177083333332860, -13.97622843553588723 ) ) ;
#23234 = UNCERTAINTY_MEASURE_WITH_UNIT (LENGTH_MEASURE( 1.000000000000000082E-05 ), #9258, 'distance_accuracy_value', 'NONE');
#23235 = CARTESIAN_POINT ( 'NONE',  ( 28.00173670424549499, 18.30767333425730214, 7.543491769121417612 ) ) ;
#23236 = CARTESIAN_POINT ( 'NONE',  ( -26.00068869287368756, 66.85677083333334281, -15.01150461594595775 ) ) ;
#23237 = CARTESIAN_POINT ( 'NONE',  ( 33.58253175000000113, 2.125000002731192161, -4.112674001490185761E-15 ) ) ;
#23238 = CARTESIAN_POINT ( 'NONE',  ( -10.04305231718579172, 56.10000000546239107, -30.90933677959248982 ) ) ;
#23239 = CARTESIAN_POINT ( 'NONE',  ( 32.50000000000000000, 40.99999999999999289, -3.980102097228898626E-15 ) ) ;
#23240 = CARTESIAN_POINT ( 'NONE',  ( -10.37757302488623701, 47.52500000273118985, 31.93888565452638417 ) ) ;
#23241 = CIRCLE ( 'NONE', #15025, 33.00000000000000000 ) ;
#23242 = CARTESIAN_POINT ( 'NONE',  ( -7.236395654485763274, 12.02499999726880375, 22.27133577429736633 ) ) ;
#23243 = CARTESIAN_POINT ( 'NONE',  ( 4.635254915624209993, 79.39999999999999147, -14.26584774442730463 ) ) ;
#23244 = ORIENTED_EDGE ( 'NONE', *, *, #23644, .T. ) ;
#23245 = CARTESIAN_POINT ( 'NONE',  ( -27.16883889988623935, 51.57500000273117280, 19.73931689729374739 ) ) ;
#23246 = CARTESIAN_POINT ( 'NONE',  ( 3.000384657911015469E-15, 0.000000000000000000, -24.50000000000000000 ) ) ;
#23247 = CARTESIAN_POINT ( 'NONE',  ( 24.18731323226247554, 42.51340250092398065, 14.01125832528285997 ) ) ;
#23248 = CARTESIAN_POINT ( 'NONE',  ( -20.75514604977248823, 73.07500000273115859, -28.56700777964554305 ) ) ;
#23249 = ORIENTED_EDGE ( 'NONE', *, *, #28032, .T. ) ;
#23250 = CARTESIAN_POINT ( 'NONE',  ( 20.75514604977249178, 25.82500000273117280, 28.56700777964553950 ) ) ;
#23251 = CARTESIAN_POINT ( 'NONE',  ( -26.00068869287340334, 14.72135416666666607, 15.01150461594643382 ) ) ;
#23252 = VERTEX_POINT ( 'NONE', #21079 ) ;
#23253 = CARTESIAN_POINT ( 'NONE',  ( 4.041334437186266200E-15, -10.99999999999999645, 33.00000000000000000 ) ) ;
#23254 = CARTESIAN_POINT ( 'NONE',  ( -27.16883889988623935, 63.32500000273119412, 19.73931689729374739 ) ) ;
#23255 = CARTESIAN_POINT ( 'NONE',  ( -30.02300923189239512, 39.07031249999997868, 2.654126918244515359E-13 ) ) ;
#23256 = FACE_OUTER_BOUND ( 'NONE', #12248, .T. ) ;
#23257 = CARTESIAN_POINT ( 'NONE',  ( -4.523095164977117273E-15, 4.624999997268820273, 24.62258325217400312 ) ) ;
#23258 = CARTESIAN_POINT ( 'NONE',  ( 33.58253175000000113, 6.225000002731185589, -10.91162601494193751 ) ) ;
#23259 =( NAMED_UNIT ( * ) PLANE_ANGLE_UNIT ( ) SI_UNIT ( $, .RADIAN. ) );
#23260 = CARTESIAN_POINT ( 'NONE',  ( 7.543491769121922985, 50.37982666574269075, 28.00173670424535644 ) ) ;
#23261 = CARTESIAN_POINT ( 'NONE',  ( 15.00000000000000000, 75.00000000000001421, -1.836970198721029589E-15 ) ) ;
#23262 = CIRCLE ( 'NONE', #23805, 32.63512777199724724 ) ;
#23263 = CARTESIAN_POINT ( 'NONE',  ( -1.089172066684569321E-14, 78.49999999999998579, 15.00000000000000000 ) ) ;
#23264 = CYLINDRICAL_SURFACE ( 'NONE', #16668, 32.50000000000000000 ) ;
#23265 = CARTESIAN_POINT ( 'NONE',  ( -2.092463501923844636E-15, 15.50000000000000533, -34.17252228774368916 ) ) ;
#23266 = CARTESIAN_POINT ( 'NONE',  ( -24.50000000000000355, 10.64999999453762491, -7.960532557706207157 ) ) ;
#23267 = CARTESIAN_POINT ( 'NONE',  ( 4.635254915624209993, 71.65000000546240244, -14.26584774442730463 ) ) ;
#23268 = CARTESIAN_POINT ( 'NONE',  ( 27.95245687107222921, 20.16406249999999645, -2.463307335887066074E-13 ) ) ;
#23269 = CARTESIAN_POINT ( 'NONE',  ( -33.58253175000000113, 29.12500000273118772, 0.000000000000000000 ) ) ;
#23270 = CARTESIAN_POINT ( 'NONE',  ( 9.270509831248425314, 74.69999999999996021, 12.75976212528059683 ) ) ;
#23271 = CARTESIAN_POINT ( 'NONE',  ( 33.58253175000000823, 34.27500000273116854, 10.91162601494192863 ) ) ;
#23272 = CARTESIAN_POINT ( 'NONE',  ( -33.58253175000000113, 19.37500000273118062, 0.000000000000000000 ) ) ;
#23273 = CARTESIAN_POINT ( 'NONE',  ( -19.82091636218621034, 6.800000000000000711, -14.40073868116559552 ) ) ;
#23274 = CARTESIAN_POINT ( 'NONE',  ( 20.75514604977248467, 78.42500000273115290, -28.56700777964554305 ) ) ;
#23275 = DIRECTION ( 'NONE',  ( 0.000000000000000000, 0.000000000000000000, -1.000000000000000000 ) ) ;
#23276 = CARTESIAN_POINT ( 'NONE',  ( 26.29305231718578995, 61.20000000000001705, -19.10302069950538240 ) ) ;
#23277 = CARTESIAN_POINT ( 'NONE',  ( 31.38736896855614944, -89.55944200217849982, 0.000000000000000000 ) ) ;
#23278 = CARTESIAN_POINT ( 'NONE',  ( 33.58253175000000823, 66.02500000273118985, 10.91162601494192685 ) ) ;
#23279 = CARTESIAN_POINT ( 'NONE',  ( -23.41746824999999887, 6.124999997268814944, -2.867812753649727150E-15 ) ) ;
#23280 = CARTESIAN_POINT ( 'NONE',  ( -33.58253175000000113, 71.27500000273118985, -10.91162601494193218 ) ) ;
#23281 = CARTESIAN_POINT ( 'NONE',  ( -33.58253175000000113, 7.025000002731188964, -10.91162601494193041 ) ) ;
#23282 = CARTESIAN_POINT ( 'NONE',  ( -14.47279130897151589, 17.82499999726881157, -19.92008829642072598 ) ) ;
#23283 = CARTESIAN_POINT ( 'NONE',  ( -6.950374756619716266, 10.28684000092397532, -26.09010956794232428 ) ) ;
#23284 = VERTEX_POINT ( 'NONE', #15930 ) ;
#23285 = CARTESIAN_POINT ( 'NONE',  ( -20.75514604977248112, 41.42500000273118133, 28.56700777964554661 ) ) ;
#23286 = ORIENTED_EDGE ( 'NONE', *, *, #5341, .T. ) ;
#23287 = ORIENTED_EDGE ( 'NONE', *, *, #23296, .T. ) ;
#23288 = CARTESIAN_POINT ( 'NONE',  ( -30.02300923189239512, 39.07031249999997868, 2.654126918244515359E-13 ) ) ;
#23289 = CARTESIAN_POINT ( 'NONE',  ( 19.82091636218621034, 9.800000000000002487, 14.40073868116559730 ) ) ;
#23290 = CARTESIAN_POINT ( 'NONE',  ( -32.50000000000000000, 2.600000005462363095, 10.55989012756946366 ) ) ;
#23291 = CARTESIAN_POINT ( 'NONE',  ( -2.162160676586881955E-15, 78.62500000273115575, -35.31076352940723240 ) ) ;
#23292 = CARTESIAN_POINT ( 'NONE',  ( -7.236395654485763274, 2.524999997268823293, 22.27133577429736633 ) ) ;
#23293 = CARTESIAN_POINT ( 'NONE',  ( 18.94512977948575738, 14.42499999726881654, 13.76444248337723408 ) ) ;
#23294 = CARTESIAN_POINT ( 'NONE',  ( -10.37757302488624411, 14.97500000273119269, -31.93888565452638417 ) ) ;
#23295 = CARTESIAN_POINT ( 'NONE',  ( -32.50000000000000000, 18.40000000546238823, -10.55989012756945478 ) ) ;
#23296 = EDGE_CURVE ( 'NONE', #6976, #3977, #8845, .T. ) ;
#23297 = CARTESIAN_POINT ( 'NONE',  ( -20.08610463437156923, 68.30000000000001137, 27.64615127144130113 ) ) ;
#23298 = CARTESIAN_POINT ( 'NONE',  ( 19.82091636218621389, 11.94999999453763628, -14.40073868116559197 ) ) ;
#23299 = DIRECTION ( 'NONE',  ( -0.8660254037844402619, -0.4999999999999970579, 0.000000000000000000 ) ) ;
#23300 = CARTESIAN_POINT ( 'NONE',  ( -7.505752307973343918, 12.28645833333333037, -28.01184896238290989 ) ) ;
#23301 = CARTESIAN_POINT ( 'NONE',  ( -5.147494310547430452, 32.05125428700920764, -32.49999999999999289 ) ) ;
#23302 = CARTESIAN_POINT ( 'NONE',  ( 7.505752307973351023, 41.50520833333333570, 28.01184896238290278 ) ) ;
#23303 = SHAPE_DEFINITION_REPRESENTATION ( #3342, #33740 ) ;
#23304 = ADVANCED_FACE ( 'NONE', ( #31692 ), #18676, .F. ) ;
#23305 = PLANE ( 'NONE',  #17720 ) ;
#23306 = CARTESIAN_POINT ( 'NONE',  ( 14.47279130897151589, 14.82499999726881690, 19.92008829642072953 ) ) ;
#23307 = CARTESIAN_POINT ( 'NONE',  ( 10.04305231718579705, 8.599999999999996092, 30.90933677959248982 ) ) ;
#23308 = AXIS2_PLACEMENT_3D ( 'NONE', #13537, #24000, #18853 ) ;
#23309 = DIRECTION ( 'NONE',  ( 0.000000000000000000, 0.000000000000000000, -1.000000000000000000 ) ) ;
#23310 = CARTESIAN_POINT ( 'NONE',  ( -27.95245687107223986, 51.38243083240936215, 0.04044903255043252877 ) ) ;
#23311 = CARTESIAN_POINT ( 'NONE',  ( -2.162160676586881955E-15, 52.62500000273117706, -35.31076352940723240 ) ) ;
#23312 = CARTESIAN_POINT ( 'NONE',  ( 27.16883889988623935, 64.57500000273118701, -19.73931689729374384 ) ) ;
#23313 = CARTESIAN_POINT ( 'NONE',  ( -33.58253175000000113, 43.47500000273117138, 10.91162601494193929 ) ) ;
#23314 = FACE_OUTER_BOUND ( 'NONE', #32501, .T. ) ;
#23315 = CARTESIAN_POINT ( 'NONE',  ( 0.000000000000000000, -12.99999999999999822, 0.000000000000000000 ) ) ;
#23316 = CARTESIAN_POINT ( 'NONE',  ( -7.570916362186215665, 9.399999999999991473, 23.30088464923126423 ) ) ;
#23317 = CARTESIAN_POINT ( 'NONE',  ( -20.08610463437157989, 22.20000000546238184, -27.64615127144129758 ) ) ;
#23318 = CARTESIAN_POINT ( 'NONE',  ( -32.50000000000000000, 79.90000000000001990, -10.55989012756945478 ) ) ;
#23319 = CARTESIAN_POINT ( 'NONE',  ( -10.37757302488623701, 17.52500000273120406, 31.93888565452638417 ) ) ;
#23320 = CARTESIAN_POINT ( 'NONE',  ( 3.245314017740486554E-15, -22.99999999999999289, 26.50000000000000355 ) ) ;
#23321 = CARTESIAN_POINT ( 'NONE',  ( -24.50000000000000711, 12.84999999453761532, 7.960532557706201828 ) ) ;
#23322 = CARTESIAN_POINT ( 'NONE',  ( 19.82091636218621034, 11.80000000000000426, 14.40073868116559730 ) ) ;
#23323 = CARTESIAN_POINT ( 'NONE',  ( 7.025853678916867295, 19.44232666574268364, 26.06988505166722803 ) ) ;
#23324 = CARTESIAN_POINT ( 'NONE',  ( 32.50000000000000000, 33.50000000546236834, -3.980102097228898626E-15 ) ) ;
#23325 = CARTESIAN_POINT ( 'NONE',  ( -24.50000000000000711, 10.84999999453761887, 7.960532557706201828 ) ) ;
#23326 = PRODUCT ( 'Linear Compliance Spring & Shaft', 'Linear Compliance Spring & Shaft', '', ( #5103 ) ) ;
#23327 = CARTESIAN_POINT ( 'NONE',  ( -27.16883889988624290, 28.92500000273118133, -19.73931689729374028 ) ) ;
#23328 = CARTESIAN_POINT ( 'NONE',  ( 19.09188309203661049, 43.79687500000000000, -19.09188309203694445 ) ) ;
#23329 = EDGE_LOOP ( 'NONE', ( #32214, #28885, #19788, #17077 ) ) ;
#23330 = CARTESIAN_POINT ( 'NONE',  ( 33.58253175000000113, 64.12500000273118417, -4.112674001490185761E-15 ) ) ;
#23331 = CARTESIAN_POINT ( 'NONE',  ( 20.50609665440969565, 47.23437499999999289, -20.50609665441004736 ) ) ;
#23332 = VECTOR ( 'NONE', #27244, 1000.000000000000000 ) ;
#23333 = ORIENTED_EDGE ( 'NONE', *, *, #24981, .T. ) ;
#23334 = CARTESIAN_POINT ( 'NONE',  ( -28.02196122052045268, 64.42746500092397355, 7.468012846824790607 ) ) ;
#23335 = CARTESIAN_POINT ( 'NONE',  ( 15.04653450569292872, 17.59152750092397355, -25.98046417659857710 ) ) ;
#23336 = ORIENTED_EDGE ( 'NONE', *, *, #10326, .F. ) ;
#23337 = CARTESIAN_POINT ( 'NONE',  ( -20.75514604977248823, 8.825000002731190563, -28.56700777964554305 ) ) ;
#23338 = CARTESIAN_POINT ( 'NONE',  ( 28.02196122052058413, 15.43190999907601935, 7.468012846824272799 ) ) ;
#23339 = CARTESIAN_POINT ( 'NONE',  ( 0.000000000000000000, 11.99999999999999645, 0.000000000000000000 ) ) ;
#23340 = CARTESIAN_POINT ( 'NONE',  ( 33.58253175000000113, 32.47500000273117138, -10.91162601494193751 ) ) ;
#23341 = CARTESIAN_POINT ( 'NONE',  ( -26.29305231718578995, 34.70000000546239249, 19.10302069950538595 ) ) ;
#23342 = AXIS2_PLACEMENT_3D ( 'NONE', #30064, #1575, #3826 ) ;
#23343 = CARTESIAN_POINT ( 'NONE',  ( 15.00000000000000355, 78.90000000000001990, 4.873795443493592394 ) ) ;
#23344 = CARTESIAN_POINT ( 'NONE',  ( 30.02300923189239512, 64.85156249999998579, -2.619432448724977703E-13 ) ) ;
#23345 = CARTESIAN_POINT ( 'NONE',  ( -20.75514604977248112, 21.42500000273120264, 28.56700777964554661 ) ) ;
#23346 = CARTESIAN_POINT ( 'NONE',  ( -32.50000000000000000, 52.40000000546238823, -10.55989012756945300 ) ) ;
#23347 = CARTESIAN_POINT ( 'NONE',  ( -33.58253175000000113, 49.47500000273118559, 10.91162601494193929 ) ) ;
#23348 = CARTESIAN_POINT ( 'NONE',  ( 10.04305231718579705, 30.60000000000000142, 30.90933677959248982 ) ) ;
#23349 = CARTESIAN_POINT ( 'NONE',  ( 6.277390505771533514E-15, 30.49999999999999645, 34.17252228774368916 ) ) ;
#23350 = CARTESIAN_POINT ( 'NONE',  ( 19.82091636218621034, 7.800000000000001599, 14.40073868116559730 ) ) ;
#23351 = CARTESIAN_POINT ( 'NONE',  ( -33.58253175000000113, 67.22500000273117848, 10.91162601494193929 ) ) ;
#23352 = CARTESIAN_POINT ( 'NONE',  ( -29.06502868860481215, 67.00000000000000000, 15.87274502311879232 ) ) ;
#23353 = CARTESIAN_POINT ( 'NONE',  ( -4.300734207923759378, 74.97500000273122112, -13.23629886949340495 ) ) ;
#23354 = CARTESIAN_POINT ( 'NONE',  ( -27.16883889988624290, 63.17500000273118843, -19.73931689729374028 ) ) ;
#23355 = CARTESIAN_POINT ( 'NONE',  ( 0.000000000000000000, 16.99999999999998579, 0.000000000000000000 ) ) ;
#23356 = CARTESIAN_POINT ( 'NONE',  ( 10.37757302488624056, 12.52500000273118452, -31.93888565452638417 ) ) ;
#23357 = CARTESIAN_POINT ( 'NONE',  ( 6.950374756619721595, 29.19309000092397000, 26.09010956794232428 ) ) ;
#23358 = CARTESIAN_POINT ( 'NONE',  ( 5.714234795769584707, 66.99999999999998579, -32.80324308525973720 ) ) ;
#23359 = CARTESIAN_POINT ( 'NONE',  ( 10.37757302488624767, 33.72500000273119269, 31.93888565452638417 ) ) ;
#23360 = CARTESIAN_POINT ( 'NONE',  ( 40.00000000000000000, 52.00000000000000711, 23.09401076758503990 ) ) ;
#23361 = DIRECTION ( 'NONE',  ( -0.000000000000000000, -1.000000000000000000, -0.000000000000000000 ) ) ;
#23362 = CARTESIAN_POINT ( 'NONE',  ( -8.601468415847515203, 75.17500000273118133, 11.83890561707634959 ) ) ;
#23363 = CARTESIAN_POINT ( 'NONE',  ( -20.47846945139866648, 47.51524333240936215, 20.53372385742108008 ) ) ;
#23364 = CARTESIAN_POINT ( 'NONE',  ( -2.092463501923844636E-15, 56.00000000546236123, -34.17252228774368916 ) ) ;
#23365 = CARTESIAN_POINT ( 'NONE',  ( 13.91746825000000065, 76.27500000273116143, 4.522059556121114987 ) ) ;
#23366 = AXIS2_PLACEMENT_3D ( 'NONE', #18595, #3136, #5538 ) ;
#23367 = CARTESIAN_POINT ( 'NONE',  ( -13.97622843553632421, 19.01822916666666785, -24.20753774853731599 ) ) ;
#23368 = CARTESIAN_POINT ( 'NONE',  ( 20.08610463437158344, 63.20000000546237118, 27.64615127144129403 ) ) ;
#23369 = CARTESIAN_POINT ( 'NONE',  ( -20.08610463437156923, 66.80000000546236549, 27.64615127144130113 ) ) ;
#23370 = CARTESIAN_POINT ( 'NONE',  ( 7.505752307973351023, 24.31770833333332504, 28.01184896238290278 ) ) ;
#23371 = CARTESIAN_POINT ( 'NONE',  ( 20.75514604977249178, 38.07500000273116569, 28.56700777964553950 ) ) ;
#23372 = CARTESIAN_POINT ( 'NONE',  ( -18.94512977948575738, 9.924999997268812990, -13.76444248337723231 ) ) ;
#23373 = VERTEX_POINT ( 'NONE', #1110 ) ;
#23374 = CARTESIAN_POINT ( 'NONE',  ( -33.58253175000000113, 77.47500000273120691, 10.91162601494193929 ) ) ;
#23375 = CARTESIAN_POINT ( 'NONE',  ( -10.04305231718578462, 20.90000000546236691, 30.90933677959249337 ) ) ;
#23376 = CARTESIAN_POINT ( 'NONE',  ( -28.01184896238290278, 38.92708333333333570, 7.505752307973363457 ) ) ;
#23377 = CARTESIAN_POINT ( 'NONE',  ( 28.01184896238290278, 57.83333333333333570, -7.505752307973347470 ) ) ;
#23378 = CARTESIAN_POINT ( 'NONE',  ( 10.37757302488624767, 55.97500000273119980, 31.93888565452638417 ) ) ;
#23379 = CARTESIAN_POINT ( 'NONE',  ( -32.50000000000000000, 54.40000000546238823, -10.55989012756945478 ) ) ;
#23380 = LINE ( 'NONE', #28852, #9471 ) ;
#23381 = CARTESIAN_POINT ( 'NONE',  ( -10.37757302488624411, 44.72500000273119269, -31.93888565452638417 ) ) ;
#23382 = CARTESIAN_POINT ( 'NONE',  ( -4.635254915624211769, 75.85000000546237686, -14.26584774442730286 ) ) ;
#23383 = CARTESIAN_POINT ( 'NONE',  ( -20.75514604977248112, 71.67500000273116711, 28.56700777964554661 ) ) ;
#23384 = PRODUCT_DEFINITION ( 'UNKNOWN', '', #9885, #2287 ) ;
#23385 = CARTESIAN_POINT ( 'NONE',  ( -32.50000000000000000, 8.600000005462376862, 10.55989012756946366 ) ) ;
#23386 = CARTESIAN_POINT ( 'NONE',  ( -10.37757302488624411, 60.72500000273119269, -31.93888565452638417 ) ) ;
#23387 = CARTESIAN_POINT ( 'NONE',  ( 11.54700538379251817, 86.00000000000001421, 19.99999999999999645 ) ) ;
#23388 = CARTESIAN_POINT ( 'NONE',  ( 20.08610463437158344, 48.70000000000000284, 27.64615127144129403 ) ) ;
#23389 = CARTESIAN_POINT ( 'NONE',  ( 7.236395654485755280, 4.224999997268802154, 22.27133577429736988 ) ) ;
#23390 = CARTESIAN_POINT ( 'NONE',  ( -33.58253175000000113, 13.37500000273117351, 0.000000000000000000 ) ) ;
#23391 = DIRECTION ( 'NONE',  ( 0.000000000000000000, 0.000000000000000000, -1.000000000000000000 ) ) ;
#23392 = CARTESIAN_POINT ( 'NONE',  ( 7.025853678916867295, 33.19232666574268364, 26.06988505166722803 ) ) ;
#23393 = CARTESIAN_POINT ( 'NONE',  ( 13.91746824999999532, 78.47500000273116427, -4.522059556121118540 ) ) ;
#23394 = CARTESIAN_POINT ( 'NONE',  ( 2.375766604868046361, 74.80125428700920054, 14.99999999999999822 ) ) ;
#23395 = DIRECTION ( 'NONE',  ( 0.8660254037844387076, 0.000000000000000000, 0.5000000000000001110 ) ) ;
#23396 = CARTESIAN_POINT ( 'NONE',  ( -20.75514604977248823, 75.07500000273118701, -28.56700777964554305 ) ) ;
#23397 = ORIENTED_EDGE ( 'NONE', *, *, #21114, .T. ) ;
#23398 = VECTOR ( 'NONE', #13343, 1000.000000000000000 ) ;
#23399 = CARTESIAN_POINT ( 'NONE',  ( 18.94512977948575738, 14.92499999726881654, 13.76444248337723408 ) ) ;
#23400 = CARTESIAN_POINT ( 'NONE',  ( 14.47279130897151767, 6.324999997268824892, 19.92008829642072953 ) ) ;
#23401 = CARTESIAN_POINT ( 'NONE',  ( 13.97622843553633665, 58.54947916666665009, 24.20753774853730889 ) ) ;
#23402 = CARTESIAN_POINT ( 'NONE',  ( -2.162160676586881955E-15, 56.62500000273116996, -35.31076352940723240 ) ) ;
#23403 = CARTESIAN_POINT ( 'NONE',  ( 33.58253175000000113, 20.37500000273119483, -4.112674001490185761E-15 ) ) ;
#23404 = CARTESIAN_POINT ( 'NONE',  ( -10.37757302488624411, 4.975000002731183812, -31.93888565452638417 ) ) ;
#23405 = CARTESIAN_POINT ( 'NONE',  ( 24.20753774853756113, 44.51302083333332860, 13.97622843553589789 ) ) ;
#23406 = CARTESIAN_POINT ( 'NONE',  ( -7.543491769121417612, 22.60454833425730925, 28.00173670424549499 ) ) ;
#23407 = CARTESIAN_POINT ( 'NONE',  ( -14.97647472619899389, 19.87201416574269075, 26.02091320914878025 ) ) ;
#23408 = CARTESIAN_POINT ( 'NONE',  ( -20.08610463437157989, 78.20000000546235697, -27.64615127144129758 ) ) ;
#23409 = CARTESIAN_POINT ( 'NONE',  ( 13.17636326499326671, 51.99999999999998579, -29.96527208688312527 ) ) ;
#23410 = CARTESIAN_POINT ( 'NONE',  ( -10.37757302488624411, 44.72500000273119269, -31.93888565452638417 ) ) ;
#23411 = CARTESIAN_POINT ( 'NONE',  ( -7.236395654485763274, 8.024999997268828622, 22.27133577429736633 ) ) ;
#23412 = DIRECTION ( 'NONE',  ( 0.5000000000000000000, 0.000000000000000000, 0.8660254037844385966 ) ) ;
#23413 = ORIENTED_EDGE ( 'NONE', *, *, #4955, .T. ) ;
#23414 = CARTESIAN_POINT ( 'NONE',  ( 20.75514604977249178, 54.07500000273118701, 28.56700777964553950 ) ) ;
#23415 = CARTESIAN_POINT ( 'NONE',  ( 7.025853678916403666, 38.07329833425730925, -26.06988505166735237 ) ) ;
#23416 = CARTESIAN_POINT ( 'NONE',  ( 20.75514604977248467, 72.67500000273118133, -28.56700777964554305 ) ) ;
#23417 = EDGE_LOOP ( 'NONE', ( #24275, #9549, #29057, #32959, #12083, #11996 ) ) ;
#23418 = CARTESIAN_POINT ( 'NONE',  ( -27.16883889988623935, 23.32500000273117635, 19.73931689729374739 ) ) ;
#23420 = CARTESIAN_POINT ( 'NONE',  ( -2.584737979205441561E-13, 19.30468749999999645, -30.02300923189239512 ) ) ;
#23419 = VECTOR ( 'NONE', #6463, 1000.000000000000000 ) ;
#23421 = ORIENTED_EDGE ( 'NONE', *, *, #26046, .F. ) ;
#23422 =( BOUNDED_CURVE ( )  B_SPLINE_CURVE ( 2, ( #6254, #29580, #18647, #26692, #26355, #2845, #23788, #255, #5589, #16070, #29254, #21383, #31828 ),
 .UNSPECIFIED., .F., .T. ) 
 B_SPLINE_CURVE_WITH_KNOTS ( ( 3, 2, 2, 2, 2, 2, 3 ),
 ( 0.05000000000000000278, 0.05999999999999999778, 0.08000000000000000167, 0.1000000000000000056, 0.1199999999999999956, 0.1400000000000000133, 0.1500000000000000222 ),
 .UNSPECIFIED. ) 
 CURVE ( )  GEOMETRIC_REPRESENTATION_ITEM ( )  RATIONAL_B_SPLINE_CURVE ( ( 0.9755282581475768211, 0.9755282581475768211, 1.000000000000000000, 0.9510565162951535312, 1.000000000000000000, 0.9510565162951535312, 1.000000000000000000, 0.9510565162951535312, 1.000000000000000000, 0.9510565162951535312, 1.000000000000000000, 0.9755282581475767101, 0.9755282581475768211 ) ) 
 REPRESENTATION_ITEM ( '' )  );
#23423 = CARTESIAN_POINT ( 'NONE',  ( 20.08610463437157279, 29.80000000546237615, -27.64615127144129758 ) ) ;
#23424 = CARTESIAN_POINT ( 'NONE',  ( 20.75514604977248467, 64.42500000273116711, -28.56700777964554305 ) ) ;
#23425 = CARTESIAN_POINT ( 'NONE',  ( -7.505752307972844761, 52.10416666666666430, 28.01184896238304134 ) ) ;
#23426 = VECTOR ( 'NONE', #5306, 1000.000000000000000 ) ;
#23427 = CARTESIAN_POINT ( 'NONE',  ( -24.50000000000000000, 6.649999994537635573, -7.960532557706207157 ) ) ;
#23428 = CARTESIAN_POINT ( 'NONE',  ( -23.41746824999999887, 4.024999997268810858, -7.608796670333730638 ) ) ;
#23429 = EDGE_CURVE ( 'NONE', #52, #32793, #25912, .T. ) ;
#23430 = CARTESIAN_POINT ( 'NONE',  ( -27.16883889988624290, 2.925000002731187543, -19.73931689729374028 ) ) ;
#23431 = CARTESIAN_POINT ( 'NONE',  ( -28.02196122052058413, 58.40065999907601935, -7.468012846824272799 ) ) ;
#23432 = CARTESIAN_POINT ( 'NONE',  ( -24.50000000000000000, 15.00000000000001421, -3.000384657911015469E-15 ) ) ;
#23433 = CARTESIAN_POINT ( 'NONE',  ( -7.505752307973343918, 63.84895833333332860, -28.01184896238290989 ) ) ;
#23434 = CARTESIAN_POINT ( 'NONE',  ( -10.04305231718579172, 3.599999999999992095, -30.90933677959248982 ) ) ;
#23435 = CARTESIAN_POINT ( 'NONE',  ( -20.08610463437157989, 19.69999999999998863, -27.64615127144129758 ) ) ;
#23436 = CARTESIAN_POINT ( 'NONE',  ( 6.988114217767829928, 64.13541666666667140, -26.07999730980489872 ) ) ;
#23437 = CARTESIAN_POINT ( 'NONE',  ( -15.14183272437241889, 10.44999999453763095, -20.84094480462497856 ) ) ;
#23438 = CARTESIAN_POINT ( 'NONE',  ( -12.13525491562421088, 72.05000000546237970, -8.816778784387096835 ) ) ;
#23439 = CARTESIAN_POINT ( 'NONE',  ( 26.07999730980477437, 20.02083333333332860, -6.988114217768290004 ) ) ;
#23440 = CARTESIAN_POINT ( 'NONE',  ( -10.37757302488623701, 29.52500000273117209, 31.93888565452638417 ) ) ;
#23441 = CARTESIAN_POINT ( 'NONE',  ( 15.00000000000000000, 75.10000000000000853, -4.873795443493596835 ) ) ;
#23442 = CARTESIAN_POINT ( 'NONE',  ( -10.37757302488624411, 36.97500000273119980, -31.93888565452638417 ) ) ;
#23443 = CARTESIAN_POINT ( 'NONE',  ( 27.16883889988623935, 24.57500000273119056, -19.73931689729374384 ) ) ;
#23444 = CARTESIAN_POINT ( 'NONE',  ( -1.778240108872766143E-15, 63.50000000000000000, -32.49999999999999289 ) ) ;
#23445 = CARTESIAN_POINT ( 'NONE',  ( -26.09010956794232428, 50.67746500092398065, 6.950374756619732253 ) ) ;
#23446 = CARTESIAN_POINT ( 'NONE',  ( 6.486482029760648627E-15, 73.62500000273118417, 35.31076352940722529 ) ) ;
#23447 = EDGE_CURVE ( 'NONE', #12812, #19067, #29413, .T. ) ;
#23448 = DIRECTION ( 'NONE',  ( -0.000000000000000000, -1.000000000000000000, -0.000000000000000000 ) ) ;
#23449 = CARTESIAN_POINT ( 'NONE',  ( 20.08610463437158344, 60.70000000000000284, 27.64615127144129403 ) ) ;
#23450 = LINE ( 'NONE', #33911, #22132 ) ;
#23451 = CARTESIAN_POINT ( 'NONE',  ( 27.16883889988624290, 61.92500000273118133, 19.73931689729373673 ) ) ;
#23452 = CARTESIAN_POINT ( 'NONE',  ( -18.94512977948575738, 9.924999997268812990, -13.76444248337723231 ) ) ;
#23453 = CARTESIAN_POINT ( 'NONE',  ( -10.37757302488624411, 74.97500000273120691, -31.93888565452638417 ) ) ;
#23454 = CARTESIAN_POINT ( 'NONE',  ( -10.37757302488624411, 6.725000002731185589, -31.93888565452638417 ) ) ;
#23455 = CARTESIAN_POINT ( 'NONE',  ( -18.94512977948575738, 17.92499999726882010, -13.76444248337723231 ) ) ;
#23456 = CARTESIAN_POINT ( 'NONE',  ( 27.95245687107223986, 18.16444416759064140, 0.04044903254993640479 ) ) ;
#23457 = ORIENTED_EDGE ( 'NONE', *, *, #23095, .T. ) ;
#23458 = CARTESIAN_POINT ( 'NONE',  ( -20.75514604977248823, 42.82500000273119412, -28.56700777964554305 ) ) ;
#23459 = EDGE_LOOP ( 'NONE', ( #1993, #30715, #4880, #21058 ) ) ;
#23460 = CARTESIAN_POINT ( 'NONE',  ( 20.50609665441005092, 44.65624999999999289, 20.50609665440969209 ) ) ;
#23461 = DIRECTION ( 'NONE',  ( -1.224646799147353454E-16, 1.000000000000000000, -0.000000000000000000 ) ) ;
#23462 = CARTESIAN_POINT ( 'NONE',  ( -26.29305231718578995, 2.700000005462374730, 19.10302069950538595 ) ) ;
#23463 = CARTESIAN_POINT ( 'NONE',  ( -33.58253175000000113, 79.02500000273118985, -10.91162601494193218 ) ) ;
#23464 = CARTESIAN_POINT ( 'NONE',  ( -14.47279130897152122, 6.424999997268821872, 19.92008829642072243 ) ) ;
#23465 = CARTESIAN_POINT ( 'NONE',  ( -24.50000000000000355, 0.9000000000000005773, -7.960532557706207157 ) ) ;
#23466 = CARTESIAN_POINT ( 'NONE',  ( -27.16883889988623935, 13.57500000273120833, 19.73931689729374739 ) ) ;
#23467 = CARTESIAN_POINT ( 'NONE',  ( 6.277390505771533514E-15, 56.49999999999998579, 34.17252228774368916 ) ) ;
#23468 = DIRECTION ( 'NONE',  ( -0.000000000000000000, -1.000000000000000000, -0.000000000000000000 ) ) ;
#23469 = CARTESIAN_POINT ( 'NONE',  ( 0.000000000000000000, 80.00000000000001421, 0.000000000000000000 ) ) ;
#23470 = CARTESIAN_POINT ( 'NONE',  ( -14.97647472619899389, 30.18451416574268720, 26.02091320914878025 ) ) ;
#23471 = CARTESIAN_POINT ( 'NONE',  ( -11.25946833292375793, 73.57500000273120122, 8.180482586598737171 ) ) ;
#23472 = CARTESIAN_POINT ( 'NONE',  ( 20.50609665441005092, 41.21875000000000000, 20.50609665440969209 ) ) ;
#23473 = PRODUCT_CONTEXT ( 'NONE', #869, 'mechanical' ) ;
#23474 = CARTESIAN_POINT ( 'NONE',  ( 0.000000000000000000, 82.00000000000001421, 0.000000000000000000 ) ) ;
#23475 = CARTESIAN_POINT ( 'NONE',  ( 10.04305231718578817, 65.40000000000001990, -30.90933677959249337 ) ) ;
#23476 = CARTESIAN_POINT ( 'NONE',  ( -10.04305231718578462, 10.39999999999999325, 30.90933677959249337 ) ) ;
#23477 = VECTOR ( 'NONE', #7170, 1000.000000000000000 ) ;
#23478 = CARTESIAN_POINT ( 'NONE',  ( 10.69578794377714281, -43.58578643762690064, 2.566657756148792685E-15 ) ) ;
#23479 = CARTESIAN_POINT ( 'NONE',  ( 19.06425588902558133, 49.23399333240936215, -19.11951029504797006 ) ) ;
#23480 = CARTESIAN_POINT ( 'NONE',  ( -33.58253175000000113, 51.02500000273119696, -10.91162601494193218 ) ) ;
#23481 = CARTESIAN_POINT ( 'NONE',  ( -33.58253175000000113, 53.27500000273117564, -10.91162601494193218 ) ) ;
#23482 = CARTESIAN_POINT ( 'NONE',  ( 33.58253175000000113, 40.37500000273119838, -4.112674001490185761E-15 ) ) ;
#23483 = CARTESIAN_POINT ( 'NONE',  ( 26.29305231718578995, 25.19999999999999929, -19.10302069950538240 ) ) ;
#23484 = CARTESIAN_POINT ( 'NONE',  ( 24.20753774853756113, 13.57552083333333037, 13.97622843553589789 ) ) ;
#23485 = VECTOR ( 'NONE', #31862, 1000.000000000000000 ) ;
#23486 = CARTESIAN_POINT ( 'NONE',  ( 1.415442245121193876, 16.99999999999998934, -23.63911378103994920 ) ) ;
#23487 = CARTESIAN_POINT ( 'NONE',  ( -20.08610463437157989, 79.70000000000000284, -27.64615127144129758 ) ) ;
#23488 = VECTOR ( 'NONE', #19339, 1000.000000000000114 ) ;
#23489 = CARTESIAN_POINT ( 'NONE',  ( 10.37757302488624767, 17.72500000273118204, 31.93888565452638417 ) ) ;
#23490 = CARTESIAN_POINT ( 'NONE',  ( 5.147494310547426899, 7.448745718453160691, -32.50000000000000000 ) ) ;
#23491 = CARTESIAN_POINT ( 'NONE',  ( 0.000000000000000000, 80.00000000000001421, -32.50000000000000000 ) ) ;
#23492 = CARTESIAN_POINT ( 'NONE',  ( -5.147494310547430452, 39.55125428154684641, -32.49999999999999289 ) ) ;
#23493 = CARTESIAN_POINT ( 'NONE',  ( 14.01125832528330051, 19.29909749907602290, 24.18731323226221974 ) ) ;
#23494 = CARTESIAN_POINT ( 'NONE',  ( 26.29305231718579350, 37.30000000546239391, 19.10302069950537529 ) ) ;
#23495 = EDGE_CURVE ( 'NONE', #7658, #11742, #11430, .T. ) ;
#23496 = CARTESIAN_POINT ( 'NONE',  ( 4.023268246324634798E-14, 10.24999999453763166, -24.50000000000000355 ) ) ;
#23497 = CARTESIAN_POINT ( 'NONE',  ( 10.37757302488624056, 28.52500000273120051, -31.93888565452638417 ) ) ;
#23498 = CARTESIAN_POINT ( 'NONE',  ( 2.584737979205441561E-13, 41.64843750000000000, 27.95245687107222921 ) ) ;
#23499 = EDGE_CURVE ( 'NONE', #28763, #27323, #12987, .T. ) ;
#23500 = ORIENTED_EDGE ( 'NONE', *, *, #23857, .F. ) ;
#23501 = CARTESIAN_POINT ( 'NONE',  ( 27.16883889988623935, 60.32500000273120833, -19.73931689729374384 ) ) ;
#23502 = CARTESIAN_POINT ( 'NONE',  ( 20.50609665441005092, 48.09375000000000000, 20.50609665440969209 ) ) ;
#23503 = ORIENTED_EDGE ( 'NONE', *, *, #7258, .T. ) ;
#23504 = CARTESIAN_POINT ( 'NONE',  ( -28.00173670424549499, 64.71392333425730214, -7.543491769121417612 ) ) ;
#23505 = CARTESIAN_POINT ( 'NONE',  ( -7.468012846824771955, 13.72434000092397532, -28.02196122052045624 ) ) ;
#23506 = CARTESIAN_POINT ( 'NONE',  ( -33.58253175000000113, 3.225000002731179372, 10.91162601494193929 ) ) ;
#23507 = CARTESIAN_POINT ( 'NONE',  ( 23.41746824999999887, 18.87499999726882649, 0.000000000000000000 ) ) ;
#23508 = CARTESIAN_POINT ( 'NONE',  ( 6.486482029760649416E-15, 35.87500000273118417, 35.31076352940723240 ) ) ;
#23509 = CARTESIAN_POINT ( 'NONE',  ( -26.29305231718579350, 38.30000000546237970, -19.10302069950537884 ) ) ;
#23510 = CARTESIAN_POINT ( 'NONE',  ( -12.13525491562420910, 74.19999999999998863, 8.816778784387098611 ) ) ;
#23511 = CARTESIAN_POINT ( 'NONE',  ( -1.778240108872766143E-15, 53.50000000000000000, -32.49999999999999289 ) ) ;
#23512 = CARTESIAN_POINT ( 'NONE',  ( 33.58253175000000113, 26.12500000273118417, -4.112674001490185761E-15 ) ) ;
#23513 = CARTESIAN_POINT ( 'NONE',  ( 27.16883889988624290, 50.17500000273117422, 19.73931689729373673 ) ) ;
#23514 = CARTESIAN_POINT ( 'NONE',  ( -20.08610463437156923, 28.30000000000000782, 27.64615127144130113 ) ) ;
#23515 = CARTESIAN_POINT ( 'NONE',  ( 26.29305231718578995, 29.20000000000000284, -19.10302069950538240 ) ) ;
#23516 = CARTESIAN_POINT ( 'NONE',  ( -7.570916362186210335, 2.599999999999991207, -23.30088464923126779 ) ) ;
#23517 =( BOUNDED_CURVE ( )  B_SPLINE_CURVE ( 2, ( #1753, #14986, #25456, #1932, #18083, #3255, #10186, #31897, #4684, #31109, #327, #30937, #9834, #29155, #10015, #15511, #10980, #20669, #23228, #5026, #18719, #3094, #7430, #2457, #17917, #7603, #20311, #10814, #25792, #20486, #5661, #28369, #15163, #28531, #25629, #4857, #30761, #21294, #2108, #17738, #31734, #12581, #2281, #25963, #15337, #16144, #13565, #26597, #33687, #24028, #497, #7251, #21454, #28196, #12923, #12756, #8393, #23400, #23051, #8225, #18878, #29327, #5829, #16308, #26763, #13725, #24190, #33510, #11639, #8728, #6498, #11812, #24849, #6661, #27092, #8895, #14058, #14562, #32733, #19546, #3586, #22288, #14393, #11310, #29825, #32064, #16806, #19212, #11475, #29649, #6329, #24520, #9065, #19379, #990, #5990, #32566, #26922, #3418, #27262, #662, #3753, #29487, #11150, #6152, #21621, #14227, #24683, #27596, #21949, #9226, #16467, #32400, #1157, #21788, #8564, #29994, #829, #22123, #1329, #16971, #16636, #19048, #27429, #19710, #3920, #30156, #32236, #17143, #4087, #13892, #24359, #28111, #33598, #15075, #17650, #10098, #6825, #6999, #27943, #2021, #20398, #1669, #4939, #25543, #4256, #22793, #30849, #12496, #23132, #9921, #17481, #12663, #18003, #2189, #9744, #33424, #7168, #33246, #30329, #1501, #20230, #4426, #7340, #30670 ),
 .UNSPECIFIED., .F., .F. ) 
 B_SPLINE_CURVE_WITH_KNOTS ( ( 3, 2, 2, 2, 2, 2, 2, 2, 2, 2, 2, 2, 2, 2, 2, 2, 2, 2, 2, 2, 2, 2, 2, 2, 2, 2, 2, 2, 2, 2, 2, 2, 2, 2, 2, 2, 2, 2, 2, 2, 2, 2, 2, 2, 2, 2, 2, 2, 2, 2, 2, 2, 2, 2, 2, 2, 2, 2, 2, 2, 2, 2, 2, 2, 2, 2, 2, 2, 2, 2, 2, 2, 2, 2, 2, 2, 2, 2, 2, 2, 2, 2, 3 ),
 ( 0.000000000000000000, 0.01111111111111111154, 0.02222222222222222307, 0.03333333333333333287, 0.04444444444444444614, 0.05555555555555555247, 0.06666666666666666574, 0.07777777777777777901, 0.08888888888888889228, 0.1000000000000000056, 0.1111111111111111049, 0.1222222222222222182, 0.1333333333333333315, 0.1444444444444444309, 0.1555555555555555580, 0.1666666666666666574, 0.1777777777777777846, 0.1888888888888888840, 0.2000000000000000111, 0.2111111111111111105, 0.2222222222222222099, 0.2333333333333333370, 0.2444444444444444364, 0.2555555555555555358, 0.2666666666666666630, 0.2777777777777777901, 0.2888888888888888618, 0.2999999999999999889, 0.3111111111111111160, 0.3222222222222222432, 0.3333333333333333148, 0.3444444444444444420, 0.3555555555555555691, 0.3666666666666666408, 0.3777777777777777679, 0.3888888888888888951, 0.4000000000000000222, 0.4111111111111110938, 0.4222222222222222210, 0.4333333333333334036, 0.4444444444444444198, 0.4555555555555555469, 0.4666666666666666741, 0.4777777777777777457, 0.4888888888888888729, 0.5000000000000000000, 0.5111111111111110716, 0.5222222222222222543, 0.5333333333333333259, 0.5444444444444443976, 0.5555555555555555802, 0.5666666666666666519, 0.5777777777777777235, 0.5888888888888889062, 0.5999999999999999778, 0.6111111111111111605, 0.6222222222222222321, 0.6333333333333331927, 0.6444444444444444864, 0.6555555555555555580, 0.6666666666666666297, 0.6777777777777778123, 0.6888888888888888840, 0.6999999999999999556, 0.7111111111111111382, 0.7222222222222222099, 0.7333333333333332815, 0.7444444444444444642, 0.7555555555555555358, 0.7666666666666667185, 0.7777777777777777901, 0.7888888888888888618, 0.8000000000000000444, 0.8111111111111111160, 0.8222222222222221877, 0.8333333333333333703, 0.8444444444444444420, 0.8555555555555555136, 0.8666666666666668073, 0.8777777777777777679, 0.8888888888888888395, 0.9000000000000000222, 0.9096763566646446364 ),
 .UNSPECIFIED. ) 
 CURVE ( )  GEOMETRIC_REPRESENTATION_ITEM ( )  RATIONAL_B_SPLINE_CURVE ( ( 1.000000000000000000, 0.9510565162951535312, 1.000000000000000000, 0.9510565162951535312, 1.000000000000000000, 0.9510565162951535312, 1.000000000000000000, 0.9510565162951535312, 1.000000000000000000, 0.9510565162951535312, 1.000000000000000000, 0.9510565162951535312, 1.000000000000000000, 0.9510565162951535312, 1.000000000000000000, 0.9510565162951535312, 1.000000000000000000, 0.9510565162951535312, 1.000000000000000000, 0.9510565162951535312, 1.000000000000000000, 0.9510565162951535312, 1.000000000000000000, 0.9510565162951535312, 1.000000000000000000, 0.9510565162951535312, 1.000000000000000000, 0.9510565162951535312, 1.000000000000000000, 0.9510565162951535312, 1.000000000000000000, 0.9510565162951535312, 1.000000000000000000, 0.9510565162951535312, 1.000000000000000000, 0.9510565162951535312, 1.000000000000000000, 0.9510565162951535312, 1.000000000000000000, 0.9510565162951535312, 1.000000000000000000, 0.9510565162951535312, 1.000000000000000000, 0.9510565162951535312, 1.000000000000000000, 0.9510565162951535312, 1.000000000000000000, 0.9510565162951535312, 1.000000000000000000, 0.9510565162951535312, 1.000000000000000000, 0.9510565162951535312, 1.000000000000000000, 0.9510565162951535312, 1.000000000000000000, 0.9510565162951535312, 1.000000000000000000, 0.9510565162951535312, 1.000000000000000000, 0.9510565162951535312, 1.000000000000000000, 0.9510565162951535312, 1.000000000000000000, 0.9510565162951535312, 1.000000000000000000, 0.9510565162951535312, 1.000000000000000000, 0.9510565162951535312, 1.000000000000000000, 0.9510565162951535312, 1.000000000000000000, 0.9510565162951535312, 1.000000000000000000, 0.9510565162951535312, 1.000000000000000000, 0.9510565162951535312, 1.000000000000000000, 0.9510565162951535312, 1.000000000000000000, 0.9510565162951535312, 1.000000000000000000, 0.9510565162951535312, 1.000000000000000000, 0.9510565162951535312, 1.000000000000000000, 0.9510565162951535312, 1.000000000000000000, 0.9510565162951535312, 1.000000000000000000, 0.9510565162951535312, 1.000000000000000000, 0.9510565162951535312, 1.000000000000000000, 0.9510565162951535312, 1.000000000000000000, 0.9510565162951535312, 1.000000000000000000, 0.9510565162951535312, 1.000000000000000000, 0.9510565162951535312, 1.000000000000000000, 0.9510565162951535312, 1.000000000000000000, 0.9510565162951535312, 1.000000000000000000, 0.9510565162951535312, 1.000000000000000000, 0.9510565162951535312, 1.000000000000000000, 0.9510565162951535312, 1.000000000000000000, 0.9510565162951535312, 1.000000000000000000, 0.9510565162951535312, 1.000000000000000000, 0.9510565162951535312, 1.000000000000000000, 0.9510565162951535312, 1.000000000000000000, 0.9510565162951535312, 1.000000000000000000, 0.9510565162951535312, 1.000000000000000000, 0.9510565162951535312, 1.000000000000000000, 0.9510565162951535312, 1.000000000000000000, 0.9510565162951535312, 1.000000000000000000, 0.9510565162951535312, 1.000000000000000000, 0.9510565162951535312, 1.000000000000000000, 0.9510565162951535312, 1.000000000000000000, 0.9510565162951535312, 1.000000000000000000, 0.9510565162951535312, 1.000000000000000000, 0.9510565162951535312, 1.000000000000000000, 0.9510565162951535312, 1.000000000000000000, 0.9510565162951535312, 1.000000000000000000, 0.9510565162951535312, 1.000000000000000000, 0.9510565162951535312, 1.000000000000000000, 0.9510565162951535312, 1.000000000000000000, 0.9510565162951535312, 1.000000000000000000, 0.9510565162951535312, 1.000000000000000000, 0.9510565162951535312, 1.000000000000000000, 0.9510565162951535312, 1.000000000000000000, 0.9510565162951535312, 1.000000000000000000, 0.9510565162951535312, 1.000000000000000000, 0.9573764855735513724, 0.9889922301674725080 ) ) 
 REPRESENTATION_ITEM ( '' )  );
#23518 = CARTESIAN_POINT ( 'NONE',  ( -10.37757302488623701, 67.52500000273120406, 31.93888565452638417 ) ) ;
#23519 = CARTESIAN_POINT ( 'NONE',  ( 7.570916362186213000, 2.149999994537632464, -23.30088464923126423 ) ) ;
#23520 = CARTESIAN_POINT ( 'NONE',  ( -9.688038132598597585, 73.99999999999998579, -11.40930151615730814 ) ) ;
#23521 = CARTESIAN_POINT ( 'NONE',  ( 10.37757302488624056, 62.77500000273117564, -31.93888565452638417 ) ) ;
#23522 = DIRECTION ( 'NONE',  ( 0.000000000000000000, 0.000000000000000000, -1.000000000000000000 ) ) ;
#23523 = CARTESIAN_POINT ( 'NONE',  ( -10.37757302488624411, 12.72500000273119092, -31.93888565452638417 ) ) ;
#23524 = CARTESIAN_POINT ( 'NONE',  ( -13.94119854578936923, 34.20611083425730925, -24.22776226481241224 ) ) ;
#23525 = CARTESIAN_POINT ( 'NONE',  ( -3.724851327375141796, 66.99999999999997158, -33.24794091741932789 ) ) ;
#23526 = CARTESIAN_POINT ( 'NONE',  ( -33.58253175000000113, 3.375000002731193049, 0.000000000000000000 ) ) ;
#23527 = CARTESIAN_POINT ( 'NONE',  ( -10.37757302488623701, 37.52500000273118985, 31.93888565452638417 ) ) ;
#23528 = CARTESIAN_POINT ( 'NONE',  ( 32.50000000000000000, 45.50000000546239676, -3.980102097228898626E-15 ) ) ;
#23529 = CARTESIAN_POINT ( 'NONE',  ( 20.08610463437157279, 19.30000000000000071, -27.64615127144129758 ) ) ;
#23530 = CARTESIAN_POINT ( 'NONE',  ( 12.23270501248084585, 74.03838462613526872, -6.840937216516965513 ) ) ;
#23531 = CARTESIAN_POINT ( 'NONE',  ( 25.98046417659831775, 45.93972249907602645, -15.04653450569338879 ) ) ;
#23532 = CARTESIAN_POINT ( 'NONE',  ( 32.50000000000000000, 55.50000000546238965, -3.980102097228898626E-15 ) ) ;
#23533 = EDGE_CURVE ( 'NONE', #20505, #16826, #7476, .T. ) ;
#23534 = CARTESIAN_POINT ( 'NONE',  ( 8.601468415847520532, 78.07500000273120122, 11.83890561707634781 ) ) ;
#23535 =( NAMED_UNIT ( * ) PLANE_ANGLE_UNIT ( ) SI_UNIT ( $, .RADIAN. ) );
#23536 = CARTESIAN_POINT ( 'NONE',  ( -2.428612866367529427E-13, 12.42968749999999289, -27.95245687107222921 ) ) ;
#23537 = CARTESIAN_POINT ( 'NONE',  ( -26.29305231718579350, 53.80000000000001137, -19.10302069950537884 ) ) ;
#23538 = ADVANCED_FACE ( 'NONE', ( #6453 ), #27385, .F. ) ;
#23539 = CARTESIAN_POINT ( 'NONE',  ( 32.50000000000000711, 67.40000000546237402, 10.55989012756945122 ) ) ;
#23540 = CARTESIAN_POINT ( 'NONE',  ( -7.505752307973343918, 26.03645833333333215, -28.01184896238290989 ) ) ;
#23541 = CARTESIAN_POINT ( 'NONE',  ( 20.75514604977248467, 34.67500000273118843, -28.56700777964554305 ) ) ;
#23542 = CARTESIAN_POINT ( 'NONE',  ( -23.41746824999999887, 12.02499999726881974, -7.608796670333730638 ) ) ;
#23543 = ORIENTED_EDGE ( 'NONE', *, *, #13660, .T. ) ;
#23544 = CARTESIAN_POINT ( 'NONE',  ( 20.53372385742072481, 41.79725666759063785, -20.47846945139902175 ) ) ;
#23545 = CARTESIAN_POINT ( 'NONE',  ( -10.04305231718579172, 26.10000000546238041, -30.90933677959248982 ) ) ;
#23546 = CARTESIAN_POINT ( 'NONE',  ( -2.584737979205441561E-13, 46.80468750000000000, -30.02300923189239512 ) ) ;
#23547 = CARTESIAN_POINT ( 'NONE',  ( -20.08610463437157989, 35.70000000000000995, -27.64615127144129758 ) ) ;
#23548 = CARTESIAN_POINT ( 'NONE',  ( 27.16883889988624290, 56.17500000273118133, 19.73931689729373673 ) ) ;
#23549 = CARTESIAN_POINT ( 'NONE',  ( -10.04305231718579172, 54.10000000546239107, -30.90933677959248982 ) ) ;
#23550 = CARTESIAN_POINT ( 'NONE',  ( 5.779280353836490358E-15, 11.00000000546238077, 32.49999999999999289 ) ) ;
#23551 = CARTESIAN_POINT ( 'NONE',  ( -20.75514604977248823, 44.82500000273117990, -28.56700777964554305 ) ) ;
#23552 = CARTESIAN_POINT ( 'NONE',  ( -1.089172066684569321E-14, 76.75000000546238255, 15.00000000000000000 ) ) ;
#23553 = CARTESIAN_POINT ( 'NONE',  ( 27.16883889988624290, 70.17500000273119554, 19.73931689729373673 ) ) ;
#23554 = DIRECTION ( 'NONE',  ( -0.000000000000000000, -1.000000000000000000, -0.000000000000000000 ) ) ;
#23555 = CARTESIAN_POINT ( 'NONE',  ( 33.58253175000000823, 62.02500000273116854, 10.91162601494192685 ) ) ;
#23556 = CARTESIAN_POINT ( 'NONE',  ( -26.00068869287368756, 22.16927083333332860, -15.01150461594595775 ) ) ;
#23557 = CARTESIAN_POINT ( 'NONE',  ( 20.08610463437157279, 45.29999999999999005, -27.64615127144129758 ) ) ;
#23558 = CARTESIAN_POINT ( 'NONE',  ( 14.47279130897151589, 6.324999997268824892, 19.92008829642072953 ) ) ;
#23559 = CARTESIAN_POINT ( 'NONE',  ( -20.75514604977248823, 13.07500000273120300, -28.56700777964554305 ) ) ;
#23560 = CARTESIAN_POINT ( 'NONE',  ( -20.08610463437157989, 66.20000000546238539, -27.64615127144129758 ) ) ;
#23561 = CARTESIAN_POINT ( 'NONE',  ( 19.06425588902558133, 32.04649333240934084, -19.11951029504797006 ) ) ;
#23562 = CARTESIAN_POINT ( 'NONE',  ( 2.688165632520823219E-15, 79.87500000273118417, 14.63369212191046387 ) ) ;
#23563 = CARTESIAN_POINT ( 'NONE',  ( 33.58253175000000113, 76.37500000273116996, -4.112674001490185761E-15 ) ) ;
#23564 = CARTESIAN_POINT ( 'NONE',  ( -8.891200544363830713E-16, 75.50000000000000000, -15.00000000000000000 ) ) ;
#23565 = CARTESIAN_POINT ( 'NONE',  ( 20.75514604977249178, 78.07500000273117280, 28.56700777964553950 ) ) ;
#23566 = ORIENTED_EDGE ( 'NONE', *, *, #2571, .T. ) ;
#23567 = CARTESIAN_POINT ( 'NONE',  ( -14.47279130897152122, 18.42499999726882365, 19.92008829642072243 ) ) ;
#23568 = CARTESIAN_POINT ( 'NONE',  ( -6.988114217767819270, 55.54166666666667140, 26.07999730980490583 ) ) ;
#23569 = CARTESIAN_POINT ( 'NONE',  ( 33.58253175000000113, 56.12500000273119838, -4.112674001490185761E-15 ) ) ;
#23570 = CARTESIAN_POINT ( 'NONE',  ( 33.58253175000000113, 14.47500000273118737, -10.91162601494193751 ) ) ;
#23571 = CARTESIAN_POINT ( 'NONE',  ( 10.37757302488624767, 5.975000002731184701, 31.93888565452638417 ) ) ;
#23572 = CARTESIAN_POINT ( 'NONE',  ( -24.20753774853730889, 38.78385416666665719, 13.97622843553634020 ) ) ;
#23573 = CARTESIAN_POINT ( 'NONE',  ( 14.97647472619947351, 32.48736083425731636, 26.02091320914850314 ) ) ;
#23574 = CARTESIAN_POINT ( 'NONE',  ( 28.02196122052058413, 15.43190999907601935, 7.468012846824272799 ) ) ;
#23575 = CARTESIAN_POINT ( 'NONE',  ( 32.50000000000000711, 71.40000000546241665, 10.55989012756945122 ) ) ;
#23576 = CARTESIAN_POINT ( 'NONE',  ( -5.147494310547423346, 56.94874572391554324, 32.50000000000000000 ) ) ;
#23577 = CARTESIAN_POINT ( 'NONE',  ( 33.58253175000000823, 40.02500000273119696, 10.91162601494192685 ) ) ;
#23578 = CARTESIAN_POINT ( 'NONE',  ( 24.18731323226221974, 45.93972249907602645, -14.01125832528328985 ) ) ;
#23579 = CARTESIAN_POINT ( 'NONE',  ( 14.47279130897151767, 8.924999997268800556, -19.92008829642072598 ) ) ;
#23580 = PRODUCT_DEFINITION_SHAPE ( 'NONE', 'NONE',  #78 ) ;
#23581 = CARTESIAN_POINT ( 'NONE',  ( -10.04305231718579172, 2.100000005462371533, -30.90933677959248982 ) ) ;
#23582 = ORIENTED_EDGE ( 'NONE', *, *, #17122, .T. ) ;
#23583 = CARTESIAN_POINT ( 'NONE',  ( -33.58253175000000113, 53.37500000273119838, 0.000000000000000000 ) ) ;
#23584 = CARTESIAN_POINT ( 'NONE',  ( -9.270509831248419985, 70.55000000546236549, 12.75976212528060039 ) ) ;
#23585 = CARTESIAN_POINT ( 'NONE',  ( -24.18731323226248264, 40.79465250092398065, -14.01125832528284931 ) ) ;
#23586 = CARTESIAN_POINT ( 'NONE',  ( -20.75514604977248823, 77.07500000273117280, -28.56700777964554305 ) ) ;
#23587 = ORIENTED_EDGE ( 'NONE', *, *, #18889, .F. ) ;
#23588 = CARTESIAN_POINT ( 'NONE',  ( -2.162160676586881955E-15, 26.62500000273118417, -35.31076352940723240 ) ) ;
#23589 = CARTESIAN_POINT ( 'NONE',  ( -28.01184896238290278, 18.30208333333332860, 7.505752307973363457 ) ) ;
#23590 = VERTEX_POINT ( 'NONE', #12099 ) ;
#23591 = PLANE ( 'NONE',  #22609 ) ;
#23592 = CARTESIAN_POINT ( 'NONE',  ( -20.75514604977248112, 63.42500000273118133, 28.56700777964554661 ) ) ;
#23593 = CARTESIAN_POINT ( 'NONE',  ( 26.00068869287367335, 44.51302083333331439, 15.01150461594596308 ) ) ;
#23594 = CARTESIAN_POINT ( 'NONE',  ( -7.570916362186210335, 6.349999994537613546, -23.30088464923126779 ) ) ;
#23595 = CARTESIAN_POINT ( 'NONE',  ( -18.94512977948575738, 11.92499999726881477, -13.76444248337723231 ) ) ;
#23596 = CARTESIAN_POINT ( 'NONE',  ( -27.16883889988623935, 3.325000002731171023, 19.73931689729374739 ) ) ;
#23597 = CARTESIAN_POINT ( 'NONE',  ( -8.891200544363830713E-16, 77.75000000546236834, -15.00000000000000000 ) ) ;
#23598 = CARTESIAN_POINT ( 'NONE',  ( 7.468012846824281681, 62.69753499907601224, -28.02196122052058058 ) ) ;
#23599 = CARTESIAN_POINT ( 'NONE',  ( 10.04305231718579705, 36.59999999999999432, 30.90933677959248982 ) ) ;
#23600 = CARTESIAN_POINT ( 'NONE',  ( -15.01150461594595775, 65.99739583333332860, 26.00068869287368756 ) ) ;
#23601 = CARTESIAN_POINT ( 'NONE',  ( 6.277390505771533514E-15, 14.50000000000000888, 34.17252228774368916 ) ) ;
#23602 = CARTESIAN_POINT ( 'NONE',  ( 26.07999730980490227, 64.99479166666665719, 6.988114217767821046 ) ) ;
#23603 = CARTESIAN_POINT ( 'NONE',  ( 15.14183272437242245, 14.04999999453763593, -20.84094480462497856 ) ) ;
#23604 = CARTESIAN_POINT ( 'NONE',  ( -12.13525491562421088, 74.05000000546237970, -8.816778784387096835 ) ) ;
#23605 = CARTESIAN_POINT ( 'NONE',  ( -13.97622843553632421, 29.33072916666665719, -24.20753774853731599 ) ) ;
#23606 = CARTESIAN_POINT ( 'NONE',  ( -20.75514604977248823, 32.82500000273118701, -28.56700777964554305 ) ) ;
#23607 = CARTESIAN_POINT ( 'NONE',  ( -27.16883889988623935, 75.32500000273118701, 19.73931689729374739 ) ) ;
#23608 = CARTESIAN_POINT ( 'NONE',  ( -2.162160676586881955E-15, 34.87500000273117706, -35.31076352940723240 ) ) ;
#23609 = CARTESIAN_POINT ( 'NONE',  ( -27.16883889988624290, 13.17500000273119554, -19.73931689729374028 ) ) ;
#23610 = CARTESIAN_POINT ( 'NONE',  ( -8.891200544363830713E-16, 79.50000000000001421, -15.00000000000000000 ) ) ;
#23611 = CARTESIAN_POINT ( 'NONE',  ( 13.94119854578937812, 53.11236083425731636, 24.22776226481240514 ) ) ;
#23612 = CARTESIAN_POINT ( 'NONE',  ( 20.75514604977249178, 77.82500000273120122, 28.56700777964553950 ) ) ;
#23613 = CARTESIAN_POINT ( 'NONE',  ( 24.50000000000000000, 7.900000000000012790, 7.960532557706212486 ) ) ;
#23614 = CARTESIAN_POINT ( 'NONE',  ( -26.29305231718578995, 52.20000000000000995, 19.10302069950538595 ) ) ;
#23615 = CARTESIAN_POINT ( 'NONE',  ( 7.236395654485755280, 14.22499999726881192, 22.27133577429736988 ) ) ;
#23616 = CARTESIAN_POINT ( 'NONE',  ( -33.58253175000000113, 59.22500000273119980, 10.91162601494193929 ) ) ;
#23617 = CARTESIAN_POINT ( 'NONE',  ( 23.41746825000000243, 9.224999997268820806, -7.608796670333727974 ) ) ;
#23618 = ORIENTED_EDGE ( 'NONE', *, *, #10218, .T. ) ;
#23619 = CARTESIAN_POINT ( 'NONE',  ( 20.75514604977249178, 72.07500000273120122, 28.56700777964553950 ) ) ;
#23620 =( BOUNDED_CURVE ( )  B_SPLINE_CURVE ( 2, ( #27331, #8964, #33139, #22349, #16869, #20125, #19948, #3818, #32796, #4155, #1565, #30224, #7066 ),
 .UNSPECIFIED., .F., .T. ) 
 B_SPLINE_CURVE_WITH_KNOTS ( ( 3, 2, 2, 2, 2, 2, 3 ),
 ( 0.04487179487179487197, 0.04615384615384615641, 0.04871794871794871834, 0.05128205128205128027, 0.05384615384615384914, 0.05641025641025641107, 0.05769230769230769551 ),
 .UNSPECIFIED. ) 
 CURVE ( )  GEOMETRIC_REPRESENTATION_ITEM ( )  RATIONAL_B_SPLINE_CURVE ( ( 0.9755282581475768211, 0.9755282581475768211, 1.000000000000000000, 0.9510565162951535312, 1.000000000000000000, 0.9510565162951535312, 1.000000000000000000, 0.9510565162951535312, 1.000000000000000000, 0.9510565162951535312, 1.000000000000000000, 0.9755282581475767101, 0.9755282581475768211 ) ) 
 REPRESENTATION_ITEM ( '' )  );
#23621 = CARTESIAN_POINT ( 'NONE',  ( -20.75514604977248112, 9.425000002731202642, 28.56700777964554661 ) ) ;
#23622 = CARTESIAN_POINT ( 'NONE',  ( -18.94512977948576093, 16.32499999726880091, 13.76444248337722698 ) ) ;
#23623 = CARTESIAN_POINT ( 'NONE',  ( 19.06425588902592239, 15.15663166759064495, 19.11951029504763611 ) ) ;
#23624 = ADVANCED_FACE ( 'NONE', ( #25145 ), #5067, .F. ) ;
#23625 = VERTEX_POINT ( 'NONE', #12233 ) ;
#23626 = CARTESIAN_POINT ( 'NONE',  ( 20.75514604977249178, 43.82500000273119412, 28.56700777964553950 ) ) ;
#23627 = ORIENTED_EDGE ( 'NONE', *, *, #30730, .T. ) ;
#23628 = CARTESIAN_POINT ( 'NONE',  ( 7.505752307972854531, 40.07291666666666430, -28.01184896238303423 ) ) ;
#23629 = CARTESIAN_POINT ( 'NONE',  ( -26.29305231718578995, 60.70000000546237118, 19.10302069950538595 ) ) ;
#23630 = CARTESIAN_POINT ( 'NONE',  ( -10.04305231718578462, 4.900000005462382013, 30.90933677959249337 ) ) ;
#23631 = CARTESIAN_POINT ( 'NONE',  ( 5.147494310547426899, 27.94874572391553613, -32.50000000000000000 ) ) ;
#23632 = CARTESIAN_POINT ( 'NONE',  ( 28.01184896238290278, 23.45833333333333215, -7.505752307973347470 ) ) ;
#23633 = ADVANCED_FACE ( 'NONE', ( #9144 ), #27348, .F. ) ;
#23634 = CARTESIAN_POINT ( 'NONE',  ( -19.82091636218621034, 0.7999999999999951594, -14.40073868116559552 ) ) ;
#23635 = CARTESIAN_POINT ( 'NONE',  ( 20.75514604977248467, 12.67500000273118488, -28.56700777964554305 ) ) ;
#23636 = CARTESIAN_POINT ( 'NONE',  ( -32.50000000000000000, 60.00000000000000000, 0.000000000000000000 ) ) ;
#23637 = CARTESIAN_POINT ( 'NONE',  ( 13.91746824999999532, 75.97500000273119269, -4.522059556121118540 ) ) ;
#23638 = DIRECTION ( 'NONE',  ( -0.000000000000000000, -1.000000000000000000, -0.000000000000000000 ) ) ;
#23639 = AXIS2_PLACEMENT_3D ( 'NONE', #33766, #17989, #5272 ) ;
#23640 = CARTESIAN_POINT ( 'NONE',  ( -28.00173670424535644, 34.05170166574267654, 7.543491769121936308 ) ) ;
#23641 = CARTESIAN_POINT ( 'NONE',  ( -4.300734207923759378, 74.97500000273119269, -13.23629886949340495 ) ) ;
#23642 = CARTESIAN_POINT ( 'NONE',  ( -7.505752307973343918, 39.78645833333332860, -28.01184896238290989 ) ) ;
#23643 = APPLICATION_PROTOCOL_DEFINITION ( 'draft international standard', 'automotive_design', 1998, #5706 ) ;
#23644 = EDGE_CURVE ( 'NONE', #23797, #9681, #4174, .T. ) ;
#23645 = CYLINDRICAL_SURFACE ( 'NONE', #22304, 15.00000000000000000 ) ;
#23646 = CARTESIAN_POINT ( 'NONE',  ( -3.880418787951136483, 12.55125428154685174, -24.50000000000000000 ) ) ;
#23647 = CARTESIAN_POINT ( 'NONE',  ( 20.08610463437158344, 4.699999999999995737, 27.64615127144129403 ) ) ;
#23648 = CARTESIAN_POINT ( 'NONE',  ( -33.58253175000000113, 79.12500000273119838, 0.000000000000000000 ) ) ;
#23649 = CARTESIAN_POINT ( 'NONE',  ( 24.22776226481265383, 63.70013916574268364, 13.94119854578893580 ) ) ;
#23650 = CARTESIAN_POINT ( 'NONE',  ( 33.58253175000000823, 48.02500000273119696, 10.91162601494192863 ) ) ;
#23651 = CARTESIAN_POINT ( 'NONE',  ( 20.75514604977248467, 52.67500000273116711, -28.56700777964554305 ) ) ;
#23652 = CARTESIAN_POINT ( 'NONE',  ( -33.58253175000000113, 35.47500000273119269, 10.91162601494193929 ) ) ;
#23653 = CARTESIAN_POINT ( 'NONE',  ( 10.04305231718578817, 25.40000000000000568, -30.90933677959249337 ) ) ;
#23654 = DIRECTION ( 'NONE',  ( -0.8660254037844410391, 0.4999999999999958367, 0.000000000000000000 ) ) ;
#23655 = LINE ( 'NONE', #26394, #10861 ) ;
#23656 = CIRCLE ( 'NONE', #28025, 3.500000000000010214 ) ;
#23657 = CARTESIAN_POINT ( 'NONE',  ( -1.778240108872766143E-15, 52.00000000546237544, -32.49999999999999289 ) ) ;
#23658 = CARTESIAN_POINT ( 'NONE',  ( -2.092463501923844636E-15, 77.50000000000000000, -34.17252228774368916 ) ) ;
#23659 = CARTESIAN_POINT ( 'NONE',  ( -33.58253175000000113, 17.12500000273119127, 0.000000000000000000 ) ) ;
#23660 = DIRECTION ( 'NONE',  ( 1.224646799147353454E-16, -1.000000000000000000, 0.000000000000000000 ) ) ;
#23661 = DIRECTION ( 'NONE',  ( -0.000000000000000000, -1.000000000000000000, -0.000000000000000000 ) ) ;
#23662 = CARTESIAN_POINT ( 'NONE',  ( 19.06425588902558133, 18.29649333240935150, -19.11951029504797006 ) ) ;
#23663 = CARTESIAN_POINT ( 'NONE',  ( 26.29305231718578995, 33.70000000546237118, -19.10302069950538240 ) ) ;
#23664 = CARTESIAN_POINT ( 'NONE',  ( -4.223320258572819786E-15, 11.24999999453763344, 24.50000000000000000 ) ) ;
#23665 = CARTESIAN_POINT ( 'NONE',  ( 20.75514604977249178, 27.82500000273116925, 28.56700777964553950 ) ) ;
#23666 = AXIS2_PLACEMENT_3D ( 'NONE', #12866, #33969, #25089 ) ;
#23667 = CARTESIAN_POINT ( 'NONE',  ( 2.584737979205441561E-13, 45.08593750000000711, 27.95245687107222921 ) ) ;
#23668 = ORIENTED_EDGE ( 'NONE', *, *, #27812, .F. ) ;
#23669 = CARTESIAN_POINT ( 'NONE',  ( -2.162160676586881955E-15, 62.62500000273116996, -35.31076352940723240 ) ) ;
#23670 = EDGE_LOOP ( 'NONE', ( #4614, #5929, #20293, #11166 ) ) ;
#23671 = CARTESIAN_POINT ( 'NONE',  ( -20.50609665441004736, 18.87499999999999645, -20.50609665440969565 ) ) ;
#23672 = CARTESIAN_POINT ( 'NONE',  ( -15.04653450569291984, 15.87277750092397710, 25.98046417659859486 ) ) ;
#23673 = CARTESIAN_POINT ( 'NONE',  ( 33.58253175000000113, 4.225000002731190030, -10.91162601494193751 ) ) ;
#23674 = CARTESIAN_POINT ( 'NONE',  ( -7.236395654485757944, 1.224999997268799712, -22.27133577429736988 ) ) ;
#23675 = CARTESIAN_POINT ( 'NONE',  ( 27.16883889988623935, 32.57500000273119412, -19.73931689729374384 ) ) ;
#23676 = CARTESIAN_POINT ( 'NONE',  ( 20.08610463437158344, 39.20000000546237118, 27.64615127144129403 ) ) ;
#23677 = CARTESIAN_POINT ( 'NONE',  ( 26.29305231718578995, 77.19999999999998863, -19.10302069950538240 ) ) ;
#23678 = CARTESIAN_POINT ( 'NONE',  ( 28.01184896238304134, 64.99479166666665719, 7.505752307972846538 ) ) ;
#23679 = CARTESIAN_POINT ( 'NONE',  ( 5.147494310547440222, 77.44874571845315359, -32.50000000000000000 ) ) ;
#23680 = CARTESIAN_POINT ( 'NONE',  ( 20.75514604977248467, 50.67500000273117422, -28.56700777964554305 ) ) ;
#23681 = CARTESIAN_POINT ( 'NONE',  ( 20.08610463437158344, 20.69999999999998508, 27.64615127144129403 ) ) ;
#23682 = CARTESIAN_POINT ( 'NONE',  ( -10.04305231718578462, 20.40000000000000213, 30.90933677959249337 ) ) ;
#23683 = CARTESIAN_POINT ( 'NONE',  ( 19.82091636218621389, 8.200000000000013500, -14.40073868116559197 ) ) ;
#23684 = EDGE_CURVE ( 'NONE', #13542, #18703, #22707, .T. ) ;
#23685 = CARTESIAN_POINT ( 'NONE',  ( 33.58253175000000113, 72.22500000273119269, -10.91162601494193751 ) ) ;
#23686 = CARTESIAN_POINT ( 'NONE',  ( -10.04305231718578462, 78.39999999999999147, 30.90933677959249337 ) ) ;
#23687 = CARTESIAN_POINT ( 'NONE',  ( 10.89113995073883068, 73.99999999999998579, -8.941408771340327633 ) ) ;
#23688 = CARTESIAN_POINT ( 'NONE',  ( 10.37757302488624056, 56.77500000273119696, -31.93888565452638417 ) ) ;
#23689 = CARTESIAN_POINT ( 'NONE',  ( 10.04305231718578817, 39.90000000546237402, -30.90933677959249337 ) ) ;
#23690 = CARTESIAN_POINT ( 'NONE',  ( 20.75514604977249178, 13.82500000273117813, 28.56700777964553950 ) ) ;
#23691 = CARTESIAN_POINT ( 'NONE',  ( -6.950374756619716266, 30.91184000092396644, -26.09010956794232428 ) ) ;
#23692 = CARTESIAN_POINT ( 'NONE',  ( 15.14183272437242067, 9.449999994537636283, 20.84094480462498211 ) ) ;
#23693 = CARTESIAN_POINT ( 'NONE',  ( -2.162160676586882350E-15, 2.875000002731204596, -35.31076352940722529 ) ) ;
#23694 = CARTESIAN_POINT ( 'NONE',  ( 6.486482029760649416E-15, 33.62500000273119127, 35.31076352940723240 ) ) ;
#23695 = CYLINDRICAL_SURFACE ( 'NONE', #16068, 32.50000000000000000 ) ;
#23696 = FACE_OUTER_BOUND ( 'NONE', #22528, .T. ) ;
#23697 = CARTESIAN_POINT ( 'NONE',  ( -8.601468415847518756, 76.57500000273120122, -11.83890561707634603 ) ) ;
#23698 = CARTESIAN_POINT ( 'NONE',  ( 26.02091320914876960, 43.07513916574269786, 14.97647472619900455 ) ) ;
#23699 = CARTESIAN_POINT ( 'NONE',  ( 26.29305231718579350, 55.30000000546237970, 19.10302069950537529 ) ) ;
#23700 = CARTESIAN_POINT ( 'NONE',  ( -8.601468415847518756, 75.07500000273118701, -11.83890561707634781 ) ) ;
#23701 = CARTESIAN_POINT ( 'NONE',  ( 5.779280353836490358E-15, 60.49999999999998579, 32.49999999999999289 ) ) ;
#23702 = CARTESIAN_POINT ( 'NONE',  ( -19.09188309203694445, 15.43749999999999645, -19.09188309203661049 ) ) ;
#23703 = CARTESIAN_POINT ( 'NONE',  ( 18.94512977948576093, 7.324999997268822227, -13.76444248337722875 ) ) ;
#23704 = CARTESIAN_POINT ( 'NONE',  ( 10.04305231718579705, 71.10000000546237686, 30.90933677959248982 ) ) ;
#23705 = CARTESIAN_POINT ( 'NONE',  ( -20.50609665440969209, 18.01562499999999645, 20.50609665441005092 ) ) ;
#23706 = CARTESIAN_POINT ( 'NONE',  ( 27.16883889988623935, 26.57500000273120477, -19.73931689729374384 ) ) ;
#23707 = CARTESIAN_POINT ( 'NONE',  ( 14.47279130897151944, 13.42499999726880411, -19.92008829642072598 ) ) ;
#23708 = ORIENTED_EDGE ( 'NONE', *, *, #20503, .F. ) ;
#23709 = CARTESIAN_POINT ( 'NONE',  ( 25.98046417659858420, 39.07590250092398065, 15.04653450569292872 ) ) ;
#23710 = CARTESIAN_POINT ( 'NONE',  ( 32.50000000000000000, 15.50000000546238077, -3.980102097228898626E-15 ) ) ;
#23711 = CARTESIAN_POINT ( 'NONE',  ( -28.01184896238290278, 49.23958333333332860, 7.505752307973363457 ) ) ;
#23712 = DIRECTION ( 'NONE',  ( 0.000000000000000000, 0.000000000000000000, -1.000000000000000000 ) ) ;
#23713 = CARTESIAN_POINT ( 'NONE',  ( 10.37757302488624056, 56.77500000273119696, -31.93888565452638417 ) ) ;
#23714 = CARTESIAN_POINT ( 'NONE',  ( 20.08610463437157279, 53.80000000546237970, -27.64615127144129758 ) ) ;
#23715 =( BOUNDED_CURVE ( )  B_SPLINE_CURVE ( 2, ( #25882, #2375, #21094, #5121, #23322, #15605, #13184, #2553, #28966, #24651, #22091, #13864, #8866 ),
 .UNSPECIFIED., .F., .T. ) 
 B_SPLINE_CURVE_WITH_KNOTS ( ( 3, 2, 2, 2, 2, 2, 3 ),
 ( 0.6388888888888889506, 0.6444444444444444864, 0.6555555555555555580, 0.6666666666666666297, 0.6777777777777778123, 0.6888888888888888840, 0.6944444444444444198 ),
 .UNSPECIFIED. ) 
 CURVE ( )  GEOMETRIC_REPRESENTATION_ITEM ( )  RATIONAL_B_SPLINE_CURVE ( ( 0.9755282581475768211, 0.9755282581475770431, 1.000000000000000000, 0.9510565162951535312, 1.000000000000000000, 0.9510565162951535312, 1.000000000000000000, 0.9510565162951535312, 1.000000000000000000, 0.9510565162951535312, 1.000000000000000000, 0.9755282581475768211, 0.9755282581475768211 ) ) 
 REPRESENTATION_ITEM ( '' )  );
#23716 = CARTESIAN_POINT ( 'NONE',  ( -4.300734207923759378, 76.97500000273122112, -13.23629886949340495 ) ) ;
#23717 = CARTESIAN_POINT ( 'NONE',  ( -33.58253175000000113, 41.22500000273118559, 10.91162601494193929 ) ) ;
#23718 = CARTESIAN_POINT ( 'NONE',  ( 5.779280353836490358E-15, 39.00000000546237544, 32.49999999999999289 ) ) ;
#23719 = CARTESIAN_POINT ( 'NONE',  ( -27.16883889988624290, 69.17500000273119554, -19.73931689729374028 ) ) ;
#23720 = CARTESIAN_POINT ( 'NONE',  ( 13.56056531762472872, 73.99999999999997158, 3.164391494949048145 ) ) ;
#23721 = CARTESIAN_POINT ( 'NONE',  ( -2.162160676586882350E-15, 60.62500000273118417, -35.31076352940722529 ) ) ;
#23722 = CARTESIAN_POINT ( 'NONE',  ( -15.01150461594642316, 19.01822916666666430, -26.00068869287341045 ) ) ;
#23723 = CARTESIAN_POINT ( 'NONE',  ( 32.50000000000000711, 48.89999999999999858, 10.55989012756945122 ) ) ;
#23724 = CARTESIAN_POINT ( 'NONE',  ( 14.47279130897151767, 4.924999997268811214, -19.92008829642072598 ) ) ;
#23725 = EDGE_CURVE ( 'NONE', #14241, #11374, #16493, .T. ) ;
#23726 = CARTESIAN_POINT ( 'NONE',  ( 20.75514604977249178, 8.075000002731185234, 28.56700777964553950 ) ) ;
#23727 = CARTESIAN_POINT ( 'NONE',  ( 10.04305231718578817, 35.90000000546239534, -30.90933677959249337 ) ) ;
#23728 = CARTESIAN_POINT ( 'NONE',  ( 19.11951029504797006, 36.34336833240934794, 19.06425588902558133 ) ) ;
#23729 = CARTESIAN_POINT ( 'NONE',  ( -4.300734207923755825, 71.77500000273117564, 13.23629886949340673 ) ) ;
#23730 = CARTESIAN_POINT ( 'NONE',  ( 10.37757302488624767, 77.97500000273119269, 31.93888565452638417 ) ) ;
#23731 = LINE ( 'NONE', #21165, #5079 ) ;
#23732 = EDGE_CURVE ( 'NONE', #25120, #19608, #12060, .T. ) ;
#23733 = VECTOR ( 'NONE', #32634, 1000.000000000000000 ) ;
#23734 = CARTESIAN_POINT ( 'NONE',  ( 27.16883889988624290, 74.17500000273118133, 19.73931689729373673 ) ) ;
#23735 = ORIENTED_EDGE ( 'NONE', *, *, #9203, .T. ) ;
#23736 = LINE ( 'NONE', #18427, #21726 ) ;
#23737 = CARTESIAN_POINT ( 'NONE',  ( 26.07999730980490227, 58.11979166666665719, 6.988114217767821046 ) ) ;
#23738 = CARTESIAN_POINT ( 'NONE',  ( -10.37757302488623701, 53.52500000273118275, 31.93888565452638417 ) ) ;
#23739 = CARTESIAN_POINT ( 'NONE',  ( 33.58253175000000113, 18.47500000273117848, -10.91162601494193751 ) ) ;
#23740 = CARTESIAN_POINT ( 'NONE',  ( -10.37757302488623701, 3.775000002731190740, 31.93888565452638417 ) ) ;
#23741 = CARTESIAN_POINT ( 'NONE',  ( 26.07999730980477437, 37.20833333333332860, -6.988114217768290004 ) ) ;
#23742 = CARTESIAN_POINT ( 'NONE',  ( -25.98046417659859486, 33.91965250092398065, -15.04653450569291628 ) ) ;
#23743 = CARTESIAN_POINT ( 'NONE',  ( 25.98046417659831775, 15.00222249907602112, -15.04653450569338879 ) ) ;
#23744 = CARTESIAN_POINT ( 'NONE',  ( -10.04305231718578462, 70.90000000546238823, 30.90933677959249337 ) ) ;
#23745 = CARTESIAN_POINT ( 'NONE',  ( 32.79451539931730508, 52.00000000000002842, -5.771861194046441490 ) ) ;
#23746 = CARTESIAN_POINT ( 'NONE',  ( 27.16883889988624290, 41.92500000273119554, 19.73931689729373673 ) ) ;
#23747 = CARTESIAN_POINT ( 'NONE',  ( -13.94119854578892514, 50.80951416574269075, 24.22776226481266448 ) ) ;
#23748 = CARTESIAN_POINT ( 'NONE',  ( -14.47279130897152122, 11.92499999726882010, 19.92008829642072243 ) ) ;
#23749 = FACE_OUTER_BOUND ( 'NONE', #2940, .T. ) ;
#23750 = VERTEX_POINT ( 'NONE', #22880 ) ;
#23751 = CARTESIAN_POINT ( 'NONE',  ( -10.37757302488624411, 46.97500000273117848, -31.93888565452638417 ) ) ;
#23752 = CARTESIAN_POINT ( 'NONE',  ( 12.13525491562420910, 77.19999999999998863, -8.816778784387098611 ) ) ;
#23753 = CARTESIAN_POINT ( 'NONE',  ( -26.06988505166735237, 44.08892333425729504, -7.025853678916388567 ) ) ;
#23754 = CARTESIAN_POINT ( 'NONE',  ( 20.75514604977248467, 68.67500000273119554, -28.56700777964554305 ) ) ;
#23755 = ORIENTED_EDGE ( 'NONE', *, *, #5517, .T. ) ;
#23756 = CARTESIAN_POINT ( 'NONE',  ( -33.58253175000000113, 23.02500000273117919, -10.91162601494193218 ) ) ;
#23757 = AXIS2_PLACEMENT_3D ( 'NONE', #20730, #25853, #17978 ) ;
#23758 = CARTESIAN_POINT ( 'NONE',  ( -2.584737979205441561E-13, 22.74218749999999645, -30.02300923189239512 ) ) ;
#23759 = EDGE_LOOP ( 'NONE', ( #1430, #16736, #3402, #25041 ) ) ;
#23760 = CARTESIAN_POINT ( 'NONE',  ( -20.08610463437157989, 14.20000000546237473, -27.64615127144129758 ) ) ;
#23761 = CARTESIAN_POINT ( 'NONE',  ( 33.58253175000000113, 64.12500000273119838, -4.112674001490185761E-15 ) ) ;
#23762 = CARTESIAN_POINT ( 'NONE',  ( 15.01150461594643204, 44.79947916666667140, 26.00068869287340334 ) ) ;
#23763 = DIRECTION ( 'NONE',  ( 0.000000000000000000, 0.000000000000000000, -1.000000000000000000 ) ) ;
#23764 = CARTESIAN_POINT ( 'NONE',  ( 18.94512977948576093, 7.324999997268822227, -13.76444248337722875 ) ) ;
#23765 = CARTESIAN_POINT ( 'NONE',  ( 10.37757302488624056, 4.525000002731205839, -31.93888565452638417 ) ) ;
#23766 = CARTESIAN_POINT ( 'NONE',  ( 27.16883889988623935, 28.57500000273119412, -19.73931689729374384 ) ) ;
#23767 = CARTESIAN_POINT ( 'NONE',  ( 26.29305231718578995, 5.700000005462390718, -19.10302069950538240 ) ) ;
#23768 = CARTESIAN_POINT ( 'NONE',  ( -14.97647472619899389, 61.12201416574268364, 26.02091320914878025 ) ) ;
#23769 = CARTESIAN_POINT ( 'NONE',  ( -3.880418787951104953, 15.44874571845315359, 24.50000000000000711 ) ) ;
#23770 = CARTESIAN_POINT ( 'NONE',  ( -20.08610463437156923, 32.29999999999999716, 27.64615127144130113 ) ) ;
#23771 = CARTESIAN_POINT ( 'NONE',  ( -1.778240108872766143E-15, 3.500000000000004441, -32.49999999999999289 ) ) ;
#23772 = CARTESIAN_POINT ( 'NONE',  ( 10.04305231718578817, 19.40000000000001279, -30.90933677959249337 ) ) ;
#23773 = CARTESIAN_POINT ( 'NONE',  ( -27.95245687107223276, 56.25781249999999289, 2.498001805406602216E-13 ) ) ;
#23774 = ADVANCED_FACE ( 'NONE', ( #16885 ), #4512, .T. ) ;
#23775 = ADVANCED_FACE ( 'NONE', ( #11895 ), #32650, .F. ) ;
#23776 = CARTESIAN_POINT ( 'NONE',  ( -7.236395654485763274, 2.524999997268823293, 22.27133577429736633 ) ) ;
#23777 = CARTESIAN_POINT ( 'NONE',  ( 4.635254915624212657, 70.85000000546237686, 14.26584774442730286 ) ) ;
#23778 = CARTESIAN_POINT ( 'NONE',  ( 6.988114217768294445, 27.75520833333332860, 26.07999730980477437 ) ) ;
#23779 = CARTESIAN_POINT ( 'NONE',  ( 27.16883889988624290, 21.92500000273117777, 19.73931689729373673 ) ) ;
#23780 = CARTESIAN_POINT ( 'NONE',  ( 20.75514604977249178, 75.82500000273118701, 28.56700777964553950 ) ) ;
#23781 = CARTESIAN_POINT ( 'NONE',  ( 20.75514604977249178, 36.07500000273117990, 28.56700777964553950 ) ) ;
#23782 = CARTESIAN_POINT ( 'NONE',  ( 27.16883889988623935, 12.57500000273120655, -19.73931689729374384 ) ) ;
#23783 = CARTESIAN_POINT ( 'NONE',  ( -5.147494310547478413, 64.44874571845315359, 32.49999999999998579 ) ) ;
#23784 = CARTESIAN_POINT ( 'NONE',  ( -24.22776226481240514, 60.84673583425731636, 13.94119854578937812 ) ) ;
#23785 = CARTESIAN_POINT ( 'NONE',  ( 20.75514604977249178, 71.82500000273117280, 28.56700777964553950 ) ) ;
#23786 = LINE ( 'NONE', #31660, #14309 ) ;
#23787 = CARTESIAN_POINT ( 'NONE',  ( 10.04305231718579705, 56.59999999999999432, 30.90933677959248982 ) ) ;
#23788 = CARTESIAN_POINT ( 'NONE',  ( 15.00000000000000000, 79.25000000546239676, -1.836970198721029589E-15 ) ) ;
#23789 = CARTESIAN_POINT ( 'NONE',  ( 33.58253175000000113, 60.22500000273119980, -10.91162601494193574 ) ) ;
#23790 = EDGE_CURVE ( 'NONE', #16901, #7704, #19968, .T. ) ;
#23791 = CARTESIAN_POINT ( 'NONE',  ( -4.523095164977116484E-15, 10.62499999726880695, 24.62258325217400312 ) ) ;
#23792 = ORIENTED_EDGE ( 'NONE', *, *, #25422, .T. ) ;
#23793 = CARTESIAN_POINT ( 'NONE',  ( -2.162160676586881955E-15, 74.87500000273116996, -35.31076352940723240 ) ) ;
#23794 = DIRECTION ( 'NONE',  ( -1.224646799147353454E-16, 1.000000000000000000, -0.000000000000000000 ) ) ;
#23795 = CARTESIAN_POINT ( 'NONE',  ( -18.94512977948576093, 1.824999997268816898, 13.76444248337722698 ) ) ;
#23796 = CARTESIAN_POINT ( 'NONE',  ( 24.18731323226247554, 11.57590250092397355, 14.01125832528285997 ) ) ;
#23797 = VERTEX_POINT ( 'NONE', #4002 ) ;
#23798 = CARTESIAN_POINT ( 'NONE',  ( 33.58253175000000823, 44.02500000273118275, 10.91162601494192863 ) ) ;
#23799 = DIRECTION ( 'NONE',  ( -1.000000000000000000, 0.000000000000000000, 0.000000000000000000 ) ) ;
#23800 = VERTEX_POINT ( 'NONE', #32813 ) ;
#23801 = CARTESIAN_POINT ( 'NONE',  ( 15.01150461594596308, 47.09114583333332860, -26.00068869287367335 ) ) ;
#23802 = CARTESIAN_POINT ( 'NONE',  ( -1.778240108872766143E-15, 5.500000000000003553, -32.49999999999999289 ) ) ;
#23803 = CARTESIAN_POINT ( 'NONE',  ( -26.29305231718579350, 4.300000005462378816, -19.10302069950537884 ) ) ;
#23804 = CARTESIAN_POINT ( 'NONE',  ( 3.000384657911015469E-15, 0.000000000000000000, -24.50000000000000000 ) ) ;
#23805 = AXIS2_PLACEMENT_3D ( 'NONE', #28960, #13177, #18004 ) ;
#23806 = CARTESIAN_POINT ( 'NONE',  ( -7.505752307972844761, 24.60416666666666430, 28.01184896238304134 ) ) ;
#23807 = CARTESIAN_POINT ( 'NONE',  ( 15.14183272437242245, 0.2999999999999904965, -20.84094480462497856 ) ) ;
#23808 = CARTESIAN_POINT ( 'NONE',  ( 10.37757302488624767, 11.97500000273118914, 31.93888565452638417 ) ) ;
#23809 = CARTESIAN_POINT ( 'NONE',  ( -26.29305231718579350, 57.80000000000001847, -19.10302069950537884 ) ) ;
#23810 = CARTESIAN_POINT ( 'NONE',  ( -4.300734207923755825, 77.27500000273118985, 13.23629886949340673 ) ) ;
#23811 = CARTESIAN_POINT ( 'NONE',  ( 26.29305231718579350, 73.30000000546237970, 19.10302069950537529 ) ) ;
#23812 = CARTESIAN_POINT ( 'NONE',  ( 28.00173670424535644, 32.33295166574267654, -7.543491769121920321 ) ) ;
#23813 = CARTESIAN_POINT ( 'NONE',  ( 13.91746824999999532, 76.47500000273117848, -4.522059556121118540 ) ) ;
#23814 = CARTESIAN_POINT ( 'NONE',  ( -26.00068869287368756, 53.10677083333332149, -15.01150461594595775 ) ) ;
#23815 = CARTESIAN_POINT ( 'NONE',  ( -1.778240108872766143E-15, 34.00000000546236834, -32.49999999999999289 ) ) ;
#23816 = CARTESIAN_POINT ( 'NONE',  ( 26.29305231718579350, 64.79999999999999716, 19.10302069950537529 ) ) ;
#23817 = CARTESIAN_POINT ( 'NONE',  ( 10.04305231718579705, 2.599999999999991207, 30.90933677959248982 ) ) ;
#23818 = CARTESIAN_POINT ( 'NONE',  ( 8.151180760100182884E-15, -89.55944200217849982, 0.000000000000000000 ) ) ;
#23819 = CARTESIAN_POINT ( 'NONE',  ( -14.01125832528328985, 58.83034749907602645, -24.18731323226223040 ) ) ;
#23820 = CARTESIAN_POINT ( 'NONE',  ( -33.58253175000000113, 47.12500000273117706, 0.000000000000000000 ) ) ;
#23821 = CARTESIAN_POINT ( 'NONE',  ( -13.91746824999999887, 80.87500000273118417, 0.000000000000000000 ) ) ;
#23822 = CARTESIAN_POINT ( 'NONE',  ( 10.37757302488624056, 58.77500000273121117, -31.93888565452638417 ) ) ;
#23823 = CARTESIAN_POINT ( 'NONE',  ( -2.162160676586882350E-15, 36.87500000273117706, -35.31076352940722529 ) ) ;
#23824 =( BOUNDED_CURVE ( )  B_SPLINE_CURVE ( 2, ( #25711, #4941, #5288, #15423, #28616, #15770, #20913, #26225, #20579, #2547, #33601, #10780, #31702 ),
 .UNSPECIFIED., .F., .T. ) 
 B_SPLINE_CURVE_WITH_KNOTS ( ( 3, 2, 2, 2, 2, 2, 3 ),
 ( 0.2243589743589743668, 0.2256410256410256443, 0.2282051282051281993, 0.2307692307692307820, 0.2333333333333333370, 0.2358974358974358920, 0.2371794871794871973 ),
 .UNSPECIFIED. ) 
 CURVE ( )  GEOMETRIC_REPRESENTATION_ITEM ( )  RATIONAL_B_SPLINE_CURVE ( ( 0.9755282581475768211, 0.9755282581475768211, 1.000000000000000000, 0.9510565162951535312, 1.000000000000000000, 0.9510565162951535312, 1.000000000000000000, 0.9510565162951535312, 1.000000000000000000, 0.9510565162951535312, 1.000000000000000000, 0.9755282581475764880, 0.9755282581475768211 ) ) 
 REPRESENTATION_ITEM ( '' )  );
#23825 = CARTESIAN_POINT ( 'NONE',  ( 23.41746824999999887, 18.62499999726882649, 0.000000000000000000 ) ) ;
#23826 = CARTESIAN_POINT ( 'NONE',  ( -26.07999730980490583, 25.46354166666666430, -6.988114217767815717 ) ) ;
#23827 = CARTESIAN_POINT ( 'NONE',  ( 32.50000000000000000, 15.60000000546238930, -10.55989012756945833 ) ) ;
#23828 =( GEOMETRIC_REPRESENTATION_CONTEXT ( 3 ) GLOBAL_UNCERTAINTY_ASSIGNED_CONTEXT ( ( #15343 ) ) GLOBAL_UNIT_ASSIGNED_CONTEXT ( ( #13718, #1150, #8720 ) ) REPRESENTATION_CONTEXT ( 'NONE', 'WORKASPACE' ) );
#23829 =( BOUNDED_SURFACE ( )  B_SPLINE_SURFACE ( 1, 2, ( 
 ( #9529, #25498, #12276, #27900, #7295, #7643, #22749, #1978, #12453, #4382, #25668, #18128, #2147, #28572, #12622, #23089, #33553, #10053, #33200, #20534, #5069, #30978, #17959, #26006, #9703, #25833, #2323, #2499, #20010, #29246, #247, #582, #31319, #23780, #26685, #31986, #8483, #18468, #23607, #23948, #16231, #15891, #13812, #7811, #18970, #21376, #13483, #29415, #13650, #24115, #5243, #21538, #5581, #10732, #13305, #33902, #8151, #18300, #29077, #5916, #3011, #21041, #31821, #8311, #16062, #28911, #21209, #5412, #26517, #31654, #18802, #18640, #2836, #15725, #5750, #26180, #2675, #417, #10393, #10562, #3181, #11072, #74, #16393, #3343, #10904, #26846, #20872, #28745, #13133, #7981, #31491, #26347, #29739, #6071, #11233, #24602, #1419, #16555, #915, #19295, #21709, #14146, #4004, #6243, #32815, #21871, #32321, #22038, #11394, #27008, #27351, #9308, #14311, #16888, #19793, #3505, #16724, #27179, #1244, #17226, #19629, #1076, #24934, #32155, #11556, #17055, #22369, #30241, #8812, #13975, #24766, #6580, #3672, #4176, #8648, #6746, #11722, #3836, #27686, #14477, #11897, #29570, #24280, #29914, #32482, #8983, #748, #19465, #6416, #9147, #27517, #30074, #22205, #19133, #24438, #32652, #17920, #1586, #14989, #25283, #28371, #20145, #19970, #1934, #25794, #12412, #12062, #30589, #4859, #33339, #12583, #4514, #22533, #33161, #32983, #31111, #20672, #2283, #6915, #23053, #30416, #7605, #10017, #9664, #25110, #22882, #9487, #17740, #33512, #1755, #20314, #20488, #9836, #15339, #30763, #17397, #27861, #28200, #4343, #14650, #7085, #14818, #7253, #4686, #18085, #25631, #12758, #15165, #12235, #2110, #22711, #17569, #30939, #28027, #7434, #25459, #23230, #33690, #10189, #28533, #2459, #31778, #2633, #31613, #23402, #13096, #21171, #31946, #2796, #23569, #7942, #15514, #8439, #10523, #18762, #8110, #29206, #20834, #377, #15687, #18930, #5540, #18259, #13263, #10863, #16021, #34, #15851, #25965, #29037, #21000, #26136, #21337, #31449, #10356, #23738, #31279, #18429, #12925, #26476, #7772, #28874, #8270, #5028, #5370, #541, #26307, #202, #28705, #24076, #10690, #5712, #18597, #2969, #16190, #13439, #33863, #23906, #5203, #26644, #3138, #13611, #11029, #21498, #3965, #27308, #24563, #3799, #876, #16513, #1036, #6373, #3466, #1203, #6543, #19590, #1379, #21834, #3632, #8772, #9271, #27476, #14271, #32279, #17016, #11684, #14438, #11516, #19423, #21996, #27138, #709, #24893, #21666, #24728, #11195, #11853, #22168, #13936, #26808, #32444, #22332, #8945, #26965, #16851, #32612, #29873, #24400, #6201, #11356, #9109, #19255, #30038, #14106, #29696, #32112, #32777, #8610, #19093, #29376, #5875, #6034, #16353, #3303, #29531, #13768, #24238, #16681, #22837, #23014, #25415, #30895, #27818, #9969, #23184, #25241, #1546, #6706, #20102, #7389, #12022, #30373, #14776, #17188, #9621, #33469, #1716, #28326, #17354, #4301, #17526, #6874, #22491, #33297, #4814, #9797, #12369, #15293, #32942, #12195, #22666, #30720, #12712, #15124, #30548, #20445, #27646, #7044, #12543, #17874, #25753, #33118, #9443, #20273, #2067, #27987, #33646, #4134, #2237, #7215, #17698, #19755, #30204, #14609, #25065, #19927, #1893, #4474, #14949, #28158, #4644, #25587, #28998, #13397, #15977, #23527, #23867, #5498, #7562, #334, #31067, #10480, #20793, #10820, #15643, #15468, #31407, #21300, #7900, #18046, #26094, #31740, #28831, #8068, #33987, #28490, #28663, #4987, #26603, #16150, #25922, #20626, #18385, #2416, #13218, #18553, #31237, #15810, #26434, #5329, #8231, #26265, #12883, #23359, #23694, #33820, #10143, #5158, #10314, #2753, #160, #3101, #21127, #18725, #10650, #7730, #31570, #18219, #2591, #2926, #13054, #29161, #20958, #5668, #13571, #24035, #8901, #31904, #27268, #32072, #27099, #18886, #8572, #16644, #27435, #32243, #19054, #3426, #10989, #3926, #5997, #14233, #3591, #24690, #16314, #29834, #11156, #14400, #997, #13730, #8735, #6335, #11481, #29494, #11316, #21460, #24527, #16473, #21627, #16813, #26927, #5836, #19219, #26771, #13898, #8398, #21958, #3261, #24365, #3762, #503, #835, #30000, #21794, #29655, #24198, #19553, #6160, #1164, #14065, #32405, #11646, #19385, #29334, #22129, #668, #32573, #9072, #6505, #16978, #22452, #33429, #22799, #20060, #33254, #30335, #11983, #30505, #1850, #32900, #30676, #2028, #15080, #30854, #17314, #33076, #4262, #4774, #22970, #9750, #27776, #12502, #7174, #9926, #7005, #14907, #17487, #22624, #25548, #6667, #20236, #1507, #24855, #25371, #4093, #9582, #17655, #12329, #9399, #1675, #1336, #28116, #6832, #19882, #4603, #14736, #30163, #27949, #17148, #25197, #11818, #20402, #27602, #12150, #7345, #22294, #4431, #17830, #28287, #32739, #14567, #9232, #19716, #25027, #10276, #12845, #18518, #13017, #23137, #18176, #29127, #15252, #20917, #23489, #18688, #23319, #23831, #13181, #10441, #23659, #20756, #2372, #31367, #26229, #33784, #21092, #26397, #5460, #21260, #7691, #33949, #28620, #25713, #13356, #120, #5118, #2890, #31538, #296, #7858, #5291, #18348, #28792, #20582, #2194, #15773, #10102, #2718, #10612, #31200, #8032, #28964, #15941, #10783, #31705, #12669, #31027, #8197, #7524, #33604, #15602, #18008, #28454, #4944, #15426, #25879, #26057, #2550, #16277, #29619, #26735, #5630, #24488, #11121, #11441, #21589, #14025, #19019, #801, #961, #3062, #32368, #3228, #32204, #23996, #13696, #21761, #32532, #3392, #24161, #8533, #16114, #9032, #32035, #19347, #8698, #631, #16441, #26566, #6122, #29460, #5963, #21918, #26893, #10950, #13862, #21426, #24327, #13533, #16606, #31867, #11283, #8862, #19976, #19181, #1121, #27059, #3552, #8361, #24647, #29789, #6293, #16769, #27228, #3722, #14192, #467, #11606, #18849, #29297, #22088, #5795, #33869, #28034, #5035, #28377, #25637, #4865, #1943, #17575, #2116, #7442, #4521, #2290, #7611, #20678, #2465, #22889, #4692, #9843, #10362, #28539, #15346, #33346, #18092, #12764, #15520, #12589, #20496, #23059, #28206, #1761, #6921, #15172, #25289, #33519, #25800, #14996, #10023, #23237, #30945, #31118, #17926, #17403, #12241, #33697, #22719, #30422, #25466, #27867 ),
 ( #14825, #12419, #10198, #23408, #25972, #20321, #30770, #4349, #33167, #7260, #12932, #9670, #20151, #30595, #7091, #17746, #715, #21343, #40, #18604, #26650, #31785, #208, #20840, #18937, #5718, #13269, #8445, #3145, #31953, #2976, #10869, #13445, #29043, #26143, #31285, #5546, #15693, #23912, #18768, #7948, #26482, #29212, #16027, #21504, #384, #7778, #2639, #8276, #13102, #18265, #5378, #28711, #16196, #13617, #13774, #24082, #548, #11035, #31455, #29382, #18436, #5209, #5882, #26313, #16359, #2802, #26814, #10696, #3310, #24244, #23575, #10529, #28880, #21006, #15857, #23744, #21177, #31619, #8116, #19261, #14112, #21672, #14615, #16687, #24900, #27315, #1386, #26971, #6549, #21840, #25071, #11690, #24406, #8951, #17023, #22174, #8778, #22002, #32120, #1209, #27144, #32285, #27482, #29703, #16519, #19429, #3472, #6207, #8617, #32618, #13942, #1042, #14444, #11201, #24570, #6713, #3638, #29879, #882, #30211, #32450, #11860, #11522, #6379, #22338, #16857, #19099, #3806, #29537, #6040, #14277, #24734, #11364, #9115, #19761, #19596, #30044, #3972, #32783, #9277, #17194, #27652, #4140, #7395, #12718, #25759, #7568, #27993, #9803, #4820, #20451, #32947, #15299, #22497, #1900, #12200, #2244, #7050, #6879, #22845, #23189, #33303, #9450, #17532, #33651, #20279, #33475, #25421, #19932, #20108, #30378, #18051, #28495, #10148, #27824, #9975, #17360, #4992, #30902, #30554, #4306, #30726, #20630, #4650, #22672, #23020, #17880, #17705, #4480, #12375, #14956, #7220, #28164, #28334, #15131, #25594, #14781, #31073, #25246, #1721, #2073, #1552, #33123, #15474, #12028, #9626, #12549, #29339, #5334, #29003, #29167, #31575, #3106, #22468, #16155, #5841, #31413, #7734, #12888, #26270, #13577, #18224, #2596, #20963, #23364, #15815, #5675, #7906, #509, #23532, #10485, #23699, #13059, #28670, #5504, #10994, #15984, #18559, #21467, #5163, #18390, #28836, #2932, #18892, #21305, #2758, #26608, #33825, #13224, #18730, #24040, #31909, #165, #15648, #26440, #8236, #10655, #25927, #10319, #8404, #13402, #23872, #2421, #20798, #31242, #26099, #21133, #8073, #340, #10825, #31745, #24531, #26933, #1172, #19558, #22135, #29662, #3266, #16650, #3431, #30005, #21798, #21632, #3596, #27440, #14070, #13735, #32249, #6510, #1002, #14238, #6166, #24204, #840, #673, #32744, #22299, #3932, #8576, #24695, #32078, #9237, #11651, #11322, #11162, #11486, #14407, #19391, #13904, #3767, #32578, #32411, #8741, #27104, #19225, #21963, #8906, #9077, #29838, #6340, #19059, #16983, #29499, #6003, #16818, #16319, #24370, #24861, #1341, #16477, #11822, #19721, #27273, #30168, #26777, #12334, #17835, #14741, #30858, #10108, #12155, #22456, #27611, #7009, #28291, #32905, #17319, #1680, #4098, #30510, #20407, #22629, #15257, #4267, #25202, #4436, #27781, #9405, #9755, #25719, #30681, #33261, #2199, #19887, #33083, #9586, #17660, #33608, #2033, #17492, #7351, #14572, #27954, #33434, #4779, #12674, #20066, #30341, #7179, #22975, #14912, #20587, #25032, #23143, #28121, #20241, #6672, #17153, #1512, #11987, #6839, #22804, #25376, #1857, #4608, #15085, #25553, #12508, #9931, #21096, #2555, #18522, #10617, #28459, #28968, #13022, #26401, #25884, #20761, #28625, #18012, #23494, #5464, #5123, #13361, #31205, #7696, #10446, #18182, #12850, #5296, #23835, #26234, #28798, #300, #2378, #15608, #26062, #13186, #21265, #31541, #33953, #15945, #4950, #20923, #2894, #10787, #31709, #31372, #33789, #2723, #8036, #7863, #8201, #15431, #31032, #126, #23663, #7529, #23324, #10281, #18354, #15778, #24910, #1050, #17202, #1731, #22182, #1396, #11530, #25256, #17031, #6890, #1218, #3814, #9460, #3980, #14122, #9123, #20120, #6217, #11870, #14453, #9637, #14286, #14792, #4150, #22345, #14623, #11698, #27326, #32792, #27661, #24743, #12036, #17371, #30388, #12211, #32627, #9285, #19605, #16698, #4317, #25079, #30052, #27834, #22506, #22683, #19769, #30220, #6720, #1560, #22013, #27154, #32958, #32458, #19942, #33134, #6556, #3646, #24579, #8958, #19439, #29887, #6388, #16865, #27491, #25433, #30564, #15142, #7061, #2256, #4831, #23545, #7582, #33836, #25770, #7230, #20642, #17716, #17543, #15485, #2085, #12387, #4662, #28003, #18060, #22856, #4490, #15311, #1910, #28505, #26110, #12560, #12730, #33314, #15660, #7407, #31253, #25606, #28175, #10333, #28346, #14966, #33488, #10496, #9813, #23200, #33663, #7, #23031, #5177, #5002, #10160, #25939, #9989, #20462, #31085, #2432, #30913, #12900, #7745, #20809, #2608, #17893, #23375, #18234, #20290, #28680, #13069, #30737, #8585, #3276, #32089, #3115, #11005, #13587, #18739, #26281, #31424, #29181, #15827, #24049, #18903, #8086, #26619, #29350, #5686, #21643, #16164, #7917, #2772, #518, #13236, #20974, #5514, #18401, #21475, #31922, #13913, #8414, #24214, #5850, #31586, #16329, #18573, #28847, #26785, #26451, #13744, #2942, #686, #352, #11172, #19069, #5346, #29509, #29014, #6013, #23710, #15995, #16487, #24380, #26943, #13413, #23881, #176, #853, #10835, #3443, #10666, #21145, #21314, #31755, #8246, #25687, #11832, #24540, #9087, #17166, #22309, #8917, #22143, #21808, #1352, #27284, #21973, #6682, #29850, #16659, #19568, #32755, #27451, #6350, #32588, #16828, #6521, #24704, #19734, #30017, #14247, #27116, #9248, #3609, #14081, #16992, #11332, #32421, #30179, #4110, #1011, #27623, #15224, #1181, #14417, #14583, #3942, #22469, #19400, #1525, #32257, #3776, #11494, #8750, #11662, #32918, #24870, #25043, #11999, #19234, #9417, #19902, #30825, #7318, #17803, #28261, #4745, #29671, #6177, #5264, #10756, #26201, #28768, #21234, #17979, #18150, #5091, #13155, #29099, #31513, #2522, #2860, #33575, #26030, #28935, #269, #31677, #20731, #25854, #2695, #18492, #28593, #16086, #10073, #8170, #23630, #15746, #18661, #15915, #26371, #7498, #23803, #97, #15576, #8007, #31341, #10414, #12817, #21063, #5434, #13330, #12991, #5604, #2167, #20554, #12641, #23111, #23462, #23290, #31000, #7663, #28429, #33924, #4919, #20892, #15399, #7833, #2345, #18322, #10586, #33758, #10250, #31171, #23970, #9008, #32507, #14169, #18826, #24463, #31843 ) ),
 .UNSPECIFIED., .F., .F., .T. ) 
 B_SPLINE_SURFACE_WITH_KNOTS ( ( 2, 2 ),
 ( 3, 2, 2, 2, 2, 2, 2, 2, 2, 2, 2, 2, 2, 2, 2, 2, 2, 2, 2, 2, 2, 2, 2, 2, 2, 2, 2, 2, 2, 2, 2, 2, 2, 2, 2, 2, 2, 2, 2, 2, 2, 2, 2, 2, 2, 2, 2, 2, 2, 2, 2, 2, 2, 2, 2, 2, 2, 2, 2, 2, 2, 2, 2, 2, 2, 2, 2, 2, 2, 2, 2, 2, 2, 2, 2, 2, 2, 2, 2, 2, 2, 2, 2, 2, 2, 2, 2, 2, 2, 2, 2, 2, 2, 2, 2, 2, 2, 2, 2, 2, 2, 2, 2, 2, 2, 2, 2, 2, 2, 2, 2, 2, 2, 2, 2, 2, 2, 2, 2, 2, 2, 2, 2, 2, 2, 2, 2, 2, 2, 2, 2, 2, 2, 2, 2, 2, 2, 2, 2, 2, 2, 2, 2, 2, 2, 2, 2, 2, 2, 2, 2, 2, 2, 2, 2, 2, 2, 2, 2, 2, 2, 2, 2, 2, 2, 2, 2, 2, 2, 2, 2, 2, 2, 2, 2, 2, 2, 2, 2, 2, 2, 2, 2, 2, 2, 2, 2, 2, 2, 2, 2, 2, 2, 2, 2, 2, 2, 2, 2, 2, 2, 2, 2, 2, 2, 2, 2, 2, 2, 2, 2, 2, 2, 2, 2, 2, 2, 2, 2, 2, 2, 2, 2, 2, 2, 2, 2, 2, 2, 2, 2, 2, 2, 2, 2, 2, 2, 2, 2, 2, 2, 2, 2, 2, 2, 2, 2, 2, 2, 2, 2, 2, 2, 2, 2, 2, 2, 2, 2, 2, 2, 2, 2, 2, 2, 2, 2, 2, 2, 2, 2, 2, 2, 2, 2, 2, 2, 2, 2, 2, 2, 2, 2, 2, 2, 2, 2, 2, 2, 2, 2, 2, 2, 2, 2, 2, 2, 2, 2, 2, 2, 2, 2, 2, 2, 2, 2, 2, 2, 2, 2, 2, 2, 2, 2, 2, 2, 2, 2, 2, 2, 2, 2, 2, 2, 2, 2, 2, 2, 2, 2, 2, 2, 2, 2, 2, 2, 2, 2, 2, 2, 2, 2, 2, 2, 2, 2, 2, 2, 2, 2, 2, 2, 2, 2, 2, 2, 2, 2, 2, 2, 2, 2, 2, 2, 2, 2, 2, 2, 2, 2, 2, 2, 2, 2, 2, 2, 2, 2, 2, 2, 2, 2, 2, 2, 2, 2, 2, 2, 2, 3 ),
 ( 0.000000000000000000, 1.000000000000000000 ),
 ( 0.000000000000000000, 0.002564102564102564100, 0.005128205128205128201, 0.007692307692307692735, 0.01025641025641025640, 0.01282051282051282007, 0.01538461538461538547, 0.01794871794871794740, 0.02051282051282051280, 0.02307692307692307820, 0.02564102564102564014, 0.02820512820512820554, 0.03076923076923077094, 0.03333333333333333287, 0.03589743589743589480, 0.03846153846153846367, 0.04102564102564102561, 0.04358974358974358754, 0.04615384615384615641, 0.04871794871794871834, 0.05128205128205128027, 0.05384615384615384914, 0.05641025641025641107, 0.05897435897435897301, 0.06153846153846154188, 0.06410256410256409687, 0.06666666666666666574, 0.06923076923076923461, 0.07179487179487178961, 0.07435897435897435848, 0.07692307692307692735, 0.07948717948717948234, 0.08205128205128205121, 0.08461538461538462008, 0.08717948717948717507, 0.08974358974358974395, 0.09230769230769231282, 0.09487179487179486781, 0.09743589743589743668, 0.1000000000000000056, 0.1025641025641025605, 0.1051282051282051294, 0.1076923076923076983, 0.1102564102564102533, 0.1128205128205128221, 0.1153846153846153910, 0.1179487179487179460, 0.1205128205128205149, 0.1230769230769230838, 0.1256410256410256387, 0.1282051282051281937, 0.1307692307692307765, 0.1333333333333333315, 0.1358974358974358865, 0.1384615384615384692, 0.1410256410256410242, 0.1435897435897435792, 0.1461538461538461620, 0.1487179487179487170, 0.1512820512820512719, 0.1538461538461538547, 0.1564102564102564097, 0.1589743589743589647, 0.1615384615384615474, 0.1641025641025641024, 0.1666666666666666574, 0.1692307692307692402, 0.1717948717948717952, 0.1743589743589743501, 0.1769230769230769329, 0.1794871794871794879, 0.1820512820512820429, 0.1846153846153846256, 0.1871794871794871806, 0.1897435897435897356, 0.1923076923076923184, 0.1948717948717948734, 0.1974358974358974284, 0.2000000000000000111, 0.2025641025641025661, 0.2051282051282051211, 0.2076923076923077038, 0.2102564102564102588, 0.2128205128205128138, 0.2153846153846153966, 0.2179487179487179516, 0.2205128205128205066, 0.2230769230769230893, 0.2256410256410256443, 0.2282051282051281993, 0.2307692307692307820, 0.2333333333333333370, 0.2358974358974358920, 0.2384615384615384748, 0.2410256410256410298, 0.2435897435897435848, 0.2461538461538461675, 0.2487179487179487225, 0.2512820512820512775, 0.2538461538461538325, 0.2564102564102563875, 0.2589743589743589980, 0.2615384615384615530, 0.2641025641025641080, 0.2666666666666666630, 0.2692307692307692180, 0.2717948717948717730, 0.2743589743589743835, 0.2769230769230769384, 0.2794871794871794934, 0.2820512820512820484, 0.2846153846153846034, 0.2871794871794871584, 0.2897435897435897689, 0.2923076923076923239, 0.2948717948717948789, 0.2974358974358974339, 0.2999999999999999889, 0.3025641025641025439, 0.3051282051282051544, 0.3076923076923077094, 0.3102564102564102644, 0.3128205128205128194, 0.3153846153846153744, 0.3179487179487179294, 0.3205128205128205399, 0.3230769230769230949, 0.3256410256410256499, 0.3282051282051282048, 0.3307692307692307598, 0.3333333333333333148, 0.3358974358974358698, 0.3384615384615384803, 0.3410256410256410353, 0.3435897435897435903, 0.3461538461538461453, 0.3487179487179487003, 0.3512820512820512553, 0.3538461538461538658, 0.3564102564102564208, 0.3589743589743589758, 0.3615384615384615308, 0.3641025641025640858, 0.3666666666666666408, 0.3692307692307692513, 0.3717948717948718063, 0.3743589743589743613, 0.3769230769230769162, 0.3794871794871794712, 0.3820512820512820262, 0.3846153846153846367, 0.3871794871794871917, 0.3897435897435897467, 0.3923076923076923017, 0.3948717948717948567, 0.3974358974358974117, 0.4000000000000000222, 0.4025641025641025772, 0.4051282051282051322, 0.4076923076923076872, 0.4102564102564102422, 0.4128205128205127972, 0.4153846153846154077, 0.4179487179487179627, 0.4205128205128205177, 0.4230769230769230727, 0.4256410256410256276, 0.4282051282051281826, 0.4307692307692307931, 0.4333333333333333481, 0.4358974358974359031, 0.4384615384615384581, 0.4410256410256410131, 0.4435897435897435681, 0.4461538461538461786, 0.4487179487179487336, 0.4512820512820512886, 0.4538461538461538436, 0.4564102564102563986, 0.4589743589743589536, 0.4615384615384615641, 0.4641025641025641191, 0.4666666666666666741, 0.4692307692307692291, 0.4717948717948717841, 0.4743589743589743390, 0.4769230769230769496, 0.4794871794871795045, 0.4820512820512820595, 0.4846153846153846145, 0.4871794871794871695, 0.4897435897435897245, 0.4923076923076923350, 0.4948717948717948900, 0.4974358974358974450, 0.5000000000000000000, 0.5025641025641025550, 0.5051282051282051100, 0.5076923076923076650, 0.5102564102564102200, 0.5128205128205127750, 0.5153846153846153300, 0.5179487179487179960, 0.5205128205128205510, 0.5230769230769231060, 0.5256410256410256610, 0.5282051282051282159, 0.5307692307692307709, 0.5333333333333333259, 0.5358974358974358809, 0.5384615384615384359, 0.5410256410256409909, 0.5435897435897435459, 0.5461538461538461009, 0.5487179487179487669, 0.5512820512820513219, 0.5538461538461538769, 0.5564102564102564319, 0.5589743589743589869, 0.5615384615384615419, 0.5641025641025640969, 0.5666666666666666519, 0.5692307692307692069, 0.5717948717948717618, 0.5743589743589743168, 0.5769230769230768718, 0.5794871794871795379, 0.5820512820512820928, 0.5846153846153846478, 0.5871794871794872028, 0.5897435897435897578, 0.5923076923076923128, 0.5948717948717948678, 0.5974358974358974228, 0.5999999999999999778, 0.6025641025641025328, 0.6051282051282050878, 0.6076923076923076428, 0.6102564102564103088, 0.6128205128205128638, 0.6153846153846154188, 0.6179487179487179738, 0.6205128205128205288, 0.6230769230769230838, 0.6256410256410256387, 0.6282051282051281937, 0.6307692307692307487, 0.6333333333333333037, 0.6358974358974358587, 0.6384615384615384137, 0.6410256410256410797, 0.6435897435897436347, 0.6461538461538461897, 0.6487179487179487447, 0.6512820512820512997, 0.6538461538461538547, 0.6564102564102564097, 0.6589743589743589647, 0.6615384615384615197, 0.6641025641025640747, 0.6666666666666666297, 0.6692307692307691847, 0.6717948717948717396, 0.6743589743589744057, 0.6769230769230769607, 0.6794871794871795156, 0.6820512820512820706, 0.6846153846153846256, 0.6871794871794871806, 0.6897435897435897356, 0.6923076923076922906, 0.6948717948717948456, 0.6974358974358974006, 0.6999999999999999556, 0.7025641025641025106, 0.7051282051282051766, 0.7076923076923077316, 0.7102564102564102866, 0.7128205128205128416, 0.7153846153846153966, 0.7179487179487179516, 0.7205128205128205066, 0.7230769230769230616, 0.7256410256410256165, 0.7282051282051281715, 0.7307692307692307265, 0.7333333333333332815, 0.7358974358974359475, 0.7384615384615385025, 0.7410256410256410575, 0.7435897435897436125, 0.7461538461538461675, 0.7487179487179487225, 0.7512820512820512775, 0.7538461538461538325, 0.7564102564102563875, 0.7589743589743589425, 0.7615384615384614975, 0.7641025641025640525, 0.7666666666666667185, 0.7692307692307692735, 0.7717948717948718285, 0.7743589743589743835, 0.7769230769230769384, 0.7794871794871794934, 0.7820512820512820484, 0.7846153846153846034, 0.7871794871794871584, 0.7897435897435897134, 0.7923076923076922684, 0.7948717948717948234, 0.7974358974358974894, 0.8000000000000000444, 0.8025641025641025994, 0.8051282051282051544, 0.8076923076923077094, 0.8102564102564102644, 0.8128205128205128194, 0.8153846153846153744, 0.8179487179487179294, 0.8205128205128204844, 0.8230769230769230393, 0.8256410256410255943, 0.8282051282051282604, 0.8307692307692308153, 0.8333333333333333703, 0.8358974358974359253, 0.8384615384615384803, 0.8410256410256410353, 0.8435897435897435903, 0.8461538461538461453, 0.8487179487179487003, 0.8512820512820512553, 0.8538461538461538103, 0.8564102564102563653, 0.8589743589743589203, 0.8615384615384615863, 0.8641025641025641413, 0.8666666666666666963, 0.8692307692307692513, 0.8717948717948718063, 0.8743589743589743613, 0.8769230769230769162, 0.8794871794871794712, 0.8820512820512820262, 0.8846153846153845812, 0.8871794871794871362, 0.8897435897435896912, 0.8923076923076923572, 0.8948717948717949122, 0.8974358974358974672, 0.9000000000000000222, 0.9025641025641025772, 0.9051282051282051322, 0.9076923076923076872, 0.9102564102564102422, 0.9128205128205127972, 0.9153846153846153522, 0.9179487179487179072, 0.9205128205128204621, 0.9230769230769231282, 0.9256410256410256832, 0.9282051282051282382, 0.9307692307692307931, 0.9333333333333333481, 0.9358974358974359031, 0.9384615384615384581, 0.9410256410256410131, 0.9435897435897435681, 0.9461538461538461231, 0.9487179487179486781, 0.9512820512820512331, 0.9538461538461538991, 0.9564102564102564541, 0.9589743589743590091, 0.9615384615384615641, 0.9641025641025641191, 0.9666666666666666741, 0.9692307692307692291, 0.9717948717948717841, 0.9743589743589743390, 0.9769230769230768940, 0.9794871794871794490, 0.9820512820512820040, 0.9846153846153846700, 0.9871794871794872250, 0.9897435897435897800, 0.9923076923076923350, 0.9948717948717948900, 0.9974358974358974450, 1.000000000000000000 ),
 .UNSPECIFIED. ) 
 GEOMETRIC_REPRESENTATION_ITEM ( )  RATIONAL_B_SPLINE_SURFACE ( (
 ( 1.000000000000000000, 0.9510565162951535312, 1.000000000000000000, 0.9510565162951535312, 1.000000000000000000, 0.9510565162951535312, 1.000000000000000000, 0.9510565162951535312, 1.000000000000000000, 0.9510565162951535312, 1.000000000000000000, 0.9510565162951535312, 1.000000000000000000, 0.9510565162951535312, 1.000000000000000000, 0.9510565162951535312, 1.000000000000000000, 0.9510565162951535312, 1.000000000000000000, 0.9510565162951535312, 1.000000000000000000, 0.9510565162951535312, 1.000000000000000000, 0.9510565162951535312, 1.000000000000000000, 0.9510565162951535312, 1.000000000000000000, 0.9510565162951535312, 1.000000000000000000, 0.9510565162951535312, 1.000000000000000000, 0.9510565162951535312, 1.000000000000000000, 0.9510565162951535312, 1.000000000000000000, 0.9510565162951535312, 1.000000000000000000, 0.9510565162951535312, 1.000000000000000000, 0.9510565162951535312, 1.000000000000000000, 0.9510565162951535312, 1.000000000000000000, 0.9510565162951535312, 1.000000000000000000, 0.9510565162951535312, 1.000000000000000000, 0.9510565162951535312, 1.000000000000000000, 0.9510565162951535312, 1.000000000000000000, 0.9510565162951535312, 1.000000000000000000, 0.9510565162951535312, 1.000000000000000000, 0.9510565162951535312, 1.000000000000000000, 0.9510565162951535312, 1.000000000000000000, 0.9510565162951535312, 1.000000000000000000, 0.9510565162951535312, 1.000000000000000000, 0.9510565162951535312, 1.000000000000000000, 0.9510565162951535312, 1.000000000000000000, 0.9510565162951535312, 1.000000000000000000, 0.9510565162951535312, 1.000000000000000000, 0.9510565162951535312, 1.000000000000000000, 0.9510565162951535312, 1.000000000000000000, 0.9510565162951535312, 1.000000000000000000, 0.9510565162951535312, 1.000000000000000000, 0.9510565162951535312, 1.000000000000000000, 0.9510565162951535312, 1.000000000000000000, 0.9510565162951535312, 1.000000000000000000, 0.9510565162951535312, 1.000000000000000000, 0.9510565162951535312, 1.000000000000000000, 0.9510565162951535312, 1.000000000000000000, 0.9510565162951535312, 1.000000000000000000, 0.9510565162951535312, 1.000000000000000000, 0.9510565162951535312, 1.000000000000000000, 0.9510565162951535312, 1.000000000000000000, 0.9510565162951535312, 1.000000000000000000, 0.9510565162951535312, 1.000000000000000000, 0.9510565162951535312, 1.000000000000000000, 0.9510565162951535312, 1.000000000000000000, 0.9510565162951535312, 1.000000000000000000, 0.9510565162951535312, 1.000000000000000000, 0.9510565162951535312, 1.000000000000000000, 0.9510565162951535312, 1.000000000000000000, 0.9510565162951535312, 1.000000000000000000, 0.9510565162951535312, 1.000000000000000000, 0.9510565162951535312, 1.000000000000000000, 0.9510565162951535312, 1.000000000000000000, 0.9510565162951535312, 1.000000000000000000, 0.9510565162951535312, 1.000000000000000000, 0.9510565162951535312, 1.000000000000000000, 0.9510565162951535312, 1.000000000000000000, 0.9510565162951535312, 1.000000000000000000, 0.9510565162951535312, 1.000000000000000000, 0.9510565162951535312, 1.000000000000000000, 0.9510565162951535312, 1.000000000000000000, 0.9510565162951535312, 1.000000000000000000, 0.9510565162951535312, 1.000000000000000000, 0.9510565162951535312, 1.000000000000000000, 0.9510565162951535312, 1.000000000000000000, 0.9510565162951535312, 1.000000000000000000, 0.9510565162951535312, 1.000000000000000000, 0.9510565162951535312, 1.000000000000000000, 0.9510565162951535312, 1.000000000000000000, 0.9510565162951535312, 1.000000000000000000, 0.9510565162951535312, 1.000000000000000000, 0.9510565162951535312, 1.000000000000000000, 0.9510565162951535312, 1.000000000000000000, 0.9510565162951535312, 1.000000000000000000, 0.9510565162951535312, 1.000000000000000000, 0.9510565162951535312, 1.000000000000000000, 0.9510565162951535312, 1.000000000000000000, 0.9510565162951535312, 1.000000000000000000, 0.9510565162951535312, 1.000000000000000000, 0.9510565162951535312, 1.000000000000000000, 0.9510565162951535312, 1.000000000000000000, 0.9510565162951535312, 1.000000000000000000, 0.9510565162951535312, 1.000000000000000000, 0.9510565162951535312, 1.000000000000000000, 0.9510565162951535312, 1.000000000000000000, 0.9510565162951535312, 1.000000000000000000, 0.9510565162951535312, 1.000000000000000000, 0.9510565162951535312, 1.000000000000000000, 0.9510565162951535312, 1.000000000000000000, 0.9510565162951535312, 1.000000000000000000, 0.9510565162951535312, 1.000000000000000000, 0.9510565162951535312, 1.000000000000000000, 0.9510565162951535312, 1.000000000000000000, 0.9510565162951535312, 1.000000000000000000, 0.9510565162951535312, 1.000000000000000000, 0.9510565162951535312, 1.000000000000000000, 0.9510565162951535312, 1.000000000000000000, 0.9510565162951535312, 1.000000000000000000, 0.9510565162951535312, 1.000000000000000000, 0.9510565162951535312, 1.000000000000000000, 0.9510565162951535312, 1.000000000000000000, 0.9510565162951535312, 1.000000000000000000, 0.9510565162951535312, 1.000000000000000000, 0.9510565162951535312, 1.000000000000000000, 0.9510565162951535312, 1.000000000000000000, 0.9510565162951535312, 1.000000000000000000, 0.9510565162951535312, 1.000000000000000000, 0.9510565162951535312, 1.000000000000000000, 0.9510565162951535312, 1.000000000000000000, 0.9510565162951535312, 1.000000000000000000, 0.9510565162951535312, 1.000000000000000000, 0.9510565162951535312, 1.000000000000000000, 0.9510565162951535312, 1.000000000000000000, 0.9510565162951535312, 1.000000000000000000, 0.9510565162951535312, 1.000000000000000000, 0.9510565162951535312, 1.000000000000000000, 0.9510565162951535312, 1.000000000000000000, 0.9510565162951535312, 1.000000000000000000, 0.9510565162951535312, 1.000000000000000000, 0.9510565162951535312, 1.000000000000000000, 0.9510565162951535312, 1.000000000000000000, 0.9510565162951535312, 1.000000000000000000, 0.9510565162951535312, 1.000000000000000000, 0.9510565162951535312, 1.000000000000000000, 0.9510565162951535312, 1.000000000000000000, 0.9510565162951535312, 1.000000000000000000, 0.9510565162951535312, 1.000000000000000000, 0.9510565162951535312, 1.000000000000000000, 0.9510565162951535312, 1.000000000000000000, 0.9510565162951535312, 1.000000000000000000, 0.9510565162951535312, 1.000000000000000000, 0.9510565162951535312, 1.000000000000000000, 0.9510565162951535312, 1.000000000000000000, 0.9510565162951535312, 1.000000000000000000, 0.9510565162951535312, 1.000000000000000000, 0.9510565162951535312, 1.000000000000000000, 0.9510565162951535312, 1.000000000000000000, 0.9510565162951535312, 1.000000000000000000, 0.9510565162951535312, 1.000000000000000000, 0.9510565162951535312, 1.000000000000000000, 0.9510565162951535312, 1.000000000000000000, 0.9510565162951535312, 1.000000000000000000, 0.9510565162951535312, 1.000000000000000000, 0.9510565162951535312, 1.000000000000000000, 0.9510565162951535312, 1.000000000000000000, 0.9510565162951535312, 1.000000000000000000, 0.9510565162951535312, 1.000000000000000000, 0.9510565162951535312, 1.000000000000000000, 0.9510565162951535312, 1.000000000000000000, 0.9510565162951535312, 1.000000000000000000, 0.9510565162951535312, 1.000000000000000000, 0.9510565162951535312, 1.000000000000000000, 0.9510565162951535312, 1.000000000000000000, 0.9510565162951535312, 1.000000000000000000, 0.9510565162951535312, 1.000000000000000000, 0.9510565162951535312, 1.000000000000000000, 0.9510565162951535312, 1.000000000000000000, 0.9510565162951535312, 1.000000000000000000, 0.9510565162951535312, 1.000000000000000000, 0.9510565162951535312, 1.000000000000000000, 0.9510565162951535312, 1.000000000000000000, 0.9510565162951535312, 1.000000000000000000, 0.9510565162951535312, 1.000000000000000000, 0.9510565162951535312, 1.000000000000000000, 0.9510565162951535312, 1.000000000000000000, 0.9510565162951535312, 1.000000000000000000, 0.9510565162951535312, 1.000000000000000000, 0.9510565162951535312, 1.000000000000000000, 0.9510565162951535312, 1.000000000000000000, 0.9510565162951535312, 1.000000000000000000, 0.9510565162951535312, 1.000000000000000000, 0.9510565162951535312, 1.000000000000000000, 0.9510565162951535312, 1.000000000000000000, 0.9510565162951535312, 1.000000000000000000, 0.9510565162951535312, 1.000000000000000000, 0.9510565162951535312, 1.000000000000000000, 0.9510565162951535312, 1.000000000000000000, 0.9510565162951535312, 1.000000000000000000, 0.9510565162951535312, 1.000000000000000000, 0.9510565162951535312, 1.000000000000000000, 0.9510565162951535312, 1.000000000000000000, 0.9510565162951535312, 1.000000000000000000, 0.9510565162951535312, 1.000000000000000000, 0.9510565162951535312, 1.000000000000000000, 0.9510565162951535312, 1.000000000000000000, 0.9510565162951535312, 1.000000000000000000, 0.9510565162951535312, 1.000000000000000000, 0.9510565162951535312, 1.000000000000000000, 0.9510565162951535312, 1.000000000000000000, 0.9510565162951535312, 1.000000000000000000, 0.9510565162951535312, 1.000000000000000000, 0.9510565162951535312, 1.000000000000000000, 0.9510565162951535312, 1.000000000000000000, 0.9510565162951535312, 1.000000000000000000, 0.9510565162951535312, 1.000000000000000000, 0.9510565162951535312, 1.000000000000000000, 0.9510565162951535312, 1.000000000000000000, 0.9510565162951535312, 1.000000000000000000, 0.9510565162951535312, 1.000000000000000000, 0.9510565162951535312, 1.000000000000000000, 0.9510565162951535312, 1.000000000000000000, 0.9510565162951535312, 1.000000000000000000, 0.9510565162951535312, 1.000000000000000000, 0.9510565162951535312, 1.000000000000000000, 0.9510565162951535312, 1.000000000000000000, 0.9510565162951535312, 1.000000000000000000, 0.9510565162951535312, 1.000000000000000000, 0.9510565162951535312, 1.000000000000000000, 0.9510565162951535312, 1.000000000000000000, 0.9510565162951535312, 1.000000000000000000, 0.9510565162951535312, 1.000000000000000000, 0.9510565162951535312, 1.000000000000000000, 0.9510565162951535312, 1.000000000000000000, 0.9510565162951535312, 1.000000000000000000, 0.9510565162951535312, 1.000000000000000000, 0.9510565162951535312, 1.000000000000000000, 0.9510565162951535312, 1.000000000000000000, 0.9510565162951535312, 1.000000000000000000, 0.9510565162951535312, 1.000000000000000000, 0.9510565162951535312, 1.000000000000000000, 0.9510565162951535312, 1.000000000000000000, 0.9510565162951535312, 1.000000000000000000, 0.9510565162951535312, 1.000000000000000000, 0.9510565162951535312, 1.000000000000000000, 0.9510565162951535312, 1.000000000000000000, 0.9510565162951535312, 1.000000000000000000, 0.9510565162951535312, 1.000000000000000000, 0.9510565162951535312, 1.000000000000000000, 0.9510565162951535312, 1.000000000000000000, 0.9510565162951535312, 1.000000000000000000, 0.9510565162951535312, 1.000000000000000000, 0.9510565162951535312, 1.000000000000000000, 0.9510565162951535312, 1.000000000000000000, 0.9510565162951535312, 1.000000000000000000, 0.9510565162951535312, 1.000000000000000000, 0.9510565162951535312, 1.000000000000000000, 0.9510565162951535312, 1.000000000000000000, 0.9510565162951535312, 1.000000000000000000, 0.9510565162951535312, 1.000000000000000000, 0.9510565162951535312, 1.000000000000000000, 0.9510565162951535312, 1.000000000000000000, 0.9510565162951535312, 1.000000000000000000, 0.9510565162951535312, 1.000000000000000000, 0.9510565162951535312, 1.000000000000000000, 0.9510565162951535312, 1.000000000000000000, 0.9510565162951535312, 1.000000000000000000, 0.9510565162951535312, 1.000000000000000000, 0.9510565162951535312, 1.000000000000000000, 0.9510565162951535312, 1.000000000000000000, 0.9510565162951535312, 1.000000000000000000, 0.9510565162951535312, 1.000000000000000000, 0.9510565162951535312, 1.000000000000000000, 0.9510565162951535312, 1.000000000000000000, 0.9510565162951535312, 1.000000000000000000, 0.9510565162951535312, 1.000000000000000000, 0.9510565162951535312, 1.000000000000000000, 0.9510565162951535312, 1.000000000000000000, 0.9510565162951535312, 1.000000000000000000, 0.9510565162951535312, 1.000000000000000000, 0.9510565162951535312, 1.000000000000000000, 0.9510565162951535312, 1.000000000000000000, 0.9510565162951535312, 1.000000000000000000, 0.9510565162951535312, 1.000000000000000000, 0.9510565162951535312, 1.000000000000000000, 0.9510565162951535312, 1.000000000000000000, 0.9510565162951535312, 1.000000000000000000, 0.9510565162951535312, 1.000000000000000000, 0.9510565162951535312, 1.000000000000000000, 0.9510565162951535312, 1.000000000000000000, 0.9510565162951535312, 1.000000000000000000, 0.9510565162951535312, 1.000000000000000000, 0.9510565162951535312, 1.000000000000000000, 0.9510565162951535312, 1.000000000000000000, 0.9510565162951535312, 1.000000000000000000, 0.9510565162951535312, 1.000000000000000000, 0.9510565162951535312, 1.000000000000000000, 0.9510565162951535312, 1.000000000000000000, 0.9510565162951535312, 1.000000000000000000, 0.9510565162951535312, 1.000000000000000000, 0.9510565162951535312, 1.000000000000000000, 0.9510565162951535312, 1.000000000000000000, 0.9510565162951535312, 1.000000000000000000, 0.9510565162951535312, 1.000000000000000000, 0.9510565162951535312, 1.000000000000000000, 0.9510565162951535312, 1.000000000000000000, 0.9510565162951535312, 1.000000000000000000, 0.9510565162951535312, 1.000000000000000000, 0.9510565162951535312, 1.000000000000000000, 0.9510565162951535312, 1.000000000000000000, 0.9510565162951535312, 1.000000000000000000, 0.9510565162951535312, 1.000000000000000000, 0.9510565162951535312, 1.000000000000000000, 0.9510565162951535312, 1.000000000000000000, 0.9510565162951535312, 1.000000000000000000, 0.9510565162951535312, 1.000000000000000000, 0.9510565162951535312, 1.000000000000000000, 0.9510565162951535312, 1.000000000000000000, 0.9510565162951535312, 1.000000000000000000, 0.9510565162951535312, 1.000000000000000000, 0.9510565162951535312, 1.000000000000000000, 0.9510565162951535312, 1.000000000000000000, 0.9510565162951535312, 1.000000000000000000, 0.9510565162951535312, 1.000000000000000000, 0.9510565162951535312, 1.000000000000000000, 0.9510565162951535312, 1.000000000000000000, 0.9510565162951535312, 1.000000000000000000, 0.9510565162951535312, 1.000000000000000000, 0.9510565162951535312, 1.000000000000000000, 0.9510565162951535312, 1.000000000000000000, 0.9510565162951535312, 1.000000000000000000, 0.9510565162951535312, 1.000000000000000000, 0.9510565162951535312, 1.000000000000000000, 0.9510565162951535312, 1.000000000000000000, 0.9510565162951535312, 1.000000000000000000, 0.9510565162951535312, 1.000000000000000000, 0.9510565162951535312, 1.000000000000000000, 0.9510565162951535312, 1.000000000000000000, 0.9510565162951535312, 1.000000000000000000, 0.9510565162951535312, 1.000000000000000000, 0.9510565162951535312, 1.000000000000000000, 0.9510565162951535312, 1.000000000000000000, 0.9510565162951535312, 1.000000000000000000, 0.9510565162951535312, 1.000000000000000000, 0.9510565162951535312, 1.000000000000000000, 0.9510565162951535312, 1.000000000000000000, 0.9510565162951535312, 1.000000000000000000, 0.9510565162951535312, 1.000000000000000000, 0.9510565162951535312, 1.000000000000000000, 0.9510565162951535312, 1.000000000000000000, 0.9510565162951535312, 1.000000000000000000, 0.9510565162951535312, 1.000000000000000000, 0.9510565162951535312, 1.000000000000000000, 0.9510565162951535312, 1.000000000000000000, 0.9510565162951535312, 1.000000000000000000, 0.9510565162951535312, 1.000000000000000000, 0.9510565162951535312, 1.000000000000000000, 0.9510565162951535312, 1.000000000000000000, 0.9510565162951535312, 1.000000000000000000, 0.9510565162951535312, 1.000000000000000000, 0.9510565162951535312, 1.000000000000000000, 0.9510565162951535312, 1.000000000000000000, 0.9510565162951535312, 1.000000000000000000, 0.9510565162951535312, 1.000000000000000000, 0.9510565162951535312, 1.000000000000000000, 0.9510565162951535312, 1.000000000000000000, 0.9510565162951535312, 1.000000000000000000, 0.9510565162951535312, 1.000000000000000000, 0.9510565162951535312, 1.000000000000000000, 0.9510565162951535312, 1.000000000000000000, 0.9510565162951535312, 1.000000000000000000, 0.9510565162951535312, 1.000000000000000000, 0.9510565162951535312, 1.000000000000000000, 0.9510565162951535312, 1.000000000000000000, 0.9510565162951535312, 1.000000000000000000, 0.9510565162951535312, 1.000000000000000000, 0.9510565162951535312, 1.000000000000000000, 0.9510565162951535312, 1.000000000000000000, 0.9510565162951535312, 1.000000000000000000, 0.9510565162951535312, 1.000000000000000000, 0.9510565162951535312, 1.000000000000000000, 0.9510565162951535312, 1.000000000000000000, 0.9510565162951535312, 1.000000000000000000, 0.9510565162951535312, 1.000000000000000000, 0.9510565162951535312, 1.000000000000000000, 0.9510565162951535312, 1.000000000000000000, 0.9510565162951535312, 1.000000000000000000, 0.9510565162951535312, 1.000000000000000000, 0.9510565162951535312, 1.000000000000000000, 0.9510565162951535312, 1.000000000000000000, 0.9510565162951535312, 1.000000000000000000, 0.9510565162951535312, 1.000000000000000000, 0.9510565162951535312, 1.000000000000000000, 0.9510565162951535312, 1.000000000000000000, 0.9510565162951535312, 1.000000000000000000, 0.9510565162951535312, 1.000000000000000000, 0.9510565162951535312, 1.000000000000000000, 0.9510565162951535312, 1.000000000000000000, 0.9510565162951535312, 1.000000000000000000, 0.9510565162951535312, 1.000000000000000000, 0.9510565162951535312, 1.000000000000000000, 0.9510565162951535312, 1.000000000000000000, 0.9510565162951535312, 1.000000000000000000),
 ( 1.000000000000000000, 0.9510565162951535312, 1.000000000000000000, 0.9510565162951535312, 1.000000000000000000, 0.9510565162951535312, 1.000000000000000000, 0.9510565162951535312, 1.000000000000000000, 0.9510565162951535312, 1.000000000000000000, 0.9510565162951535312, 1.000000000000000000, 0.9510565162951535312, 1.000000000000000000, 0.9510565162951535312, 1.000000000000000000, 0.9510565162951535312, 1.000000000000000000, 0.9510565162951535312, 1.000000000000000000, 0.9510565162951535312, 1.000000000000000000, 0.9510565162951535312, 1.000000000000000000, 0.9510565162951535312, 1.000000000000000000, 0.9510565162951535312, 1.000000000000000000, 0.9510565162951535312, 1.000000000000000000, 0.9510565162951535312, 1.000000000000000000, 0.9510565162951535312, 1.000000000000000000, 0.9510565162951535312, 1.000000000000000000, 0.9510565162951535312, 1.000000000000000000, 0.9510565162951535312, 1.000000000000000000, 0.9510565162951535312, 1.000000000000000000, 0.9510565162951535312, 1.000000000000000000, 0.9510565162951535312, 1.000000000000000000, 0.9510565162951535312, 1.000000000000000000, 0.9510565162951535312, 1.000000000000000000, 0.9510565162951535312, 1.000000000000000000, 0.9510565162951535312, 1.000000000000000000, 0.9510565162951535312, 1.000000000000000000, 0.9510565162951535312, 1.000000000000000000, 0.9510565162951535312, 1.000000000000000000, 0.9510565162951535312, 1.000000000000000000, 0.9510565162951535312, 1.000000000000000000, 0.9510565162951535312, 1.000000000000000000, 0.9510565162951535312, 1.000000000000000000, 0.9510565162951535312, 1.000000000000000000, 0.9510565162951535312, 1.000000000000000000, 0.9510565162951535312, 1.000000000000000000, 0.9510565162951535312, 1.000000000000000000, 0.9510565162951535312, 1.000000000000000000, 0.9510565162951535312, 1.000000000000000000, 0.9510565162951535312, 1.000000000000000000, 0.9510565162951535312, 1.000000000000000000, 0.9510565162951535312, 1.000000000000000000, 0.9510565162951535312, 1.000000000000000000, 0.9510565162951535312, 1.000000000000000000, 0.9510565162951535312, 1.000000000000000000, 0.9510565162951535312, 1.000000000000000000, 0.9510565162951535312, 1.000000000000000000, 0.9510565162951535312, 1.000000000000000000, 0.9510565162951535312, 1.000000000000000000, 0.9510565162951535312, 1.000000000000000000, 0.9510565162951535312, 1.000000000000000000, 0.9510565162951535312, 1.000000000000000000, 0.9510565162951535312, 1.000000000000000000, 0.9510565162951535312, 1.000000000000000000, 0.9510565162951535312, 1.000000000000000000, 0.9510565162951535312, 1.000000000000000000, 0.9510565162951535312, 1.000000000000000000, 0.9510565162951535312, 1.000000000000000000, 0.9510565162951535312, 1.000000000000000000, 0.9510565162951535312, 1.000000000000000000, 0.9510565162951535312, 1.000000000000000000, 0.9510565162951535312, 1.000000000000000000, 0.9510565162951535312, 1.000000000000000000, 0.9510565162951535312, 1.000000000000000000, 0.9510565162951535312, 1.000000000000000000, 0.9510565162951535312, 1.000000000000000000, 0.9510565162951535312, 1.000000000000000000, 0.9510565162951535312, 1.000000000000000000, 0.9510565162951535312, 1.000000000000000000, 0.9510565162951535312, 1.000000000000000000, 0.9510565162951535312, 1.000000000000000000, 0.9510565162951535312, 1.000000000000000000, 0.9510565162951535312, 1.000000000000000000, 0.9510565162951535312, 1.000000000000000000, 0.9510565162951535312, 1.000000000000000000, 0.9510565162951535312, 1.000000000000000000, 0.9510565162951535312, 1.000000000000000000, 0.9510565162951535312, 1.000000000000000000, 0.9510565162951535312, 1.000000000000000000, 0.9510565162951535312, 1.000000000000000000, 0.9510565162951535312, 1.000000000000000000, 0.9510565162951535312, 1.000000000000000000, 0.9510565162951535312, 1.000000000000000000, 0.9510565162951535312, 1.000000000000000000, 0.9510565162951535312, 1.000000000000000000, 0.9510565162951535312, 1.000000000000000000, 0.9510565162951535312, 1.000000000000000000, 0.9510565162951535312, 1.000000000000000000, 0.9510565162951535312, 1.000000000000000000, 0.9510565162951535312, 1.000000000000000000, 0.9510565162951535312, 1.000000000000000000, 0.9510565162951535312, 1.000000000000000000, 0.9510565162951535312, 1.000000000000000000, 0.9510565162951535312, 1.000000000000000000, 0.9510565162951535312, 1.000000000000000000, 0.9510565162951535312, 1.000000000000000000, 0.9510565162951535312, 1.000000000000000000, 0.9510565162951535312, 1.000000000000000000, 0.9510565162951535312, 1.000000000000000000, 0.9510565162951535312, 1.000000000000000000, 0.9510565162951535312, 1.000000000000000000, 0.9510565162951535312, 1.000000000000000000, 0.9510565162951535312, 1.000000000000000000, 0.9510565162951535312, 1.000000000000000000, 0.9510565162951535312, 1.000000000000000000, 0.9510565162951535312, 1.000000000000000000, 0.9510565162951535312, 1.000000000000000000, 0.9510565162951535312, 1.000000000000000000, 0.9510565162951535312, 1.000000000000000000, 0.9510565162951535312, 1.000000000000000000, 0.9510565162951535312, 1.000000000000000000, 0.9510565162951535312, 1.000000000000000000, 0.9510565162951535312, 1.000000000000000000, 0.9510565162951535312, 1.000000000000000000, 0.9510565162951535312, 1.000000000000000000, 0.9510565162951535312, 1.000000000000000000, 0.9510565162951535312, 1.000000000000000000, 0.9510565162951535312, 1.000000000000000000, 0.9510565162951535312, 1.000000000000000000, 0.9510565162951535312, 1.000000000000000000, 0.9510565162951535312, 1.000000000000000000, 0.9510565162951535312, 1.000000000000000000, 0.9510565162951535312, 1.000000000000000000, 0.9510565162951535312, 1.000000000000000000, 0.9510565162951535312, 1.000000000000000000, 0.9510565162951535312, 1.000000000000000000, 0.9510565162951535312, 1.000000000000000000, 0.9510565162951535312, 1.000000000000000000, 0.9510565162951535312, 1.000000000000000000, 0.9510565162951535312, 1.000000000000000000, 0.9510565162951535312, 1.000000000000000000, 0.9510565162951535312, 1.000000000000000000, 0.9510565162951535312, 1.000000000000000000, 0.9510565162951535312, 1.000000000000000000, 0.9510565162951535312, 1.000000000000000000, 0.9510565162951535312, 1.000000000000000000, 0.9510565162951535312, 1.000000000000000000, 0.9510565162951535312, 1.000000000000000000, 0.9510565162951535312, 1.000000000000000000, 0.9510565162951535312, 1.000000000000000000, 0.9510565162951535312, 1.000000000000000000, 0.9510565162951535312, 1.000000000000000000, 0.9510565162951535312, 1.000000000000000000, 0.9510565162951535312, 1.000000000000000000, 0.9510565162951535312, 1.000000000000000000, 0.9510565162951535312, 1.000000000000000000, 0.9510565162951535312, 1.000000000000000000, 0.9510565162951535312, 1.000000000000000000, 0.9510565162951535312, 1.000000000000000000, 0.9510565162951535312, 1.000000000000000000, 0.9510565162951535312, 1.000000000000000000, 0.9510565162951535312, 1.000000000000000000, 0.9510565162951535312, 1.000000000000000000, 0.9510565162951535312, 1.000000000000000000, 0.9510565162951535312, 1.000000000000000000, 0.9510565162951535312, 1.000000000000000000, 0.9510565162951535312, 1.000000000000000000, 0.9510565162951535312, 1.000000000000000000, 0.9510565162951535312, 1.000000000000000000, 0.9510565162951535312, 1.000000000000000000, 0.9510565162951535312, 1.000000000000000000, 0.9510565162951535312, 1.000000000000000000, 0.9510565162951535312, 1.000000000000000000, 0.9510565162951535312, 1.000000000000000000, 0.9510565162951535312, 1.000000000000000000, 0.9510565162951535312, 1.000000000000000000, 0.9510565162951535312, 1.000000000000000000, 0.9510565162951535312, 1.000000000000000000, 0.9510565162951535312, 1.000000000000000000, 0.9510565162951535312, 1.000000000000000000, 0.9510565162951535312, 1.000000000000000000, 0.9510565162951535312, 1.000000000000000000, 0.9510565162951535312, 1.000000000000000000, 0.9510565162951535312, 1.000000000000000000, 0.9510565162951535312, 1.000000000000000000, 0.9510565162951535312, 1.000000000000000000, 0.9510565162951535312, 1.000000000000000000, 0.9510565162951535312, 1.000000000000000000, 0.9510565162951535312, 1.000000000000000000, 0.9510565162951535312, 1.000000000000000000, 0.9510565162951535312, 1.000000000000000000, 0.9510565162951535312, 1.000000000000000000, 0.9510565162951535312, 1.000000000000000000, 0.9510565162951535312, 1.000000000000000000, 0.9510565162951535312, 1.000000000000000000, 0.9510565162951535312, 1.000000000000000000, 0.9510565162951535312, 1.000000000000000000, 0.9510565162951535312, 1.000000000000000000, 0.9510565162951535312, 1.000000000000000000, 0.9510565162951535312, 1.000000000000000000, 0.9510565162951535312, 1.000000000000000000, 0.9510565162951535312, 1.000000000000000000, 0.9510565162951535312, 1.000000000000000000, 0.9510565162951535312, 1.000000000000000000, 0.9510565162951535312, 1.000000000000000000, 0.9510565162951535312, 1.000000000000000000, 0.9510565162951535312, 1.000000000000000000, 0.9510565162951535312, 1.000000000000000000, 0.9510565162951535312, 1.000000000000000000, 0.9510565162951535312, 1.000000000000000000, 0.9510565162951535312, 1.000000000000000000, 0.9510565162951535312, 1.000000000000000000, 0.9510565162951535312, 1.000000000000000000, 0.9510565162951535312, 1.000000000000000000, 0.9510565162951535312, 1.000000000000000000, 0.9510565162951535312, 1.000000000000000000, 0.9510565162951535312, 1.000000000000000000, 0.9510565162951535312, 1.000000000000000000, 0.9510565162951535312, 1.000000000000000000, 0.9510565162951535312, 1.000000000000000000, 0.9510565162951535312, 1.000000000000000000, 0.9510565162951535312, 1.000000000000000000, 0.9510565162951535312, 1.000000000000000000, 0.9510565162951535312, 1.000000000000000000, 0.9510565162951535312, 1.000000000000000000, 0.9510565162951535312, 1.000000000000000000, 0.9510565162951535312, 1.000000000000000000, 0.9510565162951535312, 1.000000000000000000, 0.9510565162951535312, 1.000000000000000000, 0.9510565162951535312, 1.000000000000000000, 0.9510565162951535312, 1.000000000000000000, 0.9510565162951535312, 1.000000000000000000, 0.9510565162951535312, 1.000000000000000000, 0.9510565162951535312, 1.000000000000000000, 0.9510565162951535312, 1.000000000000000000, 0.9510565162951535312, 1.000000000000000000, 0.9510565162951535312, 1.000000000000000000, 0.9510565162951535312, 1.000000000000000000, 0.9510565162951535312, 1.000000000000000000, 0.9510565162951535312, 1.000000000000000000, 0.9510565162951535312, 1.000000000000000000, 0.9510565162951535312, 1.000000000000000000, 0.9510565162951535312, 1.000000000000000000, 0.9510565162951535312, 1.000000000000000000, 0.9510565162951535312, 1.000000000000000000, 0.9510565162951535312, 1.000000000000000000, 0.9510565162951535312, 1.000000000000000000, 0.9510565162951535312, 1.000000000000000000, 0.9510565162951535312, 1.000000000000000000, 0.9510565162951535312, 1.000000000000000000, 0.9510565162951535312, 1.000000000000000000, 0.9510565162951535312, 1.000000000000000000, 0.9510565162951535312, 1.000000000000000000, 0.9510565162951535312, 1.000000000000000000, 0.9510565162951535312, 1.000000000000000000, 0.9510565162951535312, 1.000000000000000000, 0.9510565162951535312, 1.000000000000000000, 0.9510565162951535312, 1.000000000000000000, 0.9510565162951535312, 1.000000000000000000, 0.9510565162951535312, 1.000000000000000000, 0.9510565162951535312, 1.000000000000000000, 0.9510565162951535312, 1.000000000000000000, 0.9510565162951535312, 1.000000000000000000, 0.9510565162951535312, 1.000000000000000000, 0.9510565162951535312, 1.000000000000000000, 0.9510565162951535312, 1.000000000000000000, 0.9510565162951535312, 1.000000000000000000, 0.9510565162951535312, 1.000000000000000000, 0.9510565162951535312, 1.000000000000000000, 0.9510565162951535312, 1.000000000000000000, 0.9510565162951535312, 1.000000000000000000, 0.9510565162951535312, 1.000000000000000000, 0.9510565162951535312, 1.000000000000000000, 0.9510565162951535312, 1.000000000000000000, 0.9510565162951535312, 1.000000000000000000, 0.9510565162951535312, 1.000000000000000000, 0.9510565162951535312, 1.000000000000000000, 0.9510565162951535312, 1.000000000000000000, 0.9510565162951535312, 1.000000000000000000, 0.9510565162951535312, 1.000000000000000000, 0.9510565162951535312, 1.000000000000000000, 0.9510565162951535312, 1.000000000000000000, 0.9510565162951535312, 1.000000000000000000, 0.9510565162951535312, 1.000000000000000000, 0.9510565162951535312, 1.000000000000000000, 0.9510565162951535312, 1.000000000000000000, 0.9510565162951535312, 1.000000000000000000, 0.9510565162951535312, 1.000000000000000000, 0.9510565162951535312, 1.000000000000000000, 0.9510565162951535312, 1.000000000000000000, 0.9510565162951535312, 1.000000000000000000, 0.9510565162951535312, 1.000000000000000000, 0.9510565162951535312, 1.000000000000000000, 0.9510565162951535312, 1.000000000000000000, 0.9510565162951535312, 1.000000000000000000, 0.9510565162951535312, 1.000000000000000000, 0.9510565162951535312, 1.000000000000000000, 0.9510565162951535312, 1.000000000000000000, 0.9510565162951535312, 1.000000000000000000, 0.9510565162951535312, 1.000000000000000000, 0.9510565162951535312, 1.000000000000000000, 0.9510565162951535312, 1.000000000000000000, 0.9510565162951535312, 1.000000000000000000, 0.9510565162951535312, 1.000000000000000000, 0.9510565162951535312, 1.000000000000000000, 0.9510565162951535312, 1.000000000000000000, 0.9510565162951535312, 1.000000000000000000, 0.9510565162951535312, 1.000000000000000000, 0.9510565162951535312, 1.000000000000000000, 0.9510565162951535312, 1.000000000000000000, 0.9510565162951535312, 1.000000000000000000, 0.9510565162951535312, 1.000000000000000000, 0.9510565162951535312, 1.000000000000000000, 0.9510565162951535312, 1.000000000000000000, 0.9510565162951535312, 1.000000000000000000, 0.9510565162951535312, 1.000000000000000000, 0.9510565162951535312, 1.000000000000000000, 0.9510565162951535312, 1.000000000000000000, 0.9510565162951535312, 1.000000000000000000, 0.9510565162951535312, 1.000000000000000000, 0.9510565162951535312, 1.000000000000000000, 0.9510565162951535312, 1.000000000000000000, 0.9510565162951535312, 1.000000000000000000, 0.9510565162951535312, 1.000000000000000000, 0.9510565162951535312, 1.000000000000000000, 0.9510565162951535312, 1.000000000000000000, 0.9510565162951535312, 1.000000000000000000, 0.9510565162951535312, 1.000000000000000000, 0.9510565162951535312, 1.000000000000000000, 0.9510565162951535312, 1.000000000000000000, 0.9510565162951535312, 1.000000000000000000, 0.9510565162951535312, 1.000000000000000000, 0.9510565162951535312, 1.000000000000000000, 0.9510565162951535312, 1.000000000000000000, 0.9510565162951535312, 1.000000000000000000, 0.9510565162951535312, 1.000000000000000000, 0.9510565162951535312, 1.000000000000000000, 0.9510565162951535312, 1.000000000000000000, 0.9510565162951535312, 1.000000000000000000, 0.9510565162951535312, 1.000000000000000000, 0.9510565162951535312, 1.000000000000000000, 0.9510565162951535312, 1.000000000000000000, 0.9510565162951535312, 1.000000000000000000, 0.9510565162951535312, 1.000000000000000000, 0.9510565162951535312, 1.000000000000000000, 0.9510565162951535312, 1.000000000000000000, 0.9510565162951535312, 1.000000000000000000, 0.9510565162951535312, 1.000000000000000000, 0.9510565162951535312, 1.000000000000000000, 0.9510565162951535312, 1.000000000000000000, 0.9510565162951535312, 1.000000000000000000, 0.9510565162951535312, 1.000000000000000000, 0.9510565162951535312, 1.000000000000000000, 0.9510565162951535312, 1.000000000000000000, 0.9510565162951535312, 1.000000000000000000, 0.9510565162951535312, 1.000000000000000000, 0.9510565162951535312, 1.000000000000000000, 0.9510565162951535312, 1.000000000000000000, 0.9510565162951535312, 1.000000000000000000, 0.9510565162951535312, 1.000000000000000000, 0.9510565162951535312, 1.000000000000000000, 0.9510565162951535312, 1.000000000000000000, 0.9510565162951535312, 1.000000000000000000, 0.9510565162951535312, 1.000000000000000000, 0.9510565162951535312, 1.000000000000000000, 0.9510565162951535312, 1.000000000000000000, 0.9510565162951535312, 1.000000000000000000, 0.9510565162951535312, 1.000000000000000000, 0.9510565162951535312, 1.000000000000000000, 0.9510565162951535312, 1.000000000000000000, 0.9510565162951535312, 1.000000000000000000, 0.9510565162951535312, 1.000000000000000000, 0.9510565162951535312, 1.000000000000000000, 0.9510565162951535312, 1.000000000000000000, 0.9510565162951535312, 1.000000000000000000, 0.9510565162951535312, 1.000000000000000000, 0.9510565162951535312, 1.000000000000000000, 0.9510565162951535312, 1.000000000000000000, 0.9510565162951535312, 1.000000000000000000, 0.9510565162951535312, 1.000000000000000000, 0.9510565162951535312, 1.000000000000000000, 0.9510565162951535312, 1.000000000000000000, 0.9510565162951535312, 1.000000000000000000, 0.9510565162951535312, 1.000000000000000000, 0.9510565162951535312, 1.000000000000000000, 0.9510565162951535312, 1.000000000000000000, 0.9510565162951535312, 1.000000000000000000, 0.9510565162951535312, 1.000000000000000000, 0.9510565162951535312, 1.000000000000000000, 0.9510565162951535312, 1.000000000000000000, 0.9510565162951535312, 1.000000000000000000, 0.9510565162951535312, 1.000000000000000000, 0.9510565162951535312, 1.000000000000000000, 0.9510565162951535312, 1.000000000000000000, 0.9510565162951535312, 1.000000000000000000, 0.9510565162951535312, 1.000000000000000000, 0.9510565162951535312, 1.000000000000000000, 0.9510565162951535312, 1.000000000000000000, 0.9510565162951535312, 1.000000000000000000) ) ) 
 REPRESENTATION_ITEM ( '' )  SURFACE ( )  );
#23830 = CARTESIAN_POINT ( 'NONE',  ( 20.08610463437157279, 71.29999999999999716, -27.64615127144129758 ) ) ;
#23831 = CARTESIAN_POINT ( 'NONE',  ( -20.75514604977248112, 17.42500000273117777, 28.56700777964554661 ) ) ;
#23832 = CARTESIAN_POINT ( 'NONE',  ( -1.778240108872766143E-15, 65.50000000000000000, -32.49999999999999289 ) ) ;
#23833 = CARTESIAN_POINT ( 'NONE',  ( -26.29305231718578995, 40.20000000000001705, 19.10302069950538595 ) ) ;
#23834 = CARTESIAN_POINT ( 'NONE',  ( -14.01125832528328985, 17.58034749907602290, -24.18731323226223040 ) ) ;
#23835 = CARTESIAN_POINT ( 'NONE',  ( -26.29305231718579350, 36.30000000546239391, -19.10302069950537884 ) ) ;
#23836 = CARTESIAN_POINT ( 'NONE',  ( -19.82091636218621389, 10.94999999453763451, 14.40073868116558842 ) ) ;
#23837 = CARTESIAN_POINT ( 'NONE',  ( -27.16883889988624290, 22.92500000273117777, -19.73931689729374028 ) ) ;
#23838 = CARTESIAN_POINT ( 'NONE',  ( 24.20753774853756113, 47.95052083333331439, 13.97622843553589789 ) ) ;
#23839 = ORIENTED_EDGE ( 'NONE', *, *, #29737, .F. ) ;
#23840 = CARTESIAN_POINT ( 'NONE',  ( -27.16883889988624290, 64.92500000273119554, -19.73931689729374028 ) ) ;
#23841 = ORIENTED_EDGE ( 'NONE', *, *, #12073, .F. ) ;
#23842 = CARTESIAN_POINT ( 'NONE',  ( -28.01184896238290278, 14.86458333333333037, 7.505752307973363457 ) ) ;
#23843 = CARTESIAN_POINT ( 'NONE',  ( -28.02196122052045268, 12.86496500092397710, 7.468012846824790607 ) ) ;
#23844 = CARTESIAN_POINT ( 'NONE',  ( -10.37757302488623701, 7.525000002731194293, 31.93888565452638417 ) ) ;
#23845 = ORIENTED_EDGE ( 'NONE', *, *, #11354, .F. ) ;
#23846 = LINE ( 'NONE', #29311, #28896 ) ;
#23847 = CARTESIAN_POINT ( 'NONE',  ( 10.37757302488624056, 26.77500000273119696, -31.93888565452638417 ) ) ;
#23848 = AXIS2_PLACEMENT_3D ( 'NONE', #4653, #19473, #29923 ) ;
#23849 = CARTESIAN_POINT ( 'NONE',  ( -10.04305231718578462, 34.90000000546239534, 30.90933677959249337 ) ) ;
#23850 = CARTESIAN_POINT ( 'NONE',  ( -4.635254915624208216, 72.40000000000001990, 14.26584774442730463 ) ) ;
#23851 = CARTESIAN_POINT ( 'NONE',  ( -26.29305231718578995, 54.70000000546237828, 19.10302069950538595 ) ) ;
#23852 = CARTESIAN_POINT ( 'NONE',  ( 10.04305231718578817, 77.39999999999999147, -30.90933677959249337 ) ) ;
#23853 = CARTESIAN_POINT ( 'NONE',  ( 20.75514604977249178, 40.07500000273118701, 28.56700777964553950 ) ) ;
#23854 = CARTESIAN_POINT ( 'NONE',  ( -32.50000000000000000, 20.00000000000000355, 0.000000000000000000 ) ) ;
#23855 = CARTESIAN_POINT ( 'NONE',  ( -10.04305231718579172, 19.60000000000000497, -30.90933677959248982 ) ) ;
#23856 = CARTESIAN_POINT ( 'NONE',  ( 15.14183272437242245, 4.300000000000009592, -20.84094480462497856 ) ) ;
#23857 = EDGE_CURVE ( 'NONE', #10883, #14840, #23517, .T. ) ;
#23858 = CARTESIAN_POINT ( 'NONE',  ( -27.16883889988623935, 69.32500000273117280, 19.73931689729374739 ) ) ;
#23859 = CARTESIAN_POINT ( 'NONE',  ( 7.570916362186207671, 3.349999994537639303, 23.30088464923126779 ) ) ;
#23860 = CARTESIAN_POINT ( 'NONE',  ( -20.08610463437157989, 76.20000000546235697, -27.64615127144129758 ) ) ;
#23861 = CARTESIAN_POINT ( 'NONE',  ( -33.58253175000000113, 51.27500000273118275, -10.91162601494193041 ) ) ;
#23862 = FACE_OUTER_BOUND ( 'NONE', #27330, .T. ) ;
#23863 = CARTESIAN_POINT ( 'NONE',  ( -33.58253175000000113, 9.125000002731198379, 0.000000000000000000 ) ) ;
#23864 = CARTESIAN_POINT ( 'NONE',  ( 19.11951029504763611, 31.48475666759063074, -19.06425588902591173 ) ) ;
#23865 = CARTESIAN_POINT ( 'NONE',  ( 0.3323905815834450328, 66.99999999999998579, -33.36564663192542213 ) ) ;
#23866 = LINE ( 'NONE', #27097, #25921 ) ;
#23867 = CARTESIAN_POINT ( 'NONE',  ( -20.75514604977248112, 37.42500000273118843, 28.56700777964554661 ) ) ;
#23868 = CARTESIAN_POINT ( 'NONE',  ( -26.29305231718578995, 18.70000000546237473, 19.10302069950538595 ) ) ;
#23869 = CARTESIAN_POINT ( 'NONE',  ( 27.16883889988624290, 52.17500000273118843, 19.73931689729373673 ) ) ;
#23870 = CARTESIAN_POINT ( 'NONE',  ( -13.91746824999999532, 76.77500000273120406, -4.522059556121115875 ) ) ;
#23871 = CARTESIAN_POINT ( 'NONE',  ( 14.97647472619900455, 42.21576416574269075, -26.02091320914876960 ) ) ;
#23872 = CARTESIAN_POINT ( 'NONE',  ( -26.29305231718579350, 52.30000000546237970, -19.10302069950537884 ) ) ;
#23873 = CARTESIAN_POINT ( 'NONE',  ( -8.601468415847515203, 75.67500000273116711, 11.83890561707634959 ) ) ;
#23874 = CARTESIAN_POINT ( 'NONE',  ( 24.20753774853731244, 13.00260416666666430, -13.97622843553632599 ) ) ;
#23875 = CARTESIAN_POINT ( 'NONE',  ( 10.04305231718579705, 69.10000000546237686, 30.90933677959248982 ) ) ;
#23876 = CARTESIAN_POINT ( 'NONE',  ( 20.50609665441005092, 20.59374999999999645, 20.50609665440969209 ) ) ;
#23877 = CARTESIAN_POINT ( 'NONE',  ( -33.58253175000000113, 27.37500000273117351, 0.000000000000000000 ) ) ;
#23878 = CARTESIAN_POINT ( 'NONE',  ( 14.47279130897151944, 11.42499999726880944, -19.92008829642072598 ) ) ;
#23879 = ORIENTED_EDGE ( 'NONE', *, *, #12596, .F. ) ;
#23880 = CARTESIAN_POINT ( 'NONE',  ( 7.468012846824777284, 39.50559000092398065, 28.02196122052045268 ) ) ;
#23881 = CARTESIAN_POINT ( 'NONE',  ( -10.04305231718578462, 14.90000000546236336, 30.90933677959249337 ) ) ;
#23882 = CARTESIAN_POINT ( 'NONE',  ( -30.02300923189239512, 52.82031249999997868, 2.654126918244515359E-13 ) ) ;
#23883 = CARTESIAN_POINT ( 'NONE',  ( -15.01150461594595775, 65.99739583333334281, 26.00068869287368756 ) ) ;
#23884 = CARTESIAN_POINT ( 'NONE',  ( -27.16883889988623935, 53.57500000273118701, 19.73931689729374739 ) ) ;
#23885 = CARTESIAN_POINT ( 'NONE',  ( 10.04305231718578817, 57.90000000546238823, -30.90933677959249337 ) ) ;
#23886 = CARTESIAN_POINT ( 'NONE',  ( 13.91746824999999532, 76.47500000273120691, -4.522059556121118540 ) ) ;
#23887 = CARTESIAN_POINT ( 'NONE',  ( -33.58253175000000113, 33.22500000273117138, 10.91162601494193929 ) ) ;
#23888 = LINE ( 'NONE', #20816, #13231 ) ;
#23889 = CARTESIAN_POINT ( 'NONE',  ( 33.58253175000000113, 66.47500000273119269, -10.91162601494193751 ) ) ;
#23890 = CARTESIAN_POINT ( 'NONE',  ( 8.487781194200618273, 74.00000000000002842, 11.03901998437955534 ) ) ;
#23891 = CARTESIAN_POINT ( 'NONE',  ( -20.75514604977248823, 62.82500000273119412, -28.56700777964554305 ) ) ;
#23892 = CARTESIAN_POINT ( 'NONE',  ( -20.50609665441004736, 18.87499999999999645, -20.50609665440969565 ) ) ;
#23893 = CARTESIAN_POINT ( 'NONE',  ( -26.29305231718578995, 38.20000000000000995, 19.10302069950538595 ) ) ;
#23894 = CARTESIAN_POINT ( 'NONE',  ( -23.41746825000000243, 5.524999997268821517, -7.608796670333730638 ) ) ;
#23895 = CARTESIAN_POINT ( 'NONE',  ( 6.486482029760649416E-15, 9.875000002731187720, 35.31076352940723240 ) ) ;
#23896 = CARTESIAN_POINT ( 'NONE',  ( -32.50000000000000000, 66.40000000546238823, -10.55989012756945300 ) ) ;
#23897 = CARTESIAN_POINT ( 'NONE',  ( -6.950374756619247307, 33.47878499907601935, 26.09010956794245217 ) ) ;
#23898 = CARTESIAN_POINT ( 'NONE',  ( -11.25946833292375793, 73.57500000273120122, 8.180482586598737171 ) ) ;
#23899 = CARTESIAN_POINT ( 'NONE',  ( -33.58253175000000113, 75.27500000273118985, -10.91162601494193041 ) ) ;
#23900 = CARTESIAN_POINT ( 'NONE',  ( 11.54700538379251817, 86.00000000000001421, 19.99999999999999645 ) ) ;
#23901 = CARTESIAN_POINT ( 'NONE',  ( -20.75514604977248823, 67.07500000273118701, -28.56700777964554305 ) ) ;
#23902 = ORIENTED_EDGE ( 'NONE', *, *, #24568, .F. ) ;
#23903 = CARTESIAN_POINT ( 'NONE',  ( -18.94512977948576093, 18.32499999726880446, 13.76444248337722698 ) ) ;
#23904 = CARTESIAN_POINT ( 'NONE',  ( -19.09188309203660694, 62.70312500000000000, 19.09188309203694800 ) ) ;
#23905 = VECTOR ( 'NONE', #14261, 1000.000000000000000 ) ;
#23906 = CARTESIAN_POINT ( 'NONE',  ( -27.16883889988623935, 51.32500000273120122, 19.73931689729374739 ) ) ;
#23907 = CARTESIAN_POINT ( 'NONE',  ( -33.58253175000000113, 15.27500000273118985, -10.91162601494193218 ) ) ;
#23908 = CARTESIAN_POINT ( 'NONE',  ( -27.16883889988624290, 5.175000002731189319, -19.73931689729374028 ) ) ;
#23909 = CARTESIAN_POINT ( 'NONE',  ( -6.988114217768288228, 39.78645833333332860, -26.07999730980477437 ) ) ;
#23910 = CARTESIAN_POINT ( 'NONE',  ( -25.98046417659859486, 27.04465250092397000, -15.04653450569291628 ) ) ;
#23911 = CARTESIAN_POINT ( 'NONE',  ( 7.543491769121922985, 22.87982666574268720, 28.00173670424535644 ) ) ;
#23912 = CARTESIAN_POINT ( 'NONE',  ( -26.29305231718578995, 74.70000000546238539, 19.10302069950538595 ) ) ;
#23913 = CARTESIAN_POINT ( 'NONE',  ( 33.24513298742186862, 52.00000000000000000, -2.427281437204658943 ) ) ;
#23914 = CARTESIAN_POINT ( 'NONE',  ( -27.16883889988624290, 36.92500000273118843, -19.73931689729374028 ) ) ;
#23915 = CARTESIAN_POINT ( 'NONE',  ( -19.06425588902558133, 47.51524333240936215, 19.11951029504797006 ) ) ;
#23916 = CARTESIAN_POINT ( 'NONE',  ( 5.779280353836490358E-15, 34.49999999999998579, 32.49999999999999289 ) ) ;
#23917 = CYLINDRICAL_SURFACE ( 'NONE', #4059, 24.50000000000000000 ) ;
#23918 = EDGE_LOOP ( 'NONE', ( #17238, #4276, #5597, #18256 ) ) ;
#23919 = ADVANCED_FACE ( 'NONE', ( #4598 ), #22965, .T. ) ;
#23920 = CARTESIAN_POINT ( 'NONE',  ( -10.37757302488624411, 48.97500000273117848, -31.93888565452638417 ) ) ;
#23921 =( BOUNDED_CURVE ( )  B_SPLINE_CURVE ( 2, ( #32366, #11119, #19345, #26564, #8696, #32530, #21587, #465, #5628, #8530, #24645, #1119, #13531 ),
 .UNSPECIFIED., .F., .T. ) 
 B_SPLINE_CURVE_WITH_KNOTS ( ( 3, 2, 2, 2, 2, 2, 3 ),
 ( 0.4294871794871795156, 0.4307692307692307931, 0.4333333333333333481, 0.4358974358974359031, 0.4384615384615384581, 0.4410256410256410131, 0.4423076923076922906 ),
 .UNSPECIFIED. ) 
 CURVE ( )  GEOMETRIC_REPRESENTATION_ITEM ( )  RATIONAL_B_SPLINE_CURVE ( ( 0.9755282581475768211, 0.9755282581475772652, 1.000000000000000000, 0.9510565162951535312, 1.000000000000000000, 0.9510565162951535312, 1.000000000000000000, 0.9510565162951535312, 1.000000000000000000, 0.9510565162951535312, 1.000000000000000000, 0.9755282581475768211, 0.9755282581475768211 ) ) 
 REPRESENTATION_ITEM ( '' )  );
#23922 = CARTESIAN_POINT ( 'NONE',  ( -2.165007332552593587E-13, 51.00000000546238255, 32.50000000000000000 ) ) ;
#23923 = CARTESIAN_POINT ( 'NONE',  ( 0.04044903254993986036, 51.68006916759063785, -27.95245687107223986 ) ) ;
#23924 = CARTESIAN_POINT ( 'NONE',  ( -33.58253175000000113, 69.37500000273119838, 0.000000000000000000 ) ) ;
#23925 = ADVANCED_FACE ( 'NONE', ( #1844 ), #28282, .T. ) ;
#23926 = VERTEX_POINT ( 'NONE', #25708 ) ;
#23927 = CARTESIAN_POINT ( 'NONE',  ( 6.486482029760649416E-15, 19.62500000273116996, 35.31076352940723240 ) ) ;
#23928 = CARTESIAN_POINT ( 'NONE',  ( 7.505752307973351023, 27.75520833333332860, 28.01184896238290278 ) ) ;
#23929 = ORIENTED_EDGE ( 'NONE', *, *, #15128, .T. ) ;
#23930 = CARTESIAN_POINT ( 'NONE',  ( -1.778240108872766143E-15, 32.00000000546237544, -32.49999999999999289 ) ) ;
#23931 = CARTESIAN_POINT ( 'NONE',  ( 27.16883889988623935, 60.32500000273119412, -19.73931689729374384 ) ) ;
#23932 = CARTESIAN_POINT ( 'NONE',  ( 28.01184896238290278, 47.52083333333332860, -7.505752307973347470 ) ) ;
#23933 = CARTESIAN_POINT ( 'NONE',  ( -32.50000000000000000, 16.50000000546236834, 0.000000000000000000 ) ) ;
#23934 = CARTESIAN_POINT ( 'NONE',  ( 24.50000000000000355, 17.89999999999998437, 7.960532557706212486 ) ) ;
#23935 = CARTESIAN_POINT ( 'NONE',  ( -18.94512977948575738, 5.924999997268809437, -13.76444248337723231 ) ) ;
#23936 = CARTESIAN_POINT ( 'NONE',  ( 20.75514604977249178, 28.07500000273119412, 28.56700777964553950 ) ) ;
#23937 = CARTESIAN_POINT ( 'NONE',  ( -15.00000000000000000, 78.15000000546235981, -4.873795443493594171 ) ) ;
#23938 = CARTESIAN_POINT ( 'NONE',  ( -28.02196122052058413, 65.27565999907601224, -7.468012846824272799 ) ) ;
#23939 = LINE ( 'NONE', #408, #29475 ) ;
#23940 = CARTESIAN_POINT ( 'NONE',  ( -13.91746824999999887, 78.87500000273118417, 0.000000000000000000 ) ) ;
#23941 = CARTESIAN_POINT ( 'NONE',  ( 32.50000000000000000, 75.60000000546236265, -10.55989012756945833 ) ) ;
#23942 = CARTESIAN_POINT ( 'NONE',  ( 32.50000000000000000, 15.00000000000000000, -3.980102097228898626E-15 ) ) ;
#23943 = CARTESIAN_POINT ( 'NONE',  ( 6.988114217768294445, 62.13020833333334281, 26.07999730980477437 ) ) ;
#23944 = CARTESIAN_POINT ( 'NONE',  ( 19.82091636218621034, 19.54999999453763238, 14.40073868116559730 ) ) ;
#23945 = CARTESIAN_POINT ( 'NONE',  ( 13.91746825000000065, 73.77500000273118985, 4.522059556121114987 ) ) ;
#23946 = CARTESIAN_POINT ( 'NONE',  ( -13.97622843553588901, 28.18489583333332860, 24.20753774853756823 ) ) ;
#23947 = CARTESIAN_POINT ( 'NONE',  ( -33.58253175000000113, 25.02500000273117209, -10.91162601494193218 ) ) ;
#23948 = CARTESIAN_POINT ( 'NONE',  ( -33.58253175000000113, 75.22500000273119269, 10.91162601494193929 ) ) ;
#23949 = CARTESIAN_POINT ( 'NONE',  ( -10.37757302488624411, 34.97500000273119980, -31.93888565452638417 ) ) ;
#23950 = CARTESIAN_POINT ( 'NONE',  ( 27.16883889988623935, 18.57500000273118346, -19.73931689729374384 ) ) ;
#23951 = CARTESIAN_POINT ( 'NONE',  ( -0.04044903254992426173, 56.83631916759064495, 27.95245687107223276 ) ) ;
#23952 = CARTESIAN_POINT ( 'NONE',  ( 33.58253175000000113, 72.12500000273119838, -4.112674001490185761E-15 ) ) ;
#23953 = CARTESIAN_POINT ( 'NONE',  ( 26.29305231718578995, 3.700000005462389385, -19.10302069950538240 ) ) ;
#23954 = CARTESIAN_POINT ( 'NONE',  ( -32.50000000000000000, 53.90000000000001279, -10.55989012756945478 ) ) ;
#23955 = DIRECTION ( 'NONE',  ( -0.000000000000000000, -1.000000000000000000, -0.000000000000000000 ) ) ;
#23956 = CARTESIAN_POINT ( 'NONE',  ( 20.75514604977249178, 59.82500000273117280, 28.56700777964553950 ) ) ;
#23957 = CARTESIAN_POINT ( 'NONE',  ( -23.41746825000000598, 16.22499999726880304, 7.608796670333726198 ) ) ;
#23958 = VECTOR ( 'NONE', #14270, 1000.000000000000000 ) ;
#23959 = ADVANCED_FACE ( 'NONE', ( #25191 ), #30977, .T. ) ;
#23960 = ORIENTED_EDGE ( 'NONE', *, *, #21402, .T. ) ;
#23961 = CARTESIAN_POINT ( 'NONE',  ( -33.58253175000000113, 65.47500000273117848, 10.91162601494193929 ) ) ;
#23962 = CARTESIAN_POINT ( 'NONE',  ( 4.445600272181915325E-13, 15.49999999999999822, -32.50000000000000000 ) ) ;
#23963 = CARTESIAN_POINT ( 'NONE',  ( -14.47279130897151589, 15.82499999726881335, -19.92008829642072598 ) ) ;
#23964 = CARTESIAN_POINT ( 'NONE',  ( -19.06425588902591173, 20.31288166759063785, -19.11951029504763611 ) ) ;
#23965 = ORIENTED_EDGE ( 'NONE', *, *, #1063, .F. ) ;
#23966 = CARTESIAN_POINT ( 'NONE',  ( -33.58253175000000113, 39.22500000273119269, 10.91162601494193929 ) ) ;
#23967 = CARTESIAN_POINT ( 'NONE',  ( 5.779280353836490358E-15, 43.00000000546236834, 32.49999999999999289 ) ) ;
#23968 = EDGE_LOOP ( 'NONE', ( #3161, #17500, #3477, #3321 ) ) ;
#23969 = CARTESIAN_POINT ( 'NONE',  ( -30.02300923189239512, 45.94531249999997868, 2.654126918244515359E-13 ) ) ;
#23970 = CARTESIAN_POINT ( 'NONE',  ( 10.04305231718579705, 1.100000005462370423, 30.90933677959248982 ) ) ;
#23971 = CARTESIAN_POINT ( 'NONE',  ( -15.00000000000000000, 82.00000000000001421, 0.000000000000000000 ) ) ;
#23972 = CARTESIAN_POINT ( 'NONE',  ( -28.01184896238304134, 18.58854166666666430, -7.505752307972844761 ) ) ;
#23973 = CARTESIAN_POINT ( 'NONE',  ( -14.47279130897152122, 17.92499999726880588, 19.92008829642072243 ) ) ;
#23974 = CARTESIAN_POINT ( 'NONE',  ( -33.58253175000000113, 9.475000002731201576, 10.91162601494193929 ) ) ;
#23975 = CARTESIAN_POINT ( 'NONE',  ( -32.50000000000000000, 61.89999999999999147, -10.55989012756945478 ) ) ;
#23976 = CARTESIAN_POINT ( 'NONE',  ( -11.25946833292375793, 80.67500000273119554, -8.180482586598733619 ) ) ;
#23977 = DIRECTION ( 'NONE',  ( -0.000000000000000000, -1.000000000000000000, -0.000000000000000000 ) ) ;
#23978 = CARTESIAN_POINT ( 'NONE',  ( 20.53372385742108008, 36.34336833240934794, 20.47846945139866648 ) ) ;
#23979 = CARTESIAN_POINT ( 'NONE',  ( 11.25946833292375793, 78.17500000273119554, 8.180482586598731842 ) ) ;
#23980 = CARTESIAN_POINT ( 'NONE',  ( 20.50609665441005092, 48.09375000000000000, 20.50609665440969209 ) ) ;
#23981 = ITEM_DEFINED_TRANSFORMATION ( 'NONE', 'NONE', #19990,  #1376 ) ;
#23982 = CARTESIAN_POINT ( 'NONE',  ( -13.91746824999999887, 80.87500000273118417, 0.000000000000000000 ) ) ;
#23983 = FACE_OUTER_BOUND ( 'NONE', #1960, .T. ) ;
#23984 = CARTESIAN_POINT ( 'NONE',  ( -32.50000000000000000, 2.000000000000001776, 0.000000000000000000 ) ) ;
#23985 = CARTESIAN_POINT ( 'NONE',  ( 24.18731323226221974, 63.12722249907601224, -14.01125832528328985 ) ) ;
#23986 = CARTESIAN_POINT ( 'NONE',  ( -33.58253175000000113, 45.02500000273117564, -10.91162601494193218 ) ) ;
#23987 = CARTESIAN_POINT ( 'NONE',  ( -4.635254915624208216, 72.65000000546240244, 14.26584774442730463 ) ) ;
#23988 = CARTESIAN_POINT ( 'NONE',  ( -33.58253175000000113, 57.27500000273120406, -10.91162601494193218 ) ) ;
#23989 = CARTESIAN_POINT ( 'NONE',  ( -2.162160676586882350E-15, 32.87500000273118417, -35.31076352940722529 ) ) ;
#23990 = CARTESIAN_POINT ( 'NONE',  ( 32.50000000000000000, 25.09999999999999432, -10.55989012756945833 ) ) ;
#23991 = VECTOR ( 'NONE', #2774, 1000.000000000000000 ) ;
#23992 = CARTESIAN_POINT ( 'NONE',  ( 6.988114217767829928, 22.88541666666666430, -26.07999730980489872 ) ) ;
#23993 = DIRECTION ( 'NONE',  ( -0.000000000000000000, -1.000000000000000000, -0.000000000000000000 ) ) ;
#23994 = LINE ( 'NONE', #5961, #7439 ) ;
#23995 = CARTESIAN_POINT ( 'NONE',  ( -32.50000000000000000, 75.89999999999996305, -10.55989012756945478 ) ) ;
#23996 = CARTESIAN_POINT ( 'NONE',  ( -2.162160676586881955E-15, 10.62500000273119127, -35.31076352940723240 ) ) ;
#23997 = CARTESIAN_POINT ( 'NONE',  ( 7.236395654485755280, 4.224999997268802154, 22.27133577429736988 ) ) ;
#23998 = CARTESIAN_POINT ( 'NONE',  ( 19.82091636218621034, 9.549999994537621717, 14.40073868116559730 ) ) ;
#23999 = CARTESIAN_POINT ( 'NONE',  ( 0.04044903255044120238, 26.46055583240935505, 27.95245687107223276 ) ) ;
#24000 = DIRECTION ( 'NONE',  ( -0.000000000000000000, 1.000000000000000000, -0.000000000000000000 ) ) ;
#24001 = CARTESIAN_POINT ( 'NONE',  ( -33.58253175000000113, 17.22500000273118914, 10.91162601494193929 ) ) ;
#24002 = CARTESIAN_POINT ( 'NONE',  ( -6.988114217767819270, 48.66666666666666430, 26.07999730980490583 ) ) ;
#24003 = ORIENTED_EDGE ( 'NONE', *, *, #5812, .T. ) ;
#24004 = CARTESIAN_POINT ( 'NONE',  ( -33.58253175000000113, 61.02500000273118985, -10.91162601494193218 ) ) ;
#24005 = ORIENTED_EDGE ( 'NONE', *, *, #6826, .T. ) ;
#24006 = CARTESIAN_POINT ( 'NONE',  ( 20.50609665440969565, 16.29687499999999645, -20.50609665441004736 ) ) ;
#24007 = CARTESIAN_POINT ( 'NONE',  ( -7.543491769121417612, 19.16704833425730570, 28.00173670424549499 ) ) ;
#24008 = CARTESIAN_POINT ( 'NONE',  ( 10.37757302488624056, 6.525000002731193405, -31.93888565452638417 ) ) ;
#24009 = ORIENTED_EDGE ( 'NONE', *, *, #3707, .T. ) ;
#24010 = FACE_OUTER_BOUND ( 'NONE', #6576, .T. ) ;
#24011 = CARTESIAN_POINT ( 'NONE',  ( -27.16883889988624290, 27.17500000273118133, -19.73931689729374028 ) ) ;
#24012 = AXIS2_PLACEMENT_3D ( 'NONE', #7634, #20862, #13296 ) ;
#24013 = CARTESIAN_POINT ( 'NONE',  ( 26.29305231718579350, 37.30000000546237970, 19.10302069950537529 ) ) ;
#24014 = CARTESIAN_POINT ( 'NONE',  ( 12.13525491562420910, 73.19999999999998863, -8.816778784387098611 ) ) ;
#24015 = CARTESIAN_POINT ( 'NONE',  ( 32.50000000000000000, 33.50000000546238255, -3.980102097228898626E-15 ) ) ;
#24016 = CARTESIAN_POINT ( 'NONE',  ( 32.50000000000000000, 37.50000000546238255, -3.980102097228898626E-15 ) ) ;
#24017 = CARTESIAN_POINT ( 'NONE',  ( -27.16883889988624290, 45.17500000273119554, -19.73931689729374028 ) ) ;
#24018 =( BOUNDED_CURVE ( )  B_SPLINE_CURVE ( 2, ( #31465, #13277, #21185, #29220, #23752, #16035, #26490, #2985, #13453, #10877, #8284, #5726, #22011 ),
 .UNSPECIFIED., .F., .T. ) 
 B_SPLINE_CURVE_WITH_KNOTS ( ( 3, 2, 2, 2, 2, 2, 3 ),
 ( 0.4500000000000000111, 0.4600000000000000200, 0.4799999999999999822, 0.5000000000000000000, 0.5200000000000000178, 0.5400000000000000355, 0.5500000000000000444 ),
 .UNSPECIFIED. ) 
 CURVE ( )  GEOMETRIC_REPRESENTATION_ITEM ( )  RATIONAL_B_SPLINE_CURVE ( ( 0.9755282581475768211, 0.9755282581475768211, 1.000000000000000000, 0.9510565162951535312, 1.000000000000000000, 0.9510565162951535312, 1.000000000000000000, 0.9510565162951535312, 1.000000000000000000, 0.9510565162951535312, 1.000000000000000000, 0.9755282581475768211, 0.9755282581475768211 ) ) 
 REPRESENTATION_ITEM ( '' )  );
#24019 =( NAMED_UNIT ( * ) SI_UNIT ( $, .STERADIAN. ) SOLID_ANGLE_UNIT ( ) );
#24020 = CARTESIAN_POINT ( 'NONE',  ( -26.29305231718579350, 25.80000000000000426, -19.10302069950537884 ) ) ;
#24021 = CARTESIAN_POINT ( 'NONE',  ( -32.50000000000000000, 23.99999999999999289, 0.000000000000000000 ) ) ;
#24022 = CARTESIAN_POINT ( 'NONE',  ( 15.14183272437241889, 3.699999999999999289, 20.84094480462498211 ) ) ;
#24023 =( BOUNDED_CURVE ( )  B_SPLINE_CURVE ( 2, ( #33815, #10136, #10308, #30712, #14940, #17866, #7207, #15115, #20618, #23004, #20436, #20786, #33461 ),
 .UNSPECIFIED., .F., .T. ) 
 B_SPLINE_CURVE_WITH_KNOTS ( ( 3, 2, 2, 2, 2, 2, 3 ),
 ( 0.8055555555555555802, 0.8111111111111111160, 0.8222222222222221877, 0.8333333333333333703, 0.8444444444444444420, 0.8555555555555555136, 0.8611111111111111605 ),
 .UNSPECIFIED. ) 
 CURVE ( )  GEOMETRIC_REPRESENTATION_ITEM ( )  RATIONAL_B_SPLINE_CURVE ( ( 0.9755282581475768211, 0.9755282581475768211, 1.000000000000000000, 0.9510565162951535312, 1.000000000000000000, 0.9510565162951535312, 1.000000000000000000, 0.9510565162951535312, 1.000000000000000000, 0.9510565162951535312, 1.000000000000000000, 0.9755282581475765991, 0.9755282581475768211 ) ) 
 REPRESENTATION_ITEM ( '' )  );
#24024 = CARTESIAN_POINT ( 'NONE',  ( 10.37757302488624767, 61.72500000273117848, 31.93888565452638417 ) ) ;
#24025 = CARTESIAN_POINT ( 'NONE',  ( -33.37605761044780905, 67.00000000000000000, -0.2721180500505538391 ) ) ;
#24026 = CARTESIAN_POINT ( 'NONE',  ( 5.389190825954574215, 74.00000000000005684, -13.31942880713982724 ) ) ;
#24027 = CARTESIAN_POINT ( 'NONE',  ( -2.162160676586882350E-15, 50.87500000273119838, -35.31076352940722529 ) ) ;
#24028 = CARTESIAN_POINT ( 'NONE',  ( -23.41746824999999887, 5.524999997268821517, -7.608796670333730638 ) ) ;
#24029 = CARTESIAN_POINT ( 'NONE',  ( -15.14183272437242067, 8.700000000000017053, -20.84094480462497856 ) ) ;
#24030 = CARTESIAN_POINT ( 'NONE',  ( 33.58253175000000823, 6.025000002731191628, 10.91162601494192863 ) ) ;
#24031 = CARTESIAN_POINT ( 'NONE',  ( -26.06988505166735237, 33.77642333425730214, -7.025853678916388567 ) ) ;
#24032 = CARTESIAN_POINT ( 'NONE',  ( 10.04305231718578817, 25.90000000546238823, -30.90933677959249337 ) ) ;
#24033 = CARTESIAN_POINT ( 'NONE',  ( -1.683996601885078048, 52.00000000000000000, 33.30202823065787499 ) ) ;
#24034 = UNCERTAINTY_MEASURE_WITH_UNIT (LENGTH_MEASURE( 1.000000000000000082E-05 ), #19868, 'distance_accuracy_value', 'NONE');
#24035 = CARTESIAN_POINT ( 'NONE',  ( -10.37757302488623701, 31.52500000273118630, 31.93888565452638417 ) ) ;
#24036 = CARTESIAN_POINT ( 'NONE',  ( 5.147494310547426899, 65.44874571845315359, -32.50000000000000000 ) ) ;
#24037 = CARTESIAN_POINT ( 'NONE',  ( -1.778240108872766143E-15, 58.00000000546237544, -32.49999999999999289 ) ) ;
#24038 = CARTESIAN_POINT ( 'NONE',  ( 13.91746824999999532, 79.97500000273115006, -4.522059556121118540 ) ) ;
#24039 = CARTESIAN_POINT ( 'NONE',  ( 26.02091320914876960, 46.51263916574269786, 14.97647472619900455 ) ) ;
#24040 = CARTESIAN_POINT ( 'NONE',  ( 32.50000000000000711, 53.40000000546238823, 10.55989012756945122 ) ) ;
#24041 = CARTESIAN_POINT ( 'NONE',  ( 32.50000000000000000, 48.99999999999998579, -3.980102097228898626E-15 ) ) ;
#24042 = SURFACE_STYLE_USAGE ( .BOTH. , #10487 ) ;
#24043 = CARTESIAN_POINT ( 'NONE',  ( -26.07999730980477437, 18.30208333333332860, 6.988114217768305103 ) ) ;
#24044 = CARTESIAN_POINT ( 'NONE',  ( 6.277390505771533514E-15, 71.00000000546235412, 34.17252228774368916 ) ) ;
#24045 = CARTESIAN_POINT ( 'NONE',  ( 2.740863092043355209E-13, 17.58593749999999645, 30.02300923189239512 ) ) ;
#24046 = CARTESIAN_POINT ( 'NONE',  ( 18.94512977948575738, 14.92499999726881654, 13.76444248337723408 ) ) ;
#24047 = ORIENTED_EDGE ( 'NONE', *, *, #4410, .T. ) ;
#24048 = CARTESIAN_POINT ( 'NONE',  ( -25.98046417659859486, 37.35715250092397355, -15.04653450569291628 ) ) ;
#24049 = CARTESIAN_POINT ( 'NONE',  ( 20.08610463437158344, 19.20000000546236052, 27.64615127144129403 ) ) ;
#24050 = EDGE_CURVE ( 'NONE', #3462, #2966, #30502, .T. ) ;
#24051 = CARTESIAN_POINT ( 'NONE',  ( 30.02300923189239512, 51.10156249999998579, -2.619432448724977703E-13 ) ) ;
#24052 = CARTESIAN_POINT ( 'NONE',  ( 0.000000000000000000, 80.00000000000001421, 0.000000000000000000 ) ) ;
#24053 = CARTESIAN_POINT ( 'NONE',  ( 20.75514604977248467, 50.67500000273117422, -28.56700777964554305 ) ) ;
#24054 = CARTESIAN_POINT ( 'NONE',  ( -20.08610463437156923, 58.80000000546239391, 27.64615127144130113 ) ) ;
#24055 = CARTESIAN_POINT ( 'NONE',  ( -13.91746824999999887, 79.37500000273118417, 0.000000000000000000 ) ) ;
#24056 = CARTESIAN_POINT ( 'NONE',  ( 33.58253175000000823, 38.02500000273117564, 10.91162601494192863 ) ) ;
#24057 = CARTESIAN_POINT ( 'NONE',  ( 5.147494310547426899, 55.44874571845315359, -32.50000000000000000 ) ) ;
#24058 = CARTESIAN_POINT ( 'NONE',  ( -33.58253175000000113, 59.47500000273118559, 10.91162601494193929 ) ) ;
#24059 = CARTESIAN_POINT ( 'NONE',  ( 13.82924054492543853, 74.00000000000001421, -1.809887360631980524 ) ) ;
#24060 = EDGE_CURVE ( 'NONE', #28296, #21102, #25365, .T. ) ;
#24061 = CARTESIAN_POINT ( 'NONE',  ( 33.58253175000000823, 58.02500000273117564, 10.91162601494192685 ) ) ;
#24062 = ADVANCED_FACE ( 'NONE', ( #13351 ), #13011, .T. ) ;
#24063 = CARTESIAN_POINT ( 'NONE',  ( 7.505752307973351023, 17.44270833333333215, 28.01184896238290278 ) ) ;
#24064 = CARTESIAN_POINT ( 'NONE',  ( -32.50000000000000000, 40.00000000000000711, 0.000000000000000000 ) ) ;
#24065 = CARTESIAN_POINT ( 'NONE',  ( 23.41746825000000243, 6.724999997268811924, -7.608796670333727974 ) ) ;
#24066 = CARTESIAN_POINT ( 'NONE',  ( 10.37757302488624056, 4.775000002731177418, -31.93888565452638417 ) ) ;
#24067 = CARTESIAN_POINT ( 'NONE',  ( 5.147494310547426899, 35.94874572391554324, -32.50000000000000000 ) ) ;
#24068 = DIRECTION ( 'NONE',  ( 1.224646799147353454E-16, -1.000000000000000000, 0.000000000000000000 ) ) ;
#24069 = CARTESIAN_POINT ( 'NONE',  ( -33.58253175000000113, 71.27500000273118985, -10.91162601494193041 ) ) ;
#24070 = CARTESIAN_POINT ( 'NONE',  ( -15.14183272437242778, 19.04999999453762172, 20.84094480462497856 ) ) ;
#24071 = ADVANCED_FACE ( 'NONE', ( #2367 ), #13454, .T. ) ;
#24072 = CARTESIAN_POINT ( 'NONE',  ( -33.58253175000000113, 69.27500000273116143, -10.91162601494193218 ) ) ;
#24073 = VERTEX_POINT ( 'NONE', #23825 ) ;
#24074 = DIRECTION ( 'NONE',  ( -0.000000000000000000, -1.000000000000000000, -0.000000000000000000 ) ) ;
#24075 = CARTESIAN_POINT ( 'NONE',  ( -24.20753774853730889, 55.97135416666665719, 13.97622843553633842 ) ) ;
#24076 = CARTESIAN_POINT ( 'NONE',  ( 33.58253175000000113, 52.12500000273119838, -4.112674001490185761E-15 ) ) ;
#24077 = CARTESIAN_POINT ( 'NONE',  ( 33.58253175000000113, 10.37500000273118594, -4.112674001490185761E-15 ) ) ;
#24078 = CARTESIAN_POINT ( 'NONE',  ( 6.486482029760649416E-15, 3.875000002731187720, 35.31076352940723240 ) ) ;
#24079 = CARTESIAN_POINT ( 'NONE',  ( 27.95245687107223276, 37.35156249999999289, -2.463307335887066074E-13 ) ) ;
#24080 = CARTESIAN_POINT ( 'NONE',  ( -15.04653450569291984, 29.62277750092397355, 25.98046417659859486 ) ) ;
#24081 = CARTESIAN_POINT ( 'NONE',  ( 15.04653450569339945, 15.86159749907602112, 25.98046417659831775 ) ) ;
#24082 = CARTESIAN_POINT ( 'NONE',  ( -10.04305231718578462, 72.90000000546238823, 30.90933677959249337 ) ) ;
#24083 = CARTESIAN_POINT ( 'NONE',  ( 13.91746825000000065, 79.77500000273116143, 4.522059556121114987 ) ) ;
#24084 = CARTESIAN_POINT ( 'NONE',  ( 10.37757302488624767, 37.72500000273118559, 31.93888565452638417 ) ) ;
#24085 = CARTESIAN_POINT ( 'NONE',  ( -7.025853678916861966, 45.22357666574267654, -26.06988505166722803 ) ) ;
#24086 = CARTESIAN_POINT ( 'NONE',  ( 23.41746825000000243, 12.52499999726880375, 7.608796670333735079 ) ) ;
#24087 = DIRECTION ( 'NONE',  ( 0.000000000000000000, 0.000000000000000000, 1.000000000000000000 ) ) ;
#24088 = ORIENTED_EDGE ( 'NONE', *, *, #4457, .F. ) ;
#24089 = CARTESIAN_POINT ( 'NONE',  ( -33.58253175000000113, 45.37500000273119127, 0.000000000000000000 ) ) ;
#24090 = CARTESIAN_POINT ( 'NONE',  ( -20.08610463437156923, 50.80000000546237970, 27.64615127144130113 ) ) ;
#24091 = CARTESIAN_POINT ( 'NONE',  ( -6.950374756619716266, 54.97434000092398065, -26.09010956794232428 ) ) ;
#24092 = CARTESIAN_POINT ( 'NONE',  ( -33.58253175000000113, 71.47500000273119269, 10.91162601494193929 ) ) ;
#24093 = VERTEX_POINT ( 'NONE', #15421 ) ;
#24094 = CARTESIAN_POINT ( 'NONE',  ( 33.58253175000000823, 20.02500000273118275, 10.91162601494192863 ) ) ;
#24095 = CARTESIAN_POINT ( 'NONE',  ( -26.00068869287368756, 22.16927083333332504, -15.01150461594595775 ) ) ;
#24096 = ORIENTED_EDGE ( 'NONE', *, *, #8182, .T. ) ;
#24097 = CARTESIAN_POINT ( 'NONE',  ( -32.50000000000000000, 48.40000000546237402, -10.55989012756945300 ) ) ;
#24098 = CARTESIAN_POINT ( 'NONE',  ( -20.75514604977248823, 52.82500000273116569, -28.56700777964554305 ) ) ;
#24099 = CARTESIAN_POINT ( 'NONE',  ( -30.02300923189239512, 45.94531249999997868, 2.654126918244515359E-13 ) ) ;
#24100 = CARTESIAN_POINT ( 'NONE',  ( 32.50000000000000000, 19.60000000546237686, -10.55989012756945833 ) ) ;
#24101 = DIRECTION ( 'NONE',  ( -1.000000000000000000, 0.000000000000000000, 0.000000000000000000 ) ) ;
#24102 = CARTESIAN_POINT ( 'NONE',  ( 7.236395654485760609, 9.524999997268801977, -22.27133577429736633 ) ) ;
#24103 = CARTESIAN_POINT ( 'NONE',  ( -33.58253175000000113, 27.27500000273119340, -10.91162601494193218 ) ) ;
#24104 = DIRECTION ( 'NONE',  ( 0.000000000000000000, 0.000000000000000000, 1.000000000000000000 ) ) ;
#24105 = CARTESIAN_POINT ( 'NONE',  ( -0.04044903255044120238, 65.99180583240935505, -30.02300923189239867 ) ) ;
#24106 = CARTESIAN_POINT ( 'NONE',  ( 4.300734207923757602, 80.27500000273118985, -13.23629886949340673 ) ) ;
#24107 = CARTESIAN_POINT ( 'NONE',  ( 26.29305231718579350, 8.800000000000002487, 19.10302069950537529 ) ) ;
#24108 = CARTESIAN_POINT ( 'NONE',  ( 26.29305231718578995, 7.199999999999998401, -19.10302069950538240 ) ) ;
#24109 = CARTESIAN_POINT ( 'NONE',  ( -26.07999730980490583, 63.27604166666667140, -6.988114217767815717 ) ) ;
#24110 = CARTESIAN_POINT ( 'NONE',  ( 24.50000000000000000, 17.74999999453763522, 0.000000000000000000 ) ) ;
#24111 = CARTESIAN_POINT ( 'NONE',  ( 13.91746824999999532, 77.97500000273119269, -4.522059556121118540 ) ) ;
#24112 = CARTESIAN_POINT ( 'NONE',  ( -26.07999730980490583, 28.90104166666666785, -6.988114217767815717 ) ) ;
#24113 = EDGE_CURVE ( 'NONE', #16121, #21853, #10985, .T. ) ;
#24114 = CARTESIAN_POINT ( 'NONE',  ( -33.58253175000000113, 25.12500000273118417, 0.000000000000000000 ) ) ;
#24115 = CARTESIAN_POINT ( 'NONE',  ( 33.58253175000000113, 74.22500000273119269, -10.91162601494193751 ) ) ;
#24116 = CARTESIAN_POINT ( 'NONE',  ( -20.75514604977248112, 31.67500000273119909, 28.56700777964554661 ) ) ;
#24117 = CARTESIAN_POINT ( 'NONE',  ( 6.486482029760648627E-15, 17.87500000273119838, 35.31076352940722529 ) ) ;
#24118 = CARTESIAN_POINT ( 'NONE',  ( 26.09010956794232428, 55.83371500092398065, -6.950374756619718042 ) ) ;
#24119 = CARTESIAN_POINT ( 'NONE',  ( 10.37757302488624767, 71.72500000273119269, 31.93888565452638417 ) ) ;
#24120 = DIRECTION ( 'NONE',  ( -0.000000000000000000, -1.000000000000000000, -0.000000000000000000 ) ) ;
#24121 =( BOUNDED_CURVE ( )  B_SPLINE_CURVE ( 2, ( #3829, #30756, #30067, #22361, #20305, #6573, #32808, #27, #15680, #7766, #10181, #23394, #5364 ),
 .UNSPECIFIED., .F., .T. ) 
 B_SPLINE_CURVE_WITH_KNOTS ( ( 3, 2, 2, 2, 2, 2, 3 ),
 ( 0.4500000000000000111, 0.4600000000000000200, 0.4799999999999999822, 0.5000000000000000000, 0.5200000000000000178, 0.5400000000000000355, 0.5500000000000000444 ),
 .UNSPECIFIED. ) 
 CURVE ( )  GEOMETRIC_REPRESENTATION_ITEM ( )  RATIONAL_B_SPLINE_CURVE ( ( 0.9755282581475768211, 0.9755282581475768211, 1.000000000000000000, 0.9510565162951535312, 1.000000000000000000, 0.9510565162951535312, 1.000000000000000000, 0.9510565162951535312, 1.000000000000000000, 0.9510565162951535312, 1.000000000000000000, 0.9755282581475768211, 0.9755282581475768211 ) ) 
 REPRESENTATION_ITEM ( '' )  );
#24122 = CARTESIAN_POINT ( 'NONE',  ( 32.50000000000000000, 55.09999999999998010, -10.55989012756945833 ) ) ;
#24123 = LINE ( 'NONE', #8491, #14455 ) ;
#24124 = CARTESIAN_POINT ( 'NONE',  ( 20.75514604977248467, 60.42500000273118133, -28.56700777964554305 ) ) ;
#24125 = CARTESIAN_POINT ( 'NONE',  ( 23.41746824999999887, 15.12499999726882294, 0.000000000000000000 ) ) ;
#24126 = VERTEX_POINT ( 'NONE', #115 ) ;
#24127 = CARTESIAN_POINT ( 'NONE',  ( -20.75514604977248112, 67.67500000273116711, 28.56700777964554661 ) ) ;
#24128 = CARTESIAN_POINT ( 'NONE',  ( -20.08610463437157989, 15.69999999999999929, -27.64615127144129758 ) ) ;
#24129 = CARTESIAN_POINT ( 'NONE',  ( 7.236395654485760609, 9.024999997268800200, -22.27133577429736633 ) ) ;
#24130 = CARTESIAN_POINT ( 'NONE',  ( 0.04044903254993986036, 20.74256916759064495, -27.95245687107223986 ) ) ;
#24131 = ORIENTED_EDGE ( 'NONE', *, *, #22463, .F. ) ;
#24132 = CARTESIAN_POINT ( 'NONE',  ( -20.75514604977248823, 34.82500000273118701, -28.56700777964554305 ) ) ;
#24133 = CARTESIAN_POINT ( 'NONE',  ( -6.668400408272875007E-16, 0.5000000000000068834, -24.50000000000000355 ) ) ;
#24134 = ORIENTED_EDGE ( 'NONE', *, *, #30700, .T. ) ;
#24135 = CARTESIAN_POINT ( 'NONE',  ( 28.01184896238290278, 54.39583333333332860, -7.505752307973347470 ) ) ;
#24136 = CARTESIAN_POINT ( 'NONE',  ( 32.50000000000000000, 5.099999999999983658, -10.55989012756945833 ) ) ;
#24137 = CARTESIAN_POINT ( 'NONE',  ( -3.880418787951142701, 3.448745718453164244, 24.49999999999999645 ) ) ;
#24138 = CARTESIAN_POINT ( 'NONE',  ( 20.75514604977249178, 71.82500000273118701, 28.56700777964553950 ) ) ;
#24139 = CARTESIAN_POINT ( 'NONE',  ( 15.01150461594643204, 20.73697916666666075, 26.00068869287340334 ) ) ;
#24140 = CARTESIAN_POINT ( 'NONE',  ( -24.50000000000000000, 9.000000000000007105, -3.000384657911015469E-15 ) ) ;
#24141 = CARTESIAN_POINT ( 'NONE',  ( -20.75514604977248112, 9.675000002731193760, 28.56700777964554661 ) ) ;
#24142 = CARTESIAN_POINT ( 'NONE',  ( -10.37757302488624411, 24.72500000273119980, -31.93888565452638417 ) ) ;
#24143 = CARTESIAN_POINT ( 'NONE',  ( 8.601468415847516980, 78.17500000273118133, -11.83890561707634603 ) ) ;
#24144 = CARTESIAN_POINT ( 'NONE',  ( 12.13525491562421088, 77.05000000546242234, 8.816778784387095058 ) ) ;
#24145 = CARTESIAN_POINT ( 'NONE',  ( -20.47846945139866648, 33.76524333240934084, 20.53372385742108008 ) ) ;
#24146 = CARTESIAN_POINT ( 'NONE',  ( -4.300734207923759378, 78.97500000273119269, -13.23629886949340495 ) ) ;
#24147 = CARTESIAN_POINT ( 'NONE',  ( 20.50609665441005092, 44.65624999999999289, 20.50609665440969209 ) ) ;
#24148 = CARTESIAN_POINT ( 'NONE',  ( -24.50000000000000000, 11.00000000000001066, -3.000384657911015469E-15 ) ) ;
#24149 = CARTESIAN_POINT ( 'NONE',  ( -20.08610463437156923, 38.80000000546237260, 27.64615127144130113 ) ) ;
#24150 = CARTESIAN_POINT ( 'NONE',  ( -27.95245687107223986, 61.69493083240936926, 0.04044903255043252877 ) ) ;
#24151 = CARTESIAN_POINT ( 'NONE',  ( -33.58253175000000113, 41.12500000273119838, 0.000000000000000000 ) ) ;
#24152 = CARTESIAN_POINT ( 'NONE',  ( -4.635254915624208216, 70.65000000546240244, 14.26584774442730463 ) ) ;
#24153 = CARTESIAN_POINT ( 'NONE',  ( -10.37757302488624411, 54.97500000273118559, -31.93888565452638417 ) ) ;
#24154 = CARTESIAN_POINT ( 'NONE',  ( 20.75514604977248467, 36.67500000273118843, -28.56700777964554305 ) ) ;
#24155 = DIRECTION ( 'NONE',  ( 0.000000000000000000, 1.000000000000000000, 0.000000000000000000 ) ) ;
#24156 = ADVANCED_FACE ( 'NONE', ( #23314 ), #33779, .T. ) ;
#24157 = CARTESIAN_POINT ( 'NONE',  ( -13.97622843553588901, 17.87239583333332860, 24.20753774853756823 ) ) ;
#24158 = CARTESIAN_POINT ( 'NONE',  ( 15.14183272437242067, 11.44999999453763095, 20.84094480462498211 ) ) ;
#24159 = CARTESIAN_POINT ( 'NONE',  ( -11.54700538379251817, 86.00000000000001421, 19.99999999999999645 ) ) ;
#24160 = CARTESIAN_POINT ( 'NONE',  ( -26.29305231718579350, 71.80000000000001137, -19.10302069950537884 ) ) ;
#24161 = CARTESIAN_POINT ( 'NONE',  ( 33.58253175000000113, 10.12500000273118594, -4.112674001490185761E-15 ) ) ;
#24162 = CARTESIAN_POINT ( 'NONE',  ( 18.94512977948575738, 2.424999997268806329, 13.76444248337723408 ) ) ;
#24163 = CARTESIAN_POINT ( 'NONE',  ( 12.11000150615022264, -45.00000000000001421, 0.000000000000000000 ) ) ;
#24164 = CARTESIAN_POINT ( 'NONE',  ( -13.94119854578892514, 26.74701416574268720, 24.22776226481266448 ) ) ;
#24165 = CARTESIAN_POINT ( 'NONE',  ( -26.29305231718578995, 60.20000000000000284, 19.10302069950538595 ) ) ;
#24166 = CARTESIAN_POINT ( 'NONE',  ( -10.37757302488624411, 20.72500000273119625, -31.93888565452638417 ) ) ;
#24167 = CARTESIAN_POINT ( 'NONE',  ( 6.988114217768294445, 55.25520833333333570, 26.07999730980477437 ) ) ;
#24168 = ORIENTED_EDGE ( 'NONE', *, *, #16412, .F. ) ;
#24169 = CARTESIAN_POINT ( 'NONE',  ( 33.58253175000000823, 58.02500000273117564, 10.91162601494192863 ) ) ;
#24170 = EDGE_LOOP ( 'NONE', ( #32795, #14290, #17541, #3336 ) ) ;
#24171 = CARTESIAN_POINT ( 'NONE',  ( -2.584737979205441561E-13, 22.74218749999999645, -30.02300923189239512 ) ) ;
#24172 = CARTESIAN_POINT ( 'NONE',  ( -15.04653450569291984, 19.31027750092397710, 25.98046417659859486 ) ) ;
#24173 = AXIS2_PLACEMENT_3D ( 'NONE', #32018, #19000, #8682 ) ;
#24174 = CARTESIAN_POINT ( 'NONE',  ( 27.16883889988624290, 1.925000002731186433, 19.73931689729373673 ) ) ;
#24175 = ORIENTED_EDGE ( 'NONE', *, *, #26197, .F. ) ;
#24176 = DIRECTION ( 'NONE',  ( -1.000000000000000000, -1.224646799147353454E-16, 0.000000000000000000 ) ) ;
#24177 = CARTESIAN_POINT ( 'NONE',  ( 20.75514604977249178, 28.07500000273119412, 28.56700777964553950 ) ) ;
#24178 = CARTESIAN_POINT ( 'NONE',  ( 26.29305231718578995, 29.70000000546238539, -19.10302069950538240 ) ) ;
#24179 = CARTESIAN_POINT ( 'NONE',  ( 10.04305231718578817, 79.39999999999999147, -30.90933677959249337 ) ) ;
#24180 = CARTESIAN_POINT ( 'NONE',  ( 6.054684311146244891E-15, -72.44024934668307480, 0.000000000000000000 ) ) ;
#24181 = CARTESIAN_POINT ( 'NONE',  ( -3.880418787951104953, 11.44874571845314293, 24.50000000000000711 ) ) ;
#24182 = CARTESIAN_POINT ( 'NONE',  ( -33.58253175000000113, 45.47500000273119980, 10.91162601494193929 ) ) ;
#24183 = CARTESIAN_POINT ( 'NONE',  ( -20.08610463437157989, 25.70000000000000284, -27.64615127144129758 ) ) ;
#24184 = CARTESIAN_POINT ( 'NONE',  ( 32.50000000000000000, 18.99999999999998934, -3.980102097228898626E-15 ) ) ;
#24185 = AXIS2_PLACEMENT_3D ( 'NONE', #9806, #15135, #7573 ) ;
#24186 = CARTESIAN_POINT ( 'NONE',  ( -24.50000000000000000, 13.00000000000001066, -3.000384657911015469E-15 ) ) ;
#24187 = CARTESIAN_POINT ( 'NONE',  ( -33.58253175000000113, 63.22500000273119269, 10.91162601494193929 ) ) ;
#24188 = CARTESIAN_POINT ( 'NONE',  ( -24.50000000000001066, 6.849999994537628645, 7.960532557706201828 ) ) ;
#24189 = CARTESIAN_POINT ( 'NONE',  ( 27.16883889988624290, 56.17500000273118133, 19.73931689729373673 ) ) ;
#24190 = CARTESIAN_POINT ( 'NONE',  ( -7.236395654485757944, 7.224999997268804819, -22.27133577429736988 ) ) ;
#24191 = CARTESIAN_POINT ( 'NONE',  ( 3.880418787951134707, 9.551254281546839309, 24.50000000000000000 ) ) ;
#24192 = CARTESIAN_POINT ( 'NONE',  ( -33.58253175000000113, 7.125000002731196602, 0.000000000000000000 ) ) ;
#24193 = ADVANCED_FACE ( 'NONE', ( #15936 ), #18683, .F. ) ;
#24194 = EDGE_CURVE ( 'NONE', #27363, #19688, #3556, .T. ) ;
#24195 = CARTESIAN_POINT ( 'NONE',  ( 14.01125832528286352, 38.21652750092398065, -24.18731323226246843 ) ) ;
#24196 = CARTESIAN_POINT ( 'NONE',  ( 23.22858344560803445, 16.99999999999999289, -3.065087378623344794 ) ) ;
#24197 = CARTESIAN_POINT ( 'NONE',  ( -20.08610463437157989, 19.69999999999998863, -27.64615127144129758 ) ) ;
#24198 = CARTESIAN_POINT ( 'NONE',  ( 10.37757302488624056, 26.52500000273118275, -31.93888565452638417 ) ) ;
#24199 = CIRCLE ( 'NONE', #18185, 10.11607355459420177 ) ;
#24201 = AXIS2_PLACEMENT_3D ( 'NONE', #30866, #265, #12342 ) ;
#24200 = CARTESIAN_POINT ( 'NONE',  ( 5.147494310547380714, 64.55125428154684641, 32.50000000000002132 ) ) ;
#24202 = CARTESIAN_POINT ( 'NONE',  ( 5.779280353836490358E-15, 61.00000000546238255, 32.49999999999999289 ) ) ;
#24203 = CARTESIAN_POINT ( 'NONE',  ( -30.02300923189239867, 58.25743083240935505, 0.04044903255044988294 ) ) ;
#24204 = CARTESIAN_POINT ( 'NONE',  ( 20.08610463437158344, 49.20000000546237828, 27.64615127144129403 ) ) ;
#24205 = LINE ( 'NONE', #6167, #699 ) ;
#24206 = CARTESIAN_POINT ( 'NONE',  ( 26.07999730980490227, 27.18229166666666430, 6.988114217767821046 ) ) ;
#24207 = ORIENTED_EDGE ( 'NONE', *, *, #2759, .F. ) ;
#24208 = CARTESIAN_POINT ( 'NONE',  ( 6.486482029760649416E-15, 73.62500000273118417, 35.31076352940723240 ) ) ;
#24209 = CARTESIAN_POINT ( 'NONE',  ( -15.01150461594595775, 28.18489583333332860, 26.00068869287368756 ) ) ;
#24210 = EDGE_CURVE ( 'NONE', #6224, #15184, #16109, .T. ) ;
#24211 = DIRECTION ( 'NONE',  ( -0.000000000000000000, -1.000000000000000000, -0.000000000000000000 ) ) ;
#24212 = ORIENTED_EDGE ( 'NONE', *, *, #27904, .F. ) ;
#24213 = CARTESIAN_POINT ( 'NONE',  ( 7.543491769121427382, 41.51079833425730214, -28.00173670424548433 ) ) ;
#24214 = CARTESIAN_POINT ( 'NONE',  ( 26.29305231718579350, 17.30000000546237615, 19.10302069950537529 ) ) ;
#24215 =( BOUNDED_CURVE ( )  B_SPLINE_CURVE ( 2, ( #6684, #1183, #12001, #14084, #22146, #32423, #19904, #30353, #6855, #8920, #24382, #27286, #11335 ),
 .UNSPECIFIED., .F., .F. ) 
 B_SPLINE_CURVE_WITH_KNOTS ( ( 3, 2, 2, 2, 2, 2, 3 ),
 ( 0.1730769230769230727, 0.1743589743589743501, 0.1769230769230769329, 0.1794871794871794879, 0.1820512820512820429, 0.1846153846153846256, 0.1858974358974359031 ),
 .UNSPECIFIED. ) 
 CURVE ( )  GEOMETRIC_REPRESENTATION_ITEM ( )  RATIONAL_B_SPLINE_CURVE ( ( 0.9755282581475768211, 0.9755282581475768211, 1.000000000000000000, 0.9510565162951535312, 1.000000000000000000, 0.9510565162951535312, 1.000000000000000000, 0.9510565162951535312, 1.000000000000000000, 0.9510565162951535312, 1.000000000000000000, 0.9755282581475768211, 0.9755282581475768211 ) ) 
 REPRESENTATION_ITEM ( '' )  );
#24216 = CARTESIAN_POINT ( 'NONE',  ( 20.50609665440969565, 50.67187500000000000, -20.50609665441004736 ) ) ;
#24217 = CARTESIAN_POINT ( 'NONE',  ( -1.778240108872766143E-15, 21.50000000000000000, -32.49999999999999289 ) ) ;
#24218 = CARTESIAN_POINT ( 'NONE',  ( -2.162160676586881955E-15, 44.87500000273119127, -35.31076352940723240 ) ) ;
#24219 = CARTESIAN_POINT ( 'NONE',  ( -10.04305231718578462, 48.90000000546238113, 30.90933677959249337 ) ) ;
#24220 = CARTESIAN_POINT ( 'NONE',  ( -8.601468415847515203, 79.67500000273115290, 11.83890561707634959 ) ) ;
#24221 = CARTESIAN_POINT ( 'NONE',  ( 10.37757302488624056, 38.52500000273118275, -31.93888565452638417 ) ) ;
#24222 = DIRECTION ( 'NONE',  ( 0.000000000000000000, 0.000000000000000000, 1.000000000000000000 ) ) ;
#24223 = STYLED_ITEM ( 'NONE', ( #33542 ), #9431 ) ;
#24224 = CARTESIAN_POINT ( 'NONE',  ( -10.37757302488624411, 64.97500000273120691, -31.93888565452638417 ) ) ;
#24225 = CARTESIAN_POINT ( 'NONE',  ( 5.348221797398307942, 74.00000000000001421, 12.84883053416113974 ) ) ;
#24226 = CARTESIAN_POINT ( 'NONE',  ( -32.50000000000000000, 42.09999999999997300, 10.55989012756946366 ) ) ;
#24227 = CARTESIAN_POINT ( 'NONE',  ( -14.47279130897151589, 13.32499999726880624, -19.92008829642072598 ) ) ;
#24228 = CARTESIAN_POINT ( 'NONE',  ( -10.37757302488623701, 5.775000002731179194, 31.93888565452638417 ) ) ;
#24229 = DIRECTION ( 'NONE',  ( 1.224646799147353454E-16, -1.000000000000000000, 0.000000000000000000 ) ) ;
#24230 = CARTESIAN_POINT ( 'NONE',  ( 4.300734207923757602, 74.77500000273118985, -13.23629886949340673 ) ) ;
#24231 = CARTESIAN_POINT ( 'NONE',  ( -33.58253175000000113, 75.47500000273116427, 10.91162601494193929 ) ) ;
#24232 = CARTESIAN_POINT ( 'NONE',  ( -40.00000000000000711, 52.00000000000000711, -23.09401076758504345 ) ) ;
#24233 = CARTESIAN_POINT ( 'NONE',  ( -20.75514604977248823, 69.07500000273115859, -28.56700777964554305 ) ) ;
#24234 = ORIENTED_EDGE ( 'NONE', *, *, #4893, .F. ) ;
#24235 = DIRECTION ( 'NONE',  ( 0.000000000000000000, 0.000000000000000000, -1.000000000000000000 ) ) ;
#24236 = CARTESIAN_POINT ( 'NONE',  ( 13.97622843553633665, 65.42447916666667140, 24.20753774853730889 ) ) ;
#24237 = CARTESIAN_POINT ( 'NONE',  ( -12.11607355459419644, -70.99969134886156041, 0.000000000000000000 ) ) ;
#24238 = CARTESIAN_POINT ( 'NONE',  ( 20.75514604977248467, 44.42500000273120264, -28.56700777964554305 ) ) ;
#24239 = CARTESIAN_POINT ( 'NONE',  ( 10.37757302488624767, 13.97500000273120513, 31.93888565452638417 ) ) ;
#24240 = CARTESIAN_POINT ( 'NONE',  ( -33.58253175000000113, 61.37500000273120548, 0.000000000000000000 ) ) ;
#24241 = CARTESIAN_POINT ( 'NONE',  ( -24.20753774853756823, 53.10677083333332149, -13.97622843553588723 ) ) ;
#24242 = CARTESIAN_POINT ( 'NONE',  ( -20.47846945139902175, 30.62538166759064495, -20.53372385742072481 ) ) ;
#24243 = CARTESIAN_POINT ( 'NONE',  ( 26.02091320914876960, 25.88763916574269075, 14.97647472619900455 ) ) ;
#24244 = CARTESIAN_POINT ( 'NONE',  ( 32.50000000000000000, 71.50000000546236834, -3.980102097228898626E-15 ) ) ;
#24245 = CARTESIAN_POINT ( 'NONE',  ( -8.601468415847518756, 76.57500000273120122, -11.83890561707634781 ) ) ;
#24246 = CARTESIAN_POINT ( 'NONE',  ( -10.37757302488624411, 40.72500000273118559, -31.93888565452638417 ) ) ;
#24247 = CARTESIAN_POINT ( 'NONE',  ( -14.01125832528328985, 45.08034749907603356, -24.18731323226223040 ) ) ;
#24248 = CARTESIAN_POINT ( 'NONE',  ( -23.41746825000000243, 13.52499999726880198, -7.608796670333730638 ) ) ;
#24249 = EDGE_CURVE ( 'NONE', #5592, #5684, #26560, .T. ) ;
#24250 = CARTESIAN_POINT ( 'NONE',  ( -4.223320258572819786E-15, 5.249999994537622783, 24.50000000000000000 ) ) ;
#24251 = VERTEX_POINT ( 'NONE', #21420 ) ;
#24252 = CARTESIAN_POINT ( 'NONE',  ( 33.58253175000000113, 46.47500000273118559, -10.91162601494193751 ) ) ;
#24253 = CYLINDRICAL_SURFACE ( 'NONE', #5315, 24.50000000000000000 ) ;
#24254 = CARTESIAN_POINT ( 'NONE',  ( -24.18731323226248264, 51.10715250092397355, -14.01125832528284931 ) ) ;
#24255 = CARTESIAN_POINT ( 'NONE',  ( -10.37757302488623701, 69.77500000273117564, 31.93888565452638417 ) ) ;
#24256 = EDGE_LOOP ( 'NONE', ( #26449, #7830, #22266, #6889 ) ) ;
#24257 = CARTESIAN_POINT ( 'NONE',  ( -20.75514604977248823, 16.82500000273120122, -28.56700777964554305 ) ) ;
#24258 = EDGE_CURVE ( 'NONE', #33963, #52, #31699, .T. ) ;
#24259 = CARTESIAN_POINT ( 'NONE',  ( 26.00068869287340334, 23.31510416666666430, -15.01150461594642316 ) ) ;
#24260 = ORIENTED_EDGE ( 'NONE', *, *, #32206, .F. ) ;
#24261 = EDGE_LOOP ( 'NONE', ( #29088, #27158, #743, #8875 ) ) ;
#24262 = VECTOR ( 'NONE', #28119, 1000.000000000000000 ) ;
#24263 = CARTESIAN_POINT ( 'NONE',  ( -26.50000000000000355, -2.000000000000001332, 0.000000000000000000 ) ) ;
#24264 = CARTESIAN_POINT ( 'NONE',  ( 10.37757302488624767, 55.72500000273117138, 31.93888565452638417 ) ) ;
#24265 = CARTESIAN_POINT ( 'NONE',  ( -28.01184896238290278, 59.55208333333332149, 7.505752307973363457 ) ) ;
#24266 = CARTESIAN_POINT ( 'NONE',  ( 6.277390505771533514E-15, 21.00000000546236478, 34.17252228774368916 ) ) ;
#24267 = AXIS2_PLACEMENT_3D ( 'NONE', #24232, #19417, #32104 ) ;
#24268 = CARTESIAN_POINT ( 'NONE',  ( 3.880418787951140036, 16.19874571299077459, -24.49999999999999645 ) ) ;
#24269 = CARTESIAN_POINT ( 'NONE',  ( 18.94512977948575738, 8.924999997268812990, 13.76444248337723408 ) ) ;
#24270 = CARTESIAN_POINT ( 'NONE',  ( -20.75514604977248112, 23.67500000273118843, 28.56700777964554661 ) ) ;
#24271 = CARTESIAN_POINT ( 'NONE',  ( -20.47846945139866648, 68.14024333240935505, 20.53372385742108008 ) ) ;
#24272 = CARTESIAN_POINT ( 'NONE',  ( -8.960552108402742093E-16, 80.37500000273115575, -14.63369212191046387 ) ) ;
#24273 = FACE_OUTER_BOUND ( 'NONE', #5259, .T. ) ;
#24274 = CARTESIAN_POINT ( 'NONE',  ( 10.04305231718579705, 12.59999999999998543, 30.90933677959248982 ) ) ;
#24275 = ORIENTED_EDGE ( 'NONE', *, *, #26774, .T. ) ;
#24276 = CARTESIAN_POINT ( 'NONE',  ( -7.236395654485757944, 1.724999997268800156, -22.27133577429736988 ) ) ;
#24277 = CARTESIAN_POINT ( 'NONE',  ( -8.601468415847518756, 76.57500000273115859, -11.83890561707634781 ) ) ;
#24278 = CARTESIAN_POINT ( 'NONE',  ( -2.428612866367529427E-13, 39.92968750000000000, -27.95245687107222921 ) ) ;
#24279 = CARTESIAN_POINT ( 'NONE',  ( -27.16883889988624290, 22.92500000273117777, -19.73931689729374028 ) ) ;
#24280 = CARTESIAN_POINT ( 'NONE',  ( -20.75514604977248823, 64.82500000273120122, -28.56700777964554305 ) ) ;
#24281 = CARTESIAN_POINT ( 'NONE',  ( 20.75514604977249178, 28.07500000273119412, 28.56700777964553950 ) ) ;
#24282 = CARTESIAN_POINT ( 'NONE',  ( -20.75514604977248823, 17.07500000273119056, -28.56700777964554305 ) ) ;
#24283 = CARTESIAN_POINT ( 'NONE',  ( -33.58253175000000113, 7.475000002731175819, 10.91162601494193929 ) ) ;
#24284 = CARTESIAN_POINT ( 'NONE',  ( 0.04044903254993986036, 55.11756916759064495, -27.95245687107223986 ) ) ;
#24285 = CARTESIAN_POINT ( 'NONE',  ( -20.75514604977248112, 69.42500000273116711, 28.56700777964554661 ) ) ;
#24286 = CARTESIAN_POINT ( 'NONE',  ( -30.02300923189239512, 52.82031249999997868, 2.654126918244515359E-13 ) ) ;
#24287 = CARTESIAN_POINT ( 'NONE',  ( -8.891200544363830713E-16, 73.50000000000001421, -15.00000000000000000 ) ) ;
#24288 = CARTESIAN_POINT ( 'NONE',  ( -11.25946833292375793, 77.17500000273119554, -8.180482586598733619 ) ) ;
#24289 = VECTOR ( 'NONE', #7859, 1000.000000000000000 ) ;
#24290 = CARTESIAN_POINT ( 'NONE',  ( 32.50000000000000000, 57.09999999999999432, -10.55989012756945833 ) ) ;
#24291 = FACE_OUTER_BOUND ( 'NONE', #32048, .T. ) ;
#24292 = CARTESIAN_POINT ( 'NONE',  ( -33.58253175000000113, 61.12500000273119127, 0.000000000000000000 ) ) ;
#24293 = CARTESIAN_POINT ( 'NONE',  ( -23.41746825000000243, 14.02499999726881263, -7.608796670333730638 ) ) ;
#24294 = ORIENTED_EDGE ( 'NONE', *, *, #5178, .T. ) ;
#24295 = CARTESIAN_POINT ( 'NONE',  ( 33.58253175000000113, 68.47500000273119269, -10.91162601494193751 ) ) ;
#24296 = CARTESIAN_POINT ( 'NONE',  ( -10.04305231718578462, 16.39999999999999858, 30.90933677959249337 ) ) ;
#24297 = CARTESIAN_POINT ( 'NONE',  ( -23.41746825000000243, 9.524999997268810858, -7.608796670333730638 ) ) ;
#24298 = CARTESIAN_POINT ( 'NONE',  ( -19.06425588902591173, 23.75038166759064140, -19.11951029504763611 ) ) ;
#24299 = ORIENTED_EDGE ( 'NONE', *, *, #21746, .F. ) ;
#24300 = CARTESIAN_POINT ( 'NONE',  ( -33.58253175000000113, 39.02500000273118985, -10.91162601494193218 ) ) ;
#24301 = VERTEX_POINT ( 'NONE', #26223 ) ;
#24302 = CARTESIAN_POINT ( 'NONE',  ( -26.00068869287340334, 49.09635416666665719, 15.01150461594643382 ) ) ;
#24303 = CARTESIAN_POINT ( 'NONE',  ( 26.29305231718578995, 5.199999999999982414, -19.10302069950538240 ) ) ;
#24304 = CARTESIAN_POINT ( 'NONE',  ( -20.75514604977248112, 73.42500000273118133, 28.56700777964554661 ) ) ;
#24305 = CARTESIAN_POINT ( 'NONE',  ( -26.00068869287340334, 25.03385416666666785, 15.01150461594643382 ) ) ;
#24306 = CARTESIAN_POINT ( 'NONE',  ( 24.50000000000000355, 3.899999999999992806, 7.960532557706212486 ) ) ;
#24307 = CARTESIAN_POINT ( 'NONE',  ( -10.37757302488623701, 11.77500000273118452, 31.93888565452638417 ) ) ;
#24308 = CARTESIAN_POINT ( 'NONE',  ( -20.75514604977248823, 16.82500000273120122, -28.56700777964554305 ) ) ;
#24309 = CARTESIAN_POINT ( 'NONE',  ( -8.601468415847518756, 80.57500000273120122, -11.83890561707634603 ) ) ;
#24310 = CYLINDRICAL_SURFACE ( 'NONE', #17605, 32.50000000000000000 ) ;
#24311 = CARTESIAN_POINT ( 'NONE',  ( -20.47846945139866648, 40.64024333240936215, 20.53372385742108008 ) ) ;
#24312 = CARTESIAN_POINT ( 'NONE',  ( -12.13525491562421088, 77.80000000000001137, -8.816778784387096835 ) ) ;
#24313 = CARTESIAN_POINT ( 'NONE',  ( -20.50609665441004736, 49.81249999999999289, -20.50609665440969565 ) ) ;
#24314 = CARTESIAN_POINT ( 'NONE',  ( 20.08610463437157279, 53.80000000546237970, -27.64615127144129758 ) ) ;
#24315 = CARTESIAN_POINT ( 'NONE',  ( -26.29305231718579350, 38.30000000546237970, -19.10302069950537884 ) ) ;
#24316 = CARTESIAN_POINT ( 'NONE',  ( -6.950374756619247307, 57.54128499907602645, 26.09010956794245217 ) ) ;
#24317 =( BOUNDED_SURFACE ( )  B_SPLINE_SURFACE ( 1, 2, ( 
 ( #11365, #32451, #550, #19263, #8952, #27483, #16521, #16688, #8446, #13618, #32121, #24083, #29704, #21841, #6550, #13944, #1210, #18938, #883, #14113, #716, #11037, #19431, #13777, #6208, #14278, #24407, #32286, #24571, #29880, #22004, #8779, #11523, #1043, #8618, #27316, #3807, #24735, #22175, #30045, #3473, #9116, #21673, #24245, #26973, #17024, #21505, #31954, #5883, #26815, #3311, #22339, #27653, #20452, #33124, #7221, #17361, #30903, #22673, #9627, #30727, #1901, #9976, #20109, #14957, #23021, #30555, #7051, #17533, #7397, #17882, #17706, #20280, #27994, #32785, #28165, #6880, #25072, #32948, #4481, #17195, #9804, #3973, #2074, #12376, #6714, #12202, #25423, #14445, #9451, #19762, #24902, #27825, #1387, #12550, #9278, #4141, #4652, #19933, #11861, #15132 ),
 ( #22498, #22846, #14616, #33476, #30380, #1553, #1722, #33305, #25595, #4307, #12030, #30212, #14782, #25247, #18225, #20631, #26271, #20964, #7735, #28671, #18391, #26441, #31075, #15300, #4821, #26100, #31576, #18561, #28837, #13403, #8074, #7907, #10150, #23534, #25928, #18681, #10656, #25760, #5335, #5164, #33826, #2597, #29004, #15817, #5505, #28335, #28496, #166, #2760, #13225, #10322, #23365, #15986, #31243, #20799, #4993, #2933, #23873, #2422, #33652, #341, #15475, #12890, #23700, #15650, #13060, #10486, #2245, #12719, #21135, #10826, #23190, #21306, #7569, #31414, #31746, #8237, #18052, #11163, #29169, #26610, #13905, #3107, #19226, #18731, #5842, #5676, #11323, #27105, #6004, #8907, #24532, #510, #18893, #19392, #31910, #1003, #8577, #11487, #29663, #3598 ) ),
 .UNSPECIFIED., .F., .F., .T. ) 
 B_SPLINE_SURFACE_WITH_KNOTS ( ( 2, 2 ),
 ( 3, 2, 2, 2, 2, 2, 2, 2, 2, 2, 2, 2, 2, 2, 2, 2, 2, 2, 2, 2, 2, 2, 2, 2, 2, 2, 2, 2, 2, 2, 2, 2, 2, 2, 2, 2, 2, 2, 2, 2, 2, 2, 2, 2, 2, 2, 2, 2, 2, 2, 3 ),
 ( 0.000000000000000000, 1.000000000000000000 ),
 ( 0.000000000000000000, 0.02000000000000000042, 0.04000000000000000083, 0.05999999999999999778, 0.08000000000000000167, 0.1000000000000000056, 0.1199999999999999956, 0.1400000000000000133, 0.1600000000000000033, 0.1799999999999999933, 0.2000000000000000111, 0.2200000000000000011, 0.2399999999999999911, 0.2600000000000000089, 0.2800000000000000266, 0.2999999999999999889, 0.3200000000000000067, 0.3400000000000000244, 0.3599999999999999867, 0.3800000000000000044, 0.4000000000000000222, 0.4199999999999999845, 0.4400000000000000022, 0.4600000000000000200, 0.4799999999999999822, 0.5000000000000000000, 0.5200000000000000178, 0.5400000000000000355, 0.5600000000000000533, 0.5799999999999999600, 0.5999999999999999778, 0.6199999999999999956, 0.6400000000000000133, 0.6600000000000000311, 0.6800000000000000488, 0.6999999999999999556, 0.7199999999999999734, 0.7399999999999999911, 0.7600000000000000089, 0.7800000000000000266, 0.8000000000000000444, 0.8199999999999999512, 0.8399999999999999689, 0.8599999999999999867, 0.8800000000000000044, 0.9000000000000000222, 0.9200000000000000400, 0.9399999999999999467, 0.9599999999999999645, 0.9799999999999999822, 1.000000000000000000 ),
 .UNSPECIFIED. ) 
 GEOMETRIC_REPRESENTATION_ITEM ( )  RATIONAL_B_SPLINE_SURFACE ( (
 ( 1.000000000000000000, 0.9510565162951535312, 1.000000000000000000, 0.9510565162951535312, 1.000000000000000000, 0.9510565162951535312, 1.000000000000000000, 0.9510565162951535312, 1.000000000000000000, 0.9510565162951535312, 1.000000000000000000, 0.9510565162951535312, 1.000000000000000000, 0.9510565162951535312, 1.000000000000000000, 0.9510565162951535312, 1.000000000000000000, 0.9510565162951535312, 1.000000000000000000, 0.9510565162951535312, 1.000000000000000000, 0.9510565162951535312, 1.000000000000000000, 0.9510565162951535312, 1.000000000000000000, 0.9510565162951535312, 1.000000000000000000, 0.9510565162951535312, 1.000000000000000000, 0.9510565162951535312, 1.000000000000000000, 0.9510565162951535312, 1.000000000000000000, 0.9510565162951535312, 1.000000000000000000, 0.9510565162951535312, 1.000000000000000000, 0.9510565162951535312, 1.000000000000000000, 0.9510565162951535312, 1.000000000000000000, 0.9510565162951535312, 1.000000000000000000, 0.9510565162951535312, 1.000000000000000000, 0.9510565162951535312, 1.000000000000000000, 0.9510565162951535312, 1.000000000000000000, 0.9510565162951535312, 1.000000000000000000, 0.9510565162951535312, 1.000000000000000000, 0.9510565162951535312, 1.000000000000000000, 0.9510565162951535312, 1.000000000000000000, 0.9510565162951535312, 1.000000000000000000, 0.9510565162951535312, 1.000000000000000000, 0.9510565162951535312, 1.000000000000000000, 0.9510565162951535312, 1.000000000000000000, 0.9510565162951535312, 1.000000000000000000, 0.9510565162951535312, 1.000000000000000000, 0.9510565162951535312, 1.000000000000000000, 0.9510565162951535312, 1.000000000000000000, 0.9510565162951535312, 1.000000000000000000, 0.9510565162951535312, 1.000000000000000000, 0.9510565162951535312, 1.000000000000000000, 0.9510565162951535312, 1.000000000000000000, 0.9510565162951535312, 1.000000000000000000, 0.9510565162951535312, 1.000000000000000000, 0.9510565162951535312, 1.000000000000000000, 0.9510565162951535312, 1.000000000000000000, 0.9510565162951535312, 1.000000000000000000, 0.9510565162951535312, 1.000000000000000000, 0.9510565162951535312, 1.000000000000000000, 0.9510565162951535312, 1.000000000000000000, 0.9510565162951535312, 1.000000000000000000, 0.9510565162951535312, 1.000000000000000000),
 ( 1.000000000000000000, 0.9510565162951535312, 1.000000000000000000, 0.9510565162951535312, 1.000000000000000000, 0.9510565162951535312, 1.000000000000000000, 0.9510565162951535312, 1.000000000000000000, 0.9510565162951535312, 1.000000000000000000, 0.9510565162951535312, 1.000000000000000000, 0.9510565162951535312, 1.000000000000000000, 0.9510565162951535312, 1.000000000000000000, 0.9510565162951535312, 1.000000000000000000, 0.9510565162951535312, 1.000000000000000000, 0.9510565162951535312, 1.000000000000000000, 0.9510565162951535312, 1.000000000000000000, 0.9510565162951535312, 1.000000000000000000, 0.9510565162951535312, 1.000000000000000000, 0.9510565162951535312, 1.000000000000000000, 0.9510565162951535312, 1.000000000000000000, 0.9510565162951535312, 1.000000000000000000, 0.9510565162951535312, 1.000000000000000000, 0.9510565162951535312, 1.000000000000000000, 0.9510565162951535312, 1.000000000000000000, 0.9510565162951535312, 1.000000000000000000, 0.9510565162951535312, 1.000000000000000000, 0.9510565162951535312, 1.000000000000000000, 0.9510565162951535312, 1.000000000000000000, 0.9510565162951535312, 1.000000000000000000, 0.9510565162951535312, 1.000000000000000000, 0.9510565162951535312, 1.000000000000000000, 0.9510565162951535312, 1.000000000000000000, 0.9510565162951535312, 1.000000000000000000, 0.9510565162951535312, 1.000000000000000000, 0.9510565162951535312, 1.000000000000000000, 0.9510565162951535312, 1.000000000000000000, 0.9510565162951535312, 1.000000000000000000, 0.9510565162951535312, 1.000000000000000000, 0.9510565162951535312, 1.000000000000000000, 0.9510565162951535312, 1.000000000000000000, 0.9510565162951535312, 1.000000000000000000, 0.9510565162951535312, 1.000000000000000000, 0.9510565162951535312, 1.000000000000000000, 0.9510565162951535312, 1.000000000000000000, 0.9510565162951535312, 1.000000000000000000, 0.9510565162951535312, 1.000000000000000000, 0.9510565162951535312, 1.000000000000000000, 0.9510565162951535312, 1.000000000000000000, 0.9510565162951535312, 1.000000000000000000, 0.9510565162951535312, 1.000000000000000000, 0.9510565162951535312, 1.000000000000000000, 0.9510565162951535312, 1.000000000000000000, 0.9510565162951535312, 1.000000000000000000, 0.9510565162951535312, 1.000000000000000000) ) ) 
 REPRESENTATION_ITEM ( '' )  SURFACE ( )  );
#24318 = CARTESIAN_POINT ( 'NONE',  ( 33.58253175000000113, 44.22500000273117138, -10.91162601494193751 ) ) ;
#24319 = CARTESIAN_POINT ( 'NONE',  ( 15.00000000000000000, 73.35000000546237686, -4.873795443493596835 ) ) ;
#24320 = CARTESIAN_POINT ( 'NONE',  ( -20.75514604977248112, 49.67500000273118133, 28.56700777964554661 ) ) ;
#24321 = CARTESIAN_POINT ( 'NONE',  ( 10.37757302488624056, 36.77500000273120406, -31.93888565452638417 ) ) ;
#24322 = CARTESIAN_POINT ( 'NONE',  ( 7.736786493336079928, 16.99999999999999645, 22.60298709876044398 ) ) ;
#24323 = CARTESIAN_POINT ( 'NONE',  ( -26.07999730980477437, 18.30208333333332860, 6.988114217768305103 ) ) ;
#24324 = CARTESIAN_POINT ( 'NONE',  ( -10.04305231718578462, 18.39999999999999858, 30.90933677959249337 ) ) ;
#24325 = DIRECTION ( 'NONE',  ( -0.000000000000000000, -1.000000000000000000, -0.000000000000000000 ) ) ;
#24326 = CARTESIAN_POINT ( 'NONE',  ( -2.092463501923844636E-15, 75.50000000000001421, -34.17252228774368916 ) ) ;
#24327 = CARTESIAN_POINT ( 'NONE',  ( 27.16883889988623935, 8.325000002731188786, -19.73931689729374384 ) ) ;
#24328 = CARTESIAN_POINT ( 'NONE',  ( -23.41746824999999887, 5.524999997268821517, -7.608796670333730638 ) ) ;
#24329 = CARTESIAN_POINT ( 'NONE',  ( -20.08610463437157989, 52.20000000546236407, -27.64615127144129758 ) ) ;
#24330 = CARTESIAN_POINT ( 'NONE',  ( -0.04044903255042732459, 24.74180583240935505, -27.95245687107223986 ) ) ;
#24331 = CARTESIAN_POINT ( 'NONE',  ( 0.000000000000000000, 0.000000000000000000, 0.000000000000000000 ) ) ;
#24332 = CARTESIAN_POINT ( 'NONE',  ( -20.75514604977248823, 22.82500000273118701, -28.56700777964554305 ) ) ;
#24333 = CARTESIAN_POINT ( 'NONE',  ( -23.41746825000000243, 6.024999997268805529, -7.608796670333730638 ) ) ;
#24334 = VECTOR ( 'NONE', #14771, 1000.000000000000000 ) ;
#24335 = CARTESIAN_POINT ( 'NONE',  ( -24.20753774853756823, 49.66927083333330728, -13.97622843553588723 ) ) ;
#24336 = AXIS2_PLACEMENT_3D ( 'NONE', #17048, #6407, #3664 ) ;
#24337 = ORIENTED_EDGE ( 'NONE', *, *, #26284, .T. ) ;
#24338 = CARTESIAN_POINT ( 'NONE',  ( 33.58253175000000113, 56.12500000273119838, -4.112674001490185761E-15 ) ) ;
#24339 = EDGE_CURVE ( 'NONE', #30070, #5024, #12069, .T. ) ;
#24340 = EDGE_LOOP ( 'NONE', ( #26656, #10583, #25724, #12898 ) ) ;
#24341 = CARTESIAN_POINT ( 'NONE',  ( -15.01150461594595775, 24.74739583333332504, 26.00068869287368756 ) ) ;
#24342 = CARTESIAN_POINT ( 'NONE',  ( -7.543491769121417612, 22.60454833425730925, 28.00173670424549499 ) ) ;
#24343 = CARTESIAN_POINT ( 'NONE',  ( 19.82091636218621034, 15.54999999453762705, 14.40073868116559730 ) ) ;
#24344 = EDGE_CURVE ( 'NONE', #16549, #2430, #32816, .T. ) ;
#24345 = CARTESIAN_POINT ( 'NONE',  ( -23.41746825000000598, 7.724999997268809260, 7.608796670333726198 ) ) ;
#24346 = CARTESIAN_POINT ( 'NONE',  ( 33.58253175000000113, 26.37500000273118417, -4.112674001490185761E-15 ) ) ;
#24347 = CARTESIAN_POINT ( 'NONE',  ( 32.50000000000000000, 33.60000000546237686, -10.55989012756945833 ) ) ;
#24348 = CARTESIAN_POINT ( 'NONE',  ( 6.277390505771533514E-15, 76.50000000000001421, 34.17252228774368916 ) ) ;
#24349 = CARTESIAN_POINT ( 'NONE',  ( -26.29305231718579350, 54.30000000546236549, -19.10302069950537884 ) ) ;
#24350 = FACE_OUTER_BOUND ( 'NONE', #11576, .T. ) ;
#24351 = CARTESIAN_POINT ( 'NONE',  ( -2.162160676586881955E-15, 40.87500000273119838, -35.31076352940723240 ) ) ;
#24352 = FILL_AREA_STYLE ('',( #26915 ) ) ;
#24353 = CARTESIAN_POINT ( 'NONE',  ( 20.08610463437158344, 24.70000000000000284, 27.64615127144129403 ) ) ;
#24354 = CARTESIAN_POINT ( 'NONE',  ( -20.08610463437157989, 21.69999999999998153, -27.64615127144129758 ) ) ;
#24355 = COLOUR_RGB ( '', 0.66274510, 0.83137255, 0.94901961) ;
#24356 = CARTESIAN_POINT ( 'NONE',  ( -19.82091636218621389, 13.19999999999998863, 14.40073868116558842 ) ) ;
#24357 = CARTESIAN_POINT ( 'NONE',  ( 6.486482029760649416E-15, 65.62500000273116996, 35.31076352940723240 ) ) ;
#24358 = CARTESIAN_POINT ( 'NONE',  ( 10.37757302488624767, 55.97500000273119980, 31.93888565452638417 ) ) ;
#24359 = CARTESIAN_POINT ( 'NONE',  ( -23.41746825000000243, 13.72499999726882258, 7.608796670333725309 ) ) ;
#24360 = CARTESIAN_POINT ( 'NONE',  ( 32.50000000000000000, 39.50000000546238965, -3.980102097228898626E-15 ) ) ;
#24361 = CARTESIAN_POINT ( 'NONE',  ( -10.37757302488624411, 6.725000002731185589, -31.93888565452638417 ) ) ;
#24362 = CARTESIAN_POINT ( 'NONE',  ( 14.01125832528286352, 34.77902750092397355, -24.18731323226246843 ) ) ;
#24363 = CARTESIAN_POINT ( 'NONE',  ( 32.15037667113031716, 67.00000000000000000, -5.379467130814792775 ) ) ;
#24364 = CARTESIAN_POINT ( 'NONE',  ( -2.357955684373814975, 51.99999999999997868, 33.24972188832315823 ) ) ;
#24365 = CARTESIAN_POINT ( 'NONE',  ( -33.58253175000000113, 27.22500000273119269, 10.91162601494193929 ) ) ;
#24366 = CARTESIAN_POINT ( 'NONE',  ( 2.205017735002230837E-13, 56.00000000546238255, -32.50000000000000000 ) ) ;
#24367 = CARTESIAN_POINT ( 'NONE',  ( 4.222871413987100692E-15, -57.48236190979495319, 0.000000000000000000 ) ) ;
#24368 = CARTESIAN_POINT ( 'NONE',  ( -4.405589869732278832E-13, 31.00000000546236834, 32.50000000000000000 ) ) ;
#24369 = CARTESIAN_POINT ( 'NONE',  ( -0.04044903255044120238, 59.11680583240937636, -30.02300923189239867 ) ) ;
#24370 = CARTESIAN_POINT ( 'NONE',  ( 20.08610463437157279, 45.80000000546240102, -27.64615127144129758 ) ) ;
#24371 = CYLINDRICAL_SURFACE ( 'NONE', #22631, 15.00000000000000000 ) ;
#24372 = CARTESIAN_POINT ( 'NONE',  ( -15.14183272437242067, 16.69999999999999574, -20.84094480462497856 ) ) ;
#24373 = CARTESIAN_POINT ( 'NONE',  ( -6.988114217767819270, 28.04166666666666075, 26.07999730980490583 ) ) ;
#24374 = CARTESIAN_POINT ( 'NONE',  ( -33.58253175000000113, 73.22500000273117848, 10.91162601494193929 ) ) ;
#24375 = CARTESIAN_POINT ( 'NONE',  ( -2.584737979205441561E-13, 33.05468750000000000, -30.02300923189239512 ) ) ;
#24376 = EDGE_CURVE ( 'NONE', #27572, #7428, #6116, .T. ) ;
#24377 = CYLINDRICAL_SURFACE ( 'NONE', #10271, 26.50000000000000355 ) ;
#24378 = ORIENTED_EDGE ( 'NONE', *, *, #13968, .T. ) ;
#24379 = CARTESIAN_POINT ( 'NONE',  ( 30.02300923189239867, 45.66444416759065916, 0.04044903254992252006 ) ) ;
#24380 = CARTESIAN_POINT ( 'NONE',  ( 20.08610463437158344, 15.20000000546237118, 27.64615127144129403 ) ) ;
#24381 = CARTESIAN_POINT ( 'NONE',  ( 15.01150461594643204, 55.11197916666664298, 26.00068869287340334 ) ) ;
#24382 = CARTESIAN_POINT ( 'NONE',  ( -10.04305231718579172, 64.10000000546240528, -30.90933677959248982 ) ) ;
#24383 = CARTESIAN_POINT ( 'NONE',  ( -2.162160676586881955E-15, 46.87500000273118417, -35.31076352940723240 ) ) ;
#24384 = CARTESIAN_POINT ( 'NONE',  ( 6.277390505771533514E-15, 53.00000000546237544, 34.17252228774368916 ) ) ;
#24385 = CARTESIAN_POINT ( 'NONE',  ( 2.688165632520823219E-15, 77.87500000273119838, 14.63369212191046387 ) ) ;
#24386 = CARTESIAN_POINT ( 'NONE',  ( 10.37757302488624767, 35.72500000273118559, 31.93888565452638417 ) ) ;
#24387 = CARTESIAN_POINT ( 'NONE',  ( 20.75514604977248467, 64.67500000273118133, -28.56700777964554305 ) ) ;
#24388 = CARTESIAN_POINT ( 'NONE',  ( -20.08610463437157989, 39.70000000000000284, -27.64615127144129758 ) ) ;
#24389 = CARTESIAN_POINT ( 'NONE',  ( -14.47279130897151589, 11.32499999726881157, -19.92008829642072598 ) ) ;
#24390 = CARTESIAN_POINT ( 'NONE',  ( 33.58253175000000113, 6.375000002731168181, -4.112674001490185761E-15 ) ) ;
#24391 = LINE ( 'NONE', #30193, #2513 ) ;
#24392 = CARTESIAN_POINT ( 'NONE',  ( -8.601468415847515203, 75.67500000273116711, 11.83890561707634959 ) ) ;
#24393 = CARTESIAN_POINT ( 'NONE',  ( 27.16883889988624290, 74.17500000273119554, 19.73931689729373673 ) ) ;
#24394 = DIRECTION ( 'NONE',  ( -0.000000000000000000, -1.000000000000000000, -0.000000000000000000 ) ) ;
#24395 = CARTESIAN_POINT ( 'NONE',  ( 20.75514604977248467, 70.67500000273118133, -28.56700777964554305 ) ) ;
#24396 = ORIENTED_EDGE ( 'NONE', *, *, #20072, .T. ) ;
#24397 = CIRCLE ( 'NONE', #5201, 26.50000000000000000 ) ;
#24398 = CARTESIAN_POINT ( 'NONE',  ( 19.06425588902592239, 15.15663166759064495, 19.11951029504763611 ) ) ;
#24399 = LINE ( 'NONE', #874, #11327 ) ;
#24400 = CARTESIAN_POINT ( 'NONE',  ( 27.16883889988623935, 46.32500000273119412, -19.73931689729374384 ) ) ;
#24401 = CARTESIAN_POINT ( 'NONE',  ( -20.75514604977248823, 11.07500000273119056, -28.56700777964554305 ) ) ;
#24402 = CARTESIAN_POINT ( 'NONE',  ( -20.75514604977248112, 63.67500000273117422, 28.56700777964554661 ) ) ;
#24403 = CARTESIAN_POINT ( 'NONE',  ( 13.97622843553589966, 53.96614583333333570, -24.20753774853756113 ) ) ;
#24404 = CARTESIAN_POINT ( 'NONE',  ( 20.53372385742072481, 41.79725666759063785, -20.47846945139902175 ) ) ;
#24405 = CARTESIAN_POINT ( 'NONE',  ( 0.04044903255045854962, 29.89805583240935860, 30.02300923189239867 ) ) ;
#24406 = CARTESIAN_POINT ( 'NONE',  ( 20.08610463437158344, 69.20000000546235697, 27.64615127144129403 ) ) ;
#24407 = CARTESIAN_POINT ( 'NONE',  ( 4.300734207923757602, 78.27500000273118985, -13.23629886949340673 ) ) ;
#24408 = CARTESIAN_POINT ( 'NONE',  ( 6.950374756619257965, 59.26003499907601935, -26.09010956794244507 ) ) ;
#24409 = CARTESIAN_POINT ( 'NONE',  ( 23.41746824999999887, 14.62499999726882294, 0.000000000000000000 ) ) ;
#24410 = CARTESIAN_POINT ( 'NONE',  ( -7.570916362186215665, 5.149999994537635573, 23.30088464923126423 ) ) ;
#24411 = ORIENTED_EDGE ( 'NONE', *, *, #10090, .F. ) ;
#24412 = CARTESIAN_POINT ( 'NONE',  ( -20.75514604977248823, 47.07500000273117990, -28.56700777964554305 ) ) ;
#24413 = CARTESIAN_POINT ( 'NONE',  ( -15.00000000000000000, 70.25000000546238255, 0.000000000000000000 ) ) ;
#24414 = CARTESIAN_POINT ( 'NONE',  ( 0.04044903254993986036, 48.24256916759064495, -27.95245687107223986 ) ) ;
#24415 = CARTESIAN_POINT ( 'NONE',  ( 33.58253175000000823, 68.27500000273120406, 10.91162601494192863 ) ) ;
#24416 = ORIENTED_EDGE ( 'NONE', *, *, #5042, .T. ) ;
#24417 = CARTESIAN_POINT ( 'NONE',  ( 33.58253175000000113, 20.22500000273117848, -10.91162601494193751 ) ) ;
#24418 = CARTESIAN_POINT ( 'NONE',  ( -26.00068869287340334, 28.47135416666666075, 15.01150461594643382 ) ) ;
#24419 = ORIENTED_EDGE ( 'NONE', *, *, #9334, .F. ) ;
#24420 = CARTESIAN_POINT ( 'NONE',  ( 10.04305231718578817, 65.90000000546237402, -30.90933677959249337 ) ) ;
#24421 = CARTESIAN_POINT ( 'NONE',  ( 27.16883889988624290, 57.92500000273120975, 19.73931689729373673 ) ) ;
#24422 = CARTESIAN_POINT ( 'NONE',  ( 2.740863092043355209E-13, 55.39843749999999289, 30.02300923189239512 ) ) ;
#24423 = CARTESIAN_POINT ( 'NONE',  ( 6.277390505771533514E-15, 11.00000000546238788, 34.17252228774368916 ) ) ;
#24424 = DIRECTION ( 'NONE',  ( -0.000000000000000000, -1.000000000000000000, -0.000000000000000000 ) ) ;
#24425 = CARTESIAN_POINT ( 'NONE',  ( 14.47279130897151944, 17.42499999726882365, -19.92008829642072598 ) ) ;
#24426 = CARTESIAN_POINT ( 'NONE',  ( -33.58253175000000113, 25.27500000273119696, -10.91162601494193218 ) ) ;
#24427 = VECTOR ( 'NONE', #31440, 1000.000000000000000 ) ;
#24428 = CARTESIAN_POINT ( 'NONE',  ( 15.00000000000000355, 76.89999999999999147, 4.873795443493592394 ) ) ;
#24429 = CARTESIAN_POINT ( 'NONE',  ( 0.04044903255044120238, 16.14805583240936215, 27.95245687107223276 ) ) ;
#24430 = CARTESIAN_POINT ( 'NONE',  ( -4.300734207923759378, 80.47500000273119269, -13.23629886949340495 ) ) ;
#24431 = DIRECTION ( 'NONE',  ( -1.224646799147353454E-16, 1.000000000000000000, -0.000000000000000000 ) ) ;
#24432 = CARTESIAN_POINT ( 'NONE',  ( 20.08610463437157279, 11.30000000000000604, -27.64615127144129758 ) ) ;
#24433 = VERTEX_POINT ( 'NONE', #29455 ) ;
#24434 = CARTESIAN_POINT ( 'NONE',  ( -7.236395654485763274, 6.524999997268826846, 22.27133577429736633 ) ) ;
#24435 = CARTESIAN_POINT ( 'NONE',  ( -8.960552108402742093E-16, 74.37500000273118417, -14.63369212191046387 ) ) ;
#24436 = CARTESIAN_POINT ( 'NONE',  ( -13.97622843553588901, 41.93489583333333570, 24.20753774853756823 ) ) ;
#24437 = CARTESIAN_POINT ( 'NONE',  ( 6.486482029760649416E-15, 23.62500000273119127, 35.31076352940723240 ) ) ;
#24438 = CARTESIAN_POINT ( 'NONE',  ( 6.486482029760649416E-15, 63.62500000273117706, 35.31076352940723240 ) ) ;
#24439 = CARTESIAN_POINT ( 'NONE',  ( 6.486482029760649416E-15, 31.87500000273119127, 35.31076352940723240 ) ) ;
#24440 = CARTESIAN_POINT ( 'NONE',  ( -33.58253175000000113, 19.27500000273117919, -10.91162601494193218 ) ) ;
#24441 = CARTESIAN_POINT ( 'NONE',  ( -27.16883889988623935, 7.575000002731202997, 19.73931689729374739 ) ) ;
#24442 = CARTESIAN_POINT ( 'NONE',  ( 6.950374756619721595, 63.56809000092398065, 26.09010956794232428 ) ) ;
#24443 = CARTESIAN_POINT ( 'NONE',  ( -27.16883889988623935, 69.32500000273117280, 19.73931689729374739 ) ) ;
#24444 = CARTESIAN_POINT ( 'NONE',  ( 15.01150461594596308, 57.40364583333333570, -26.00068869287367335 ) ) ;
#24445 = LINE ( 'NONE', #8488, #22231 ) ;
#24446 = CARTESIAN_POINT ( 'NONE',  ( 13.91746824999999532, 78.47500000273116427, -4.522059556121118540 ) ) ;
#24447 = CARTESIAN_POINT ( 'NONE',  ( -32.50000000000000000, 46.09999999999999432, 10.55989012756946366 ) ) ;
#24448 = CARTESIAN_POINT ( 'NONE',  ( -15.00000000000000000, 72.25000000546238255, 0.000000000000000000 ) ) ;
#24449 = CARTESIAN_POINT ( 'NONE',  ( -2.162160676586882350E-15, 50.62500000273117706, -35.31076352940722529 ) ) ;
#24450 = CARTESIAN_POINT ( 'NONE',  ( -23.41746825000000598, 14.22499999726880660, 7.608796670333726198 ) ) ;
#24451 = ORIENTED_EDGE ( 'NONE', *, *, #32906, .F. ) ;
#24452 = CARTESIAN_POINT ( 'NONE',  ( -10.37757302488624411, 68.97500000273119269, -31.93888565452638417 ) ) ;
#24453 = CARTESIAN_POINT ( 'NONE',  ( 27.16883889988623935, 2.325000002731170134, -19.73931689729374384 ) ) ;
#24454 = AXIS2_PLACEMENT_3D ( 'NONE', #8436, #13093, #29204 ) ;
#24455 = CARTESIAN_POINT ( 'NONE',  ( 7.236395654485755280, 6.224999997268803931, 22.27133577429736988 ) ) ;
#24456 = CARTESIAN_POINT ( 'NONE',  ( 14.01125832528286352, 21.02902750092397710, -24.18731323226246843 ) ) ;
#24457 = VERTEX_POINT ( 'NONE', #22249 ) ;
#24458 = CARTESIAN_POINT ( 'NONE',  ( 33.58253175000000823, 38.02500000273117564, 10.91162601494192863 ) ) ;
#24459 = CARTESIAN_POINT ( 'NONE',  ( 26.50000000000000000, -15.84529946162074943, 0.000000000000000000 ) ) ;
#24460 = ORIENTED_EDGE ( 'NONE', *, *, #21344, .T. ) ;
#24461 = CARTESIAN_POINT ( 'NONE',  ( -15.01150461594595775, 52.24739583333332860, 26.00068869287368756 ) ) ;
#24462 = CARTESIAN_POINT ( 'NONE',  ( 33.58253175000000113, 60.37500000273119127, -4.112674001490185761E-15 ) ) ;
#24463 = CARTESIAN_POINT ( 'NONE',  ( -32.50000000000000000, 0.6000000054623827461, 10.55989012756946366 ) ) ;
#24464 = CARTESIAN_POINT ( 'NONE',  ( -27.16883889988623935, 77.32500000273118701, 19.73931689729374739 ) ) ;
#24465 = CARTESIAN_POINT ( 'NONE',  ( -7.505752307972844761, 34.91666666666666430, 28.01184896238304134 ) ) ;
#24466 = ADVANCED_FACE ( 'NONE', ( #32693 ), #11278, .T. ) ;
#24467 = CARTESIAN_POINT ( 'NONE',  ( 15.14183272437241889, 3.699999999999999289, 20.84094480462498211 ) ) ;
#24468 = CARTESIAN_POINT ( 'NONE',  ( -20.75514604977248823, 7.075000002731188786, -28.56700777964554305 ) ) ;
#24469 = CARTESIAN_POINT ( 'NONE',  ( 33.58253175000000823, 16.02500000273119340, 10.91162601494192863 ) ) ;
#24470 = CARTESIAN_POINT ( 'NONE',  ( -11.25946833292375793, 74.67500000273119554, -8.180482586598733619 ) ) ;
#24471 = CARTESIAN_POINT ( 'NONE',  ( 25.98046417659831775, 45.93972249907602645, -15.04653450569338879 ) ) ;
#24472 = CARTESIAN_POINT ( 'NONE',  ( -8.960552108402742093E-16, 72.87500000273115575, -14.63369212191046387 ) ) ;
#24473 = CARTESIAN_POINT ( 'NONE',  ( 28.01184896238304134, 51.24479166666666430, 7.505752307972846538 ) ) ;
#24474 = EDGE_CURVE ( 'NONE', #22018, #23625, #2515, .T. ) ;
#24475 = CARTESIAN_POINT ( 'NONE',  ( -24.50000000000000711, 8.849999994537624204, 7.960532557706201828 ) ) ;
#24476 = CARTESIAN_POINT ( 'NONE',  ( -26.29305231718578995, 54.70000000546236407, 19.10302069950538595 ) ) ;
#24477 = CARTESIAN_POINT ( 'NONE',  ( -19.09188309203694445, 11.99999999999999645, -19.09188309203661049 ) ) ;
#24478 = CARTESIAN_POINT ( 'NONE',  ( 6.486482029760649416E-15, 45.62500000273118417, 35.31076352940723240 ) ) ;
#24479 = CARTESIAN_POINT ( 'NONE',  ( 4.300734207923761154, 77.47500000273116427, 13.23629886949340495 ) ) ;
#24480 = CARTESIAN_POINT ( 'NONE',  ( 27.16883889988623935, 50.57500000273117280, -19.73931689729374384 ) ) ;
#24481 = CARTESIAN_POINT ( 'NONE',  ( -10.37757302488624411, 30.97500000273117848, -31.93888565452638417 ) ) ;
#24482 = CARTESIAN_POINT ( 'NONE',  ( 19.82091636218621034, 17.80000000000001137, 14.40073868116559730 ) ) ;
#24483 = CARTESIAN_POINT ( 'NONE',  ( -6.988114217768288228, 22.59895833333332860, -26.07999730980477437 ) ) ;
#24484 = CARTESIAN_POINT ( 'NONE',  ( 4.349545668204547685E-15, -58.51673569255127205, 0.000000000000000000 ) ) ;
#24485 = VECTOR ( 'NONE', #5874, 1000.000000000000000 ) ;
#24486 = CARTESIAN_POINT ( 'NONE',  ( -15.00000000000000000, 75.90000000000000568, -4.873795443493594171 ) ) ;
#24487 = CARTESIAN_POINT ( 'NONE',  ( 26.29305231718578995, 75.20000000000000284, -19.10302069950538240 ) ) ;
#24488 = CARTESIAN_POINT ( 'NONE',  ( 20.75514604977249178, 11.82500000273118346, 28.56700777964553950 ) ) ;
#24489 = CARTESIAN_POINT ( 'NONE',  ( 7.236395654485760609, 7.024999997268799312, -22.27133577429736633 ) ) ;
#24490 = CARTESIAN_POINT ( 'NONE',  ( -5.147494310547430452, 52.05125428700922185, -32.49999999999999289 ) ) ;
#24491 = CARTESIAN_POINT ( 'NONE',  ( 26.06988505166722803, 32.33295166574267654, -7.025853678916862854 ) ) ;
#24492 = CARTESIAN_POINT ( 'NONE',  ( -15.14183272437242778, 13.29999999999998650, 20.84094480462497856 ) ) ;
#24493 = CARTESIAN_POINT ( 'NONE',  ( -33.58253175000000113, 17.02500000273119340, -10.91162601494193041 ) ) ;
#24494 = CARTESIAN_POINT ( 'NONE',  ( -7.236395654485757944, 3.724999997268802154, -22.27133577429736988 ) ) ;
#24495 = CARTESIAN_POINT ( 'NONE',  ( -24.20753774853730889, 52.53385416666666430, 13.97622843553633842 ) ) ;
#24496 = ORIENTED_EDGE ( 'NONE', *, *, #11361, .F. ) ;
#24497 = CARTESIAN_POINT ( 'NONE',  ( 33.58253175000000823, 54.02500000273118275, 10.91162601494192863 ) ) ;
#24498 = CARTESIAN_POINT ( 'NONE',  ( -20.75514604977248823, 31.07500000273118701, -28.56700777964554305 ) ) ;
#24499 = VERTEX_POINT ( 'NONE', #626 ) ;
#24500 = CARTESIAN_POINT ( 'NONE',  ( 20.50609665440969565, 19.73437500000000000, -20.50609665441004736 ) ) ;
#24501 = CARTESIAN_POINT ( 'NONE',  ( -26.02091320914849959, 23.03423583425731280, 14.97647472619947528 ) ) ;
#24502 = CARTESIAN_POINT ( 'NONE',  ( 24.50000000000000000, 15.74999999453763344, 0.000000000000000000 ) ) ;
#24503 = CARTESIAN_POINT ( 'NONE',  ( 23.41746825000000243, 8.524999997268812635, 7.608796670333735079 ) ) ;
#24504 = CARTESIAN_POINT ( 'NONE',  ( -33.58253175000000113, 31.47500000273117493, 10.91162601494193929 ) ) ;
#24505 = CARTESIAN_POINT ( 'NONE',  ( -32.50000000000000000, 28.60000000546238397, 10.55989012756946366 ) ) ;
#24506 =( BOUNDED_CURVE ( )  B_SPLINE_CURVE ( 2, ( #14320, #33653, #14487, #10151, #14154, #16733, #2246, #22377, #4822, #28336, #12720, #20453, #25596 ),
 .UNSPECIFIED., .F., .T. ) 
 B_SPLINE_CURVE_WITH_KNOTS ( ( 3, 2, 2, 2, 2, 2, 3 ),
 ( 0.2115384615384615363, 0.2128205128205128138, 0.2153846153846153966, 0.2179487179487179516, 0.2205128205128205066, 0.2230769230769230893, 0.2243589743589743668 ),
 .UNSPECIFIED. ) 
 CURVE ( )  GEOMETRIC_REPRESENTATION_ITEM ( )  RATIONAL_B_SPLINE_CURVE ( ( 0.9755282581475768211, 0.9755282581475768211, 1.000000000000000000, 0.9510565162951535312, 1.000000000000000000, 0.9510565162951535312, 1.000000000000000000, 0.9510565162951535312, 1.000000000000000000, 0.9510565162951535312, 1.000000000000000000, 0.9755282581475768211, 0.9755282581475768211 ) ) 
 REPRESENTATION_ITEM ( '' )  );
#24507 = CARTESIAN_POINT ( 'NONE',  ( 6.277390505771533514E-15, 70.50000000000001421, 34.17252228774368916 ) ) ;
#24508 = CARTESIAN_POINT ( 'NONE',  ( 3.980102097228898626E-15, 52.00000000000000711, -32.50000000000000000 ) ) ;
#24509 = DIRECTION ( 'NONE',  ( 0.000000000000000000, 0.000000000000000000, -1.000000000000000000 ) ) ;
#24510 = CARTESIAN_POINT ( 'NONE',  ( 30.02300923189239867, 55.97694416759064495, 0.04044903254992252006 ) ) ;
#24511 = CARTESIAN_POINT ( 'NONE',  ( -2.162160676586881955E-15, 44.87500000273119127, -35.31076352940723240 ) ) ;
#24512 =( LENGTH_UNIT ( ) NAMED_UNIT ( * ) SI_UNIT ( .MILLI., .METRE. ) );
#24513 = VECTOR ( 'NONE', #229, 1000.000000000000114 ) ;
#24514 = CARTESIAN_POINT ( 'NONE',  ( 18.94512977948576093, 9.324999997268824004, -13.76444248337722875 ) ) ;
#24515 = CARTESIAN_POINT ( 'NONE',  ( -20.08610463437156923, 12.29999999999999183, 27.64615127144130113 ) ) ;
#24516 = CARTESIAN_POINT ( 'NONE',  ( -15.14183272437241889, 14.70000000000000107, -20.84094480462497856 ) ) ;
#24517 = CARTESIAN_POINT ( 'NONE',  ( 19.11951029504797006, 46.65586833240934794, 19.06425588902558133 ) ) ;
#24518 = CARTESIAN_POINT ( 'NONE',  ( 27.16883889988623935, 64.32500000273120122, -19.73931689729374384 ) ) ;
#24519 = CARTESIAN_POINT ( 'NONE',  ( -20.75514604977248823, 49.07500000273117280, -28.56700777964554305 ) ) ;
#24520 = CARTESIAN_POINT ( 'NONE',  ( -23.41746825000000243, 9.724999997268803043, 7.608796670333725309 ) ) ;
#24521 = CARTESIAN_POINT ( 'NONE',  ( 3.880418787951134707, 3.551254281546844194, 24.50000000000000000 ) ) ;
#24522 = CARTESIAN_POINT ( 'NONE',  ( 20.75514604977248467, 4.425000002731183990, -28.56700777964554305 ) ) ;
#24523 = CARTESIAN_POINT ( 'NONE',  ( 24.18731323226247554, 39.07590250092398065, 14.01125832528285997 ) ) ;
#24524 = EDGE_CURVE ( 'NONE', #31336, #21143, #32363, .T. ) ;
#24525 = CARTESIAN_POINT ( 'NONE',  ( 32.50000000000000000, 25.50000000546237544, -3.980102097228898626E-15 ) ) ;
#24526 = CARTESIAN_POINT ( 'NONE',  ( -12.18942006770533837, 51.99999999999998579, 30.86762708970428193 ) ) ;
#24527 = CARTESIAN_POINT ( 'NONE',  ( 20.75514604977248467, 28.42500000273118133, -28.56700777964554305 ) ) ;
#24528 = CARTESIAN_POINT ( 'NONE',  ( 5.779280353836490358E-15, 22.49999999999999645, 32.49999999999999289 ) ) ;
#24529 = CARTESIAN_POINT ( 'NONE',  ( 20.08610463437158344, 60.70000000000000284, 27.64615127144129403 ) ) ;
#24530 = CARTESIAN_POINT ( 'NONE',  ( 20.47846945139867003, 56.10899333240935505, -20.53372385742107653 ) ) ;
#24531 = CARTESIAN_POINT ( 'NONE',  ( 26.29305231718579350, 51.30000000546237970, 19.10302069950537529 ) ) ;
#24532 = CARTESIAN_POINT ( 'NONE',  ( 13.91746825000000065, 72.27500000273116143, 4.522059556121114987 ) ) ;
#24533 = CARTESIAN_POINT ( 'NONE',  ( -20.08610463437156923, 58.80000000546239391, 27.64615127144130113 ) ) ;
#24534 = CARTESIAN_POINT ( 'NONE',  ( -26.07999730980477437, 21.73958333333332860, 6.988114217768305103 ) ) ;
#24535 = CARTESIAN_POINT ( 'NONE',  ( 10.37757302488624767, 77.72500000273117848, 31.93888565452638417 ) ) ;
#24536 = CARTESIAN_POINT ( 'NONE',  ( -30.02300923189239512, 28.75781249999999645, 2.654126918244515359E-13 ) ) ;
#24537 = DIRECTION ( 'NONE',  ( 0.000000000000000000, -1.000000000000000000, 0.000000000000000000 ) ) ;
#24538 = ORIENTED_EDGE ( 'NONE', *, *, #24946, .F. ) ;
#24539 = CARTESIAN_POINT ( 'NONE',  ( -15.04653450569291984, 53.68527750092398065, 25.98046417659859486 ) ) ;
#24540 = CARTESIAN_POINT ( 'NONE',  ( 26.29305231718578995, 13.70000000546238361, -19.10302069950538240 ) ) ;
#24541 = CARTESIAN_POINT ( 'NONE',  ( 15.01150461594596308, 57.40364583333333570, -26.00068869287367335 ) ) ;
#24542 = CARTESIAN_POINT ( 'NONE',  ( -32.50000000000000000, 46.60000000546236976, 10.55989012756946366 ) ) ;
#24543 = CARTESIAN_POINT ( 'NONE',  ( -20.75514604977248823, 45.07500000273117990, -28.56700777964554305 ) ) ;
#24544 = CARTESIAN_POINT ( 'NONE',  ( 26.29305231718579350, 47.30000000546235839, 19.10302069950537529 ) ) ;
#24545 = CARTESIAN_POINT ( 'NONE',  ( 8.601468415847520532, 74.07500000273121543, 11.83890561707634781 ) ) ;
#24546 = CARTESIAN_POINT ( 'NONE',  ( -10.37757302488624411, 34.72500000273118559, -31.93888565452638417 ) ) ;
#24547 = CARTESIAN_POINT ( 'NONE',  ( -20.08610463437157989, 62.20000000546237118, -27.64615127144129758 ) ) ;
#24548 = CARTESIAN_POINT ( 'NONE',  ( -10.37757302488623701, 59.77500000273119696, 31.93888565452638417 ) ) ;
#24549 = CARTESIAN_POINT ( 'NONE',  ( -32.50000000000000000, 35.90000000000000568, -10.55989012756945478 ) ) ;
#24550 = CARTESIAN_POINT ( 'NONE',  ( 20.08610463437157279, 37.30000000000001847, -27.64615127144129758 ) ) ;
#24551 = CARTESIAN_POINT ( 'NONE',  ( 14.47279130897151589, 12.32499999726880802, 19.92008829642072953 ) ) ;
#24552 = CARTESIAN_POINT ( 'NONE',  ( -33.58253175000000113, 7.475000002731175819, 10.91162601494193929 ) ) ;
#24553 = CARTESIAN_POINT ( 'NONE',  ( 0.000000000000000000, 80.00000000000001421, 0.000000000000000000 ) ) ;
#24554 = CARTESIAN_POINT ( 'NONE',  ( -13.91746824999999887, 81.37500000273118417, 0.000000000000000000 ) ) ;
#24555 = CARTESIAN_POINT ( 'NONE',  ( -20.75514604977248112, 71.67500000273118133, 28.56700777964554661 ) ) ;
#24556 = CARTESIAN_POINT ( 'NONE',  ( -19.82091636218621389, 5.200000000000009948, 14.40073868116558842 ) ) ;
#24557 = CARTESIAN_POINT ( 'NONE',  ( 33.58253175000000823, 66.27500000273118985, 10.91162601494192863 ) ) ;
#24558 = ORIENTED_EDGE ( 'NONE', *, *, #25513, .T. ) ;
#24559 = CARTESIAN_POINT ( 'NONE',  ( 1.577395562988744260E-15, 4.249999994537624559, -25.76082449383753925 ) ) ;
#24560 = CARTESIAN_POINT ( 'NONE',  ( -24.22776226481240514, 16.15923583425731636, 13.94119854578937812 ) ) ;
#24561 = EDGE_CURVE ( 'NONE', #14202, #28636, #14484, .T. ) ;
#24562 = CARTESIAN_POINT ( 'NONE',  ( 15.00000000000000355, 74.89999999999999147, 4.873795443493592394 ) ) ;
#24563 = CARTESIAN_POINT ( 'NONE',  ( 20.75514604977248467, 50.42500000273118843, -28.56700777964554305 ) ) ;
#24564 = CARTESIAN_POINT ( 'NONE',  ( 6.486482029760649416E-15, 13.87500000273117529, 35.31076352940723240 ) ) ;
#24565 = CARTESIAN_POINT ( 'NONE',  ( 20.75514604977248467, 60.67500000273118133, -28.56700777964554305 ) ) ;
#24566 = CARTESIAN_POINT ( 'NONE',  ( 13.97622843553589966, 47.09114583333332860, -24.20753774853756113 ) ) ;
#24567 = CARTESIAN_POINT ( 'NONE',  ( -26.02091320914849959, 40.22173583425730925, 14.97647472619947528 ) ) ;
#24568 = EDGE_CURVE ( 'NONE', #5896, #29590, #15610, .T. ) ;
#24569 = CARTESIAN_POINT ( 'NONE',  ( -30.02300923189239867, 30.75743083240935505, 0.04044903255044988294 ) ) ;
#24570 = CARTESIAN_POINT ( 'NONE',  ( 6.277390505771533514E-15, 67.00000000546236834, 34.17252228774368916 ) ) ;
#24571 = CARTESIAN_POINT ( 'NONE',  ( 11.25946833292375793, 78.07500000273121543, -8.180482586598735395 ) ) ;
#24572 = CARTESIAN_POINT ( 'NONE',  ( -27.95245687107223986, 54.81993083240935505, 0.04044903255043252877 ) ) ;
#24573 = CARTESIAN_POINT ( 'NONE',  ( -23.41746825000000598, 17.72499999726881725, 7.608796670333726198 ) ) ;
#24574 = CARTESIAN_POINT ( 'NONE',  ( -24.50000000000000000, 17.00000000000001421, -3.000384657911015469E-15 ) ) ;
#24575 = ORIENTED_EDGE ( 'NONE', *, *, #19302, .F. ) ;
#24576 = CARTESIAN_POINT ( 'NONE',  ( 33.58253175000000113, 38.37500000273118417, -4.112674001490185761E-15 ) ) ;
#24577 = CARTESIAN_POINT ( 'NONE',  ( -23.41746824999999887, 4.024999997268810858, -7.608796670333730638 ) ) ;
#24578 = CARTESIAN_POINT ( 'NONE',  ( -26.09010956794232428, 47.23996500092398065, 6.950374756619732253 ) ) ;
#24579 = CARTESIAN_POINT ( 'NONE',  ( 32.50000000000000711, 27.40000000546239534, 10.55989012756945122 ) ) ;
#24580 = ORIENTED_EDGE ( 'NONE', *, *, #15609, .T. ) ;
#24581 = CARTESIAN_POINT ( 'NONE',  ( 20.75514604977248467, 18.42500000273117422, -28.56700777964554305 ) ) ;
#24582 = CARTESIAN_POINT ( 'NONE',  ( -20.50609665440969209, 35.20312500000000000, 20.50609665441005092 ) ) ;
#24583 = ORIENTED_EDGE ( 'NONE', *, *, #14595, .F. ) ;
#24584 = DIRECTION ( 'NONE',  ( -1.000000000000000000, 0.000000000000000000, 0.000000000000000000 ) ) ;
#24585 = CARTESIAN_POINT ( 'NONE',  ( -2.162160676586881955E-15, 52.62500000273117706, -35.31076352940723240 ) ) ;
#24586 = CARTESIAN_POINT ( 'NONE',  ( -20.50609665440969209, 55.82812499999999289, 20.50609665441005092 ) ) ;
#24587 = CARTESIAN_POINT ( 'NONE',  ( -20.08610463437157989, 12.20000000546237828, -27.64615127144129758 ) ) ;
#24588 = CARTESIAN_POINT ( 'NONE',  ( 0.000000000000000000, 16.99999999999998579, 0.000000000000000000 ) ) ;
#24589 = CARTESIAN_POINT ( 'NONE',  ( 1.507698388325705758E-15, 15.62499999726882116, -24.62258325217400312 ) ) ;
#24590 = CARTESIAN_POINT ( 'NONE',  ( 26.29305231718578995, 57.20000000000000284, -19.10302069950538240 ) ) ;
#24591 = CARTESIAN_POINT ( 'NONE',  ( -27.16883889988623935, 25.57500000273119056, 19.73931689729374739 ) ) ;
#24592 = CARTESIAN_POINT ( 'NONE',  ( -32.50000000000000000, 24.50000000546237544, 0.000000000000000000 ) ) ;
#24593 = CARTESIAN_POINT ( 'NONE',  ( -30.02300923189239867, 68.56993083240934084, 0.04044903255044988294 ) ) ;
#24594 = CARTESIAN_POINT ( 'NONE',  ( -11.25946833292375793, 77.07500000273121543, 8.180482586598737171 ) ) ;
#24595 = CARTESIAN_POINT ( 'NONE',  ( 1.555960095263670572E-15, 12.50000000000000355, -24.50000000000000000 ) ) ;
#24596 = CARTESIAN_POINT ( 'NONE',  ( 32.50000000000000000, 12.99999999999999822, -3.980102097228898626E-15 ) ) ;
#24597 = ORIENTED_EDGE ( 'NONE', *, *, #30841, .F. ) ;
#24598 = CARTESIAN_POINT ( 'NONE',  ( 23.41746825000000243, 7.024999997268802865, 7.608796670333735079 ) ) ;
#24599 = CARTESIAN_POINT ( 'NONE',  ( -8.601468415847518756, 74.57500000273117280, -11.83890561707634781 ) ) ;
#24600 = CARTESIAN_POINT ( 'NONE',  ( 27.95245687107222921, 40.78906249999998579, -2.463307335887066074E-13 ) ) ;
#24601 = CARTESIAN_POINT ( 'NONE',  ( -20.75514604977248112, 15.42500000273118843, 28.56700777964554661 ) ) ;
#24602 = CARTESIAN_POINT ( 'NONE',  ( -10.37757302488623701, 69.52500000273118985, 31.93888565452638417 ) ) ;
#24603 = CARTESIAN_POINT ( 'NONE',  ( -27.16883889988624290, 27.17500000273119554, -19.73931689729374028 ) ) ;
#24604 = CARTESIAN_POINT ( 'NONE',  ( -27.16883889988624290, 15.17500000273118488, -19.73931689729374028 ) ) ;
#24605 = CARTESIAN_POINT ( 'NONE',  ( -20.75514604977248112, 7.675000002731198201, 28.56700777964554661 ) ) ;
#24606 = CARTESIAN_POINT ( 'NONE',  ( -26.06988505166735237, 64.71392333425730214, -7.025853678916388567 ) ) ;
#24607 = CARTESIAN_POINT ( 'NONE',  ( -28.01184896238304134, 49.52604166666666430, -7.505752307972844761 ) ) ;
#24608 = CARTESIAN_POINT ( 'NONE',  ( -15.00000000000000000, 81.89999999999997726, -4.873795443493594171 ) ) ;
#24609 = CARTESIAN_POINT ( 'NONE',  ( 13.91746825000000065, 80.27500000273117564, 4.522059556121115875 ) ) ;
#24610 = CARTESIAN_POINT ( 'NONE',  ( -26.29305231718579350, 49.79999999999999716, -19.10302069950537884 ) ) ;
#24611 = CARTESIAN_POINT ( 'NONE',  ( 26.29305231718578995, 57.70000000546237118, -19.10302069950538240 ) ) ;
#24612 = CARTESIAN_POINT ( 'NONE',  ( -10.37757302488624411, 52.72500000273119980, -31.93888565452638417 ) ) ;
#24613 = CARTESIAN_POINT ( 'NONE',  ( -4.523095164977116484E-15, 16.62499999726881583, 24.62258325217400312 ) ) ;
#24614 = EDGE_LOOP ( 'NONE', ( #21473, #18987, #7453, #8205 ) ) ;
#24615 = CARTESIAN_POINT ( 'NONE',  ( 27.16883889988624290, 64.17500000273116711, 19.73931689729373673 ) ) ;
#24616 = DIRECTION ( 'NONE',  ( 0.000000000000000000, 0.000000000000000000, 1.000000000000000000 ) ) ;
#24617 = CARTESIAN_POINT ( 'NONE',  ( 23.41746825000000243, 6.724999997268811924, -7.608796670333727974 ) ) ;
#24618 = CARTESIAN_POINT ( 'NONE',  ( 27.95245687107223986, 28.47694416759064495, 0.04044903254993640479 ) ) ;
#24619 = EDGE_LOOP ( 'NONE', ( #32255, #23708, #31998, #18282 ) ) ;
#24620 = CARTESIAN_POINT ( 'NONE',  ( 33.58253175000000113, 40.12500000273118417, -4.112674001490185761E-15 ) ) ;
#24621 = CARTESIAN_POINT ( 'NONE',  ( 3.980102097228898626E-15, 80.00000000000001421, 32.50000000000000000 ) ) ;
#24622 = ADVANCED_FACE ( 'NONE', ( #1981 ), #7581, .T. ) ;
#24623 = ORIENTED_EDGE ( 'NONE', *, *, #19597, .F. ) ;
#24624 = CARTESIAN_POINT ( 'NONE',  ( 30.02300923189239512, 51.10156249999998579, -2.619432448724977703E-13 ) ) ;
#24625 = CARTESIAN_POINT ( 'NONE',  ( 33.58253175000000823, 62.27500000273118275, 10.91162601494192863 ) ) ;
#24626 = CARTESIAN_POINT ( 'NONE',  ( 12.13525491562421088, 75.05000000546240813, 8.816778784387095058 ) ) ;
#24627 = CARTESIAN_POINT ( 'NONE',  ( 6.486482029760649416E-15, 73.62500000273118417, 35.31076352940723240 ) ) ;
#24628 = CARTESIAN_POINT ( 'NONE',  ( 28.01184896238290278, 26.89583333333332860, -7.505752307973347470 ) ) ;
#24629 = CARTESIAN_POINT ( 'NONE',  ( -24.50000000000000000, 7.000000000000006217, -3.000384657911015469E-15 ) ) ;
#24630 = CARTESIAN_POINT ( 'NONE',  ( -2.162160676586881955E-15, 2.875000002731204596, -35.31076352940723240 ) ) ;
#24631 = CARTESIAN_POINT ( 'NONE',  ( 33.58253175000000113, 16.12500000273120548, -4.112674001490185761E-15 ) ) ;
#24632 = DIRECTION ( 'NONE',  ( 0.000000000000000000, 0.000000000000000000, -1.000000000000000000 ) ) ;
#24633 = CARTESIAN_POINT ( 'NONE',  ( 20.53372385742108008, 39.78086833240934794, 20.47846945139866648 ) ) ;
#24634 = CARTESIAN_POINT ( 'NONE',  ( 12.13525491562420910, 79.19999999999998863, -8.816778784387098611 ) ) ;
#24635 = CARTESIAN_POINT ( 'NONE',  ( 7.505752307973351023, 62.13020833333334281, 28.01184896238290278 ) ) ;
#24636 = CARTESIAN_POINT ( 'NONE',  ( -20.08610463437157989, 38.20000000546236407, -27.64615127144129758 ) ) ;
#24637 = CARTESIAN_POINT ( 'NONE',  ( 26.07999730980490227, 16.86979166666666075, 6.988114217767821046 ) ) ;
#24638 = CARTESIAN_POINT ( 'NONE',  ( -33.58253175000000113, 35.12500000273119127, 0.000000000000000000 ) ) ;
#24639 = CARTESIAN_POINT ( 'NONE',  ( 8.601468415847520532, 77.57500000273115859, 11.83890561707634781 ) ) ;
#24640 = CARTESIAN_POINT ( 'NONE',  ( -33.58253175000000113, 51.37500000273119127, 0.000000000000000000 ) ) ;
#24641 = CARTESIAN_POINT ( 'NONE',  ( -20.75514604977248112, 25.67500000273118488, 28.56700777964554661 ) ) ;
#24642 = CARTESIAN_POINT ( 'NONE',  ( -10.86059781102998478, 16.99999999999999289, 21.84823680246600119 ) ) ;
#24643 = CARTESIAN_POINT ( 'NONE',  ( -24.20753774853756823, 29.04427083333332860, -13.97622843553588723 ) ) ;
#24644 = CARTESIAN_POINT ( 'NONE',  ( 24.50000000000000000, 11.64999999453762314, 7.960532557706212486 ) ) ;
#24645 = CARTESIAN_POINT ( 'NONE',  ( -10.04305231718579172, 44.10000000546238397, -30.90933677959248982 ) ) ;
#24646 = CARTESIAN_POINT ( 'NONE',  ( -26.29305231718579350, 63.80000000000001137, -19.10302069950537884 ) ) ;
#24647 = CARTESIAN_POINT ( 'NONE',  ( -33.58253175000000113, 7.125000002731182391, 0.000000000000000000 ) ) ;
#24648 = CARTESIAN_POINT ( 'NONE',  ( -14.47279130897151767, 7.324999997268822227, -19.92008829642072598 ) ) ;
#24649 = CARTESIAN_POINT ( 'NONE',  ( -7.543491769121917656, 24.59857666574268720, -28.00173670424536354 ) ) ;
#24650 = EDGE_CURVE ( 'NONE', #20831, #31469, #12456, .T. ) ;
#24651 = CARTESIAN_POINT ( 'NONE',  ( 15.14183272437242422, 12.29999999999999183, -20.84094480462497856 ) ) ;
#24652 = CARTESIAN_POINT ( 'NONE',  ( -26.06988505166722803, 27.17670166574268009, 7.025853678916877953 ) ) ;
#24653 = CARTESIAN_POINT ( 'NONE',  ( -32.50000000000000000, 60.00000000000000000, 0.000000000000000000 ) ) ;
#24654 = CARTESIAN_POINT ( 'NONE',  ( -33.58253175000000113, 13.22500000273119802, 10.91162601494193929 ) ) ;
#24655 = CARTESIAN_POINT ( 'NONE',  ( 7.236395654485755280, 4.724999997268803043, 22.27133577429736988 ) ) ;
#24656 = CARTESIAN_POINT ( 'NONE',  ( -6.988114217768288228, 56.97395833333333570, -26.07999730980477437 ) ) ;
#24657 = EDGE_CURVE ( 'NONE', #7743, #7355, #17330, .T. ) ;
#24658 = ORIENTED_EDGE ( 'NONE', *, *, #26052, .T. ) ;
#24659 = CARTESIAN_POINT ( 'NONE',  ( -27.16883889988623935, 59.32500000273120833, 19.73931689729374739 ) ) ;
#24660 = CARTESIAN_POINT ( 'NONE',  ( -33.58253175000000113, 27.27500000273119340, -10.91162601494193218 ) ) ;
#24661 = ORIENTED_EDGE ( 'NONE', *, *, #10983, .T. ) ;
#24662 = CARTESIAN_POINT ( 'NONE',  ( 26.00068869287340334, 23.31510416666666430, -15.01150461594642316 ) ) ;
#24663 = CARTESIAN_POINT ( 'NONE',  ( -20.53372385742071771, 26.32850666759063785, 20.47846945139902530 ) ) ;
#24664 = CARTESIAN_POINT ( 'NONE',  ( 24.50000000000000000, 17.74999999453763522, 0.000000000000000000 ) ) ;
#24665 = EDGE_CURVE ( 'NONE', #17459, #18081, #12175, .T. ) ;
#24666 = CARTESIAN_POINT ( 'NONE',  ( -23.41746825000000243, 3.524999997268826402, -7.608796670333730638 ) ) ;
#24667 = CARTESIAN_POINT ( 'NONE',  ( 10.37757302488624767, 23.97500000273117138, 31.93888565452638417 ) ) ;
#24668 = CARTESIAN_POINT ( 'NONE',  ( 20.08610463437158344, 31.20000000546238894, 27.64615127144129403 ) ) ;
#24669 = CARTESIAN_POINT ( 'NONE',  ( 32.50000000000000000, 73.00000000000001421, -3.980102097228898626E-15 ) ) ;
#24670 = CARTESIAN_POINT ( 'NONE',  ( 6.001560367445586717E-15, 3.249999994537631665, 24.50000000000000000 ) ) ;
#24671 = CARTESIAN_POINT ( 'NONE',  ( 7.890940483122900408E-14, 10.49999999999999112, -24.50000000000000000 ) ) ;
#24672 = CARTESIAN_POINT ( 'NONE',  ( -7.543491769121417612, 60.41704833425730214, 28.00173670424549499 ) ) ;
#24673 = CARTESIAN_POINT ( 'NONE',  ( 10.37757302488624056, 36.77500000273120406, -31.93888565452638417 ) ) ;
#24674 = CARTESIAN_POINT ( 'NONE',  ( 20.75514604977248467, 56.42500000273120264, -28.56700777964554305 ) ) ;
#24675 = CARTESIAN_POINT ( 'NONE',  ( -26.02091320914878025, 48.23138916574269786, -14.97647472619899389 ) ) ;
#24676 = CARTESIAN_POINT ( 'NONE',  ( -20.50609665441004736, 25.74999999999999645, -20.50609665440969565 ) ) ;
#24677 = CARTESIAN_POINT ( 'NONE',  ( 14.47279130897151767, 7.424999997268820096, -19.92008829642072598 ) ) ;
#24678 = CARTESIAN_POINT ( 'NONE',  ( -32.50000000000000000, 13.89999999999999858, -10.55989012756945478 ) ) ;
#24679 = CARTESIAN_POINT ( 'NONE',  ( 24.50000000000000000, 14.00000000000001243, 0.000000000000000000 ) ) ;
#24680 = CARTESIAN_POINT ( 'NONE',  ( -24.18731323226221974, 40.78347249907601935, 14.01125832528330406 ) ) ;
#24681 = CARTESIAN_POINT ( 'NONE',  ( 10.37757302488624056, 60.52500000273119696, -31.93888565452638417 ) ) ;
#24682 = CARTESIAN_POINT ( 'NONE',  ( -10.37757302488623701, 47.77500000273118985, 31.93888565452638417 ) ) ;
#24683 = CARTESIAN_POINT ( 'NONE',  ( -14.47279130897151767, 11.32499999726881157, -19.92008829642072598 ) ) ;
#24684 = CARTESIAN_POINT ( 'NONE',  ( -24.50000000000000000, 9.000000000000007105, -3.000384657911015469E-15 ) ) ;
#24685 = CARTESIAN_POINT ( 'NONE',  ( -33.58253175000000113, 5.025000002731194293, -10.91162601494193218 ) ) ;
#24686 = CARTESIAN_POINT ( 'NONE',  ( 24.22776226481241224, 41.94048583425730925, -13.94119854578936923 ) ) ;
#24687 = CARTESIAN_POINT ( 'NONE',  ( 26.29305231718579350, 25.30000000546236905, 19.10302069950537529 ) ) ;
#24688 = CARTESIAN_POINT ( 'NONE',  ( 2.067204126564591252E-14, 4.499999999999996447, -24.50000000000000000 ) ) ;
#24689 = UNCERTAINTY_MEASURE_WITH_UNIT (LENGTH_MEASURE( 1.000000000000000082E-05 ), #5485, 'distance_accuracy_value', 'NONE');
#24690 = CARTESIAN_POINT ( 'NONE',  ( 10.37757302488624767, 29.72500000273119269, 31.93888565452638417 ) ) ;
#24691 = DIRECTION ( 'NONE',  ( 0.000000000000000000, -1.000000000000000000, 0.000000000000000000 ) ) ;
#24692 = CARTESIAN_POINT ( 'NONE',  ( 0.000000000000000000, 80.00000000000001421, 0.000000000000000000 ) ) ;
#24693 = CARTESIAN_POINT ( 'NONE',  ( -24.49999999999999645, -23.00000000000000355, 0.000000000000000000 ) ) ;
#24694 = CARTESIAN_POINT ( 'NONE',  ( 28.02196122052058413, 56.68190999907602645, 7.468012846824272799 ) ) ;
#24695 = CARTESIAN_POINT ( 'NONE',  ( -32.50000000000000000, 48.50000000546238255, 0.000000000000000000 ) ) ;
#24696 = CARTESIAN_POINT ( 'NONE',  ( -5.147494310547430452, 58.05125428700921475, -32.49999999999999289 ) ) ;
#24697 = CARTESIAN_POINT ( 'NONE',  ( -24.20753774853756823, 22.16927083333332504, -13.97622843553588723 ) ) ;
#24698 = ORIENTED_EDGE ( 'NONE', *, *, #22050, .T. ) ;
#24699 = CARTESIAN_POINT ( 'NONE',  ( 27.16883889988623935, 72.32500000273118701, -19.73931689729374384 ) ) ;
#24700 = CARTESIAN_POINT ( 'NONE',  ( -30.02300923189239512, 32.19531250000000000, 2.654126918244515359E-13 ) ) ;
#24701 = LINE ( 'NONE', #17163, #1470 ) ;
#24702 = ORIENTED_EDGE ( 'NONE', *, *, #31274, .F. ) ;
#24703 = CARTESIAN_POINT ( 'NONE',  ( 30.02300923189239867, 52.53944416759064495, 0.04044903254992252006 ) ) ;
#24704 = CARTESIAN_POINT ( 'NONE',  ( 26.29305231718578995, 11.70000000546238184, -19.10302069950538240 ) ) ;
#24705 = CARTESIAN_POINT ( 'NONE',  ( -2.584737979205441561E-13, 63.99218749999997868, -30.02300923189239512 ) ) ;
#24706 = CARTESIAN_POINT ( 'NONE',  ( 32.50000000000000000, 21.10000000000000142, -10.55989012756945833 ) ) ;
#24707 = CARTESIAN_POINT ( 'NONE',  ( -27.16883889988623935, 45.57500000273117990, 19.73931689729374739 ) ) ;
#24708 = CARTESIAN_POINT ( 'NONE',  ( -32.50000000000000000, 50.50000000546239676, 0.000000000000000000 ) ) ;
#24709 = CARTESIAN_POINT ( 'NONE',  ( 15.00000000000000355, 80.90000000000000568, 4.873795443493592394 ) ) ;
#24710 = CARTESIAN_POINT ( 'NONE',  ( -33.58253175000000113, 27.12500000273118772, 0.000000000000000000 ) ) ;
#24711 = CARTESIAN_POINT ( 'NONE',  ( -10.04305231718578462, 62.90000000546238113, 30.90933677959249337 ) ) ;
#24712 = CARTESIAN_POINT ( 'NONE',  ( -27.16883889988623935, 57.57500000273119412, 19.73931689729374739 ) ) ;
#24713 = DIRECTION ( 'NONE',  ( 1.000000000000000000, 0.000000000000000000, 0.000000000000000000 ) ) ;
#24714 = CARTESIAN_POINT ( 'NONE',  ( 26.29305231718579350, 34.79999999999998295, 19.10302069950537529 ) ) ;
#24715 = CARTESIAN_POINT ( 'NONE',  ( 32.50000000000000000, 33.00000000000000000, -3.980102097228898626E-15 ) ) ;
#24716 = CARTESIAN_POINT ( 'NONE',  ( 14.47279130897151589, 8.324999997268818674, 19.92008829642072953 ) ) ;
#24717 = CARTESIAN_POINT ( 'NONE',  ( 33.58253175000000113, 2.375000002731192161, -4.112674001490185761E-15 ) ) ;
#24718 = DIRECTION ( 'NONE',  ( 0.000000000000000000, -0.000000000000000000, -1.000000000000000000 ) ) ;
#24719 = VECTOR ( 'NONE', #15095, 1000.000000000000000 ) ;
#24720 = CARTESIAN_POINT ( 'NONE',  ( -11.25946833292375793, 77.57500000273121543, 8.180482586598737171 ) ) ;
#24721 = CARTESIAN_POINT ( 'NONE',  ( 20.75514604977248467, 64.67500000273116711, -28.56700777964554305 ) ) ;
#24722 = CARTESIAN_POINT ( 'NONE',  ( -15.14183272437242067, 18.44999999453760964, -20.84094480462497856 ) ) ;
#24723 = CARTESIAN_POINT ( 'NONE',  ( -33.58253175000000113, 63.37500000273120548, 0.000000000000000000 ) ) ;
#24724 = ORIENTED_EDGE ( 'NONE', *, *, #23732, .F. ) ;
#24725 = CARTESIAN_POINT ( 'NONE',  ( 19.82091636218621034, 7.549999994537620829, 14.40073868116559730 ) ) ;
#24726 = CARTESIAN_POINT ( 'NONE',  ( -7.025853678916393008, 12.29204833425730925, 26.06988505166735592 ) ) ;
#24727 = CARTESIAN_POINT ( 'NONE',  ( 12.13525491562421088, 74.80000000000001137, 8.816778784387095058 ) ) ;
#24728 = CARTESIAN_POINT ( 'NONE',  ( 6.486482029760649416E-15, 47.62500000273118417, 35.31076352940723240 ) ) ;
#24729 = CARTESIAN_POINT ( 'NONE',  ( 10.37757302488624767, 7.975000002731199800, 31.93888565452638417 ) ) ;
#24730 = CARTESIAN_POINT ( 'NONE',  ( 27.16883889988624290, 64.17500000273116711, 19.73931689729373673 ) ) ;
#24731 = CARTESIAN_POINT ( 'NONE',  ( -24.20753774853756823, 49.66927083333332149, -13.97622843553588723 ) ) ;
#24732 = CARTESIAN_POINT ( 'NONE',  ( 20.53372385742072481, 34.92225666759063074, -20.47846945139902175 ) ) ;
#24733 = CARTESIAN_POINT ( 'NONE',  ( -20.53372385742107653, 31.18711833240935150, -20.47846945139867003 ) ) ;
#24734 = CARTESIAN_POINT ( 'NONE',  ( 26.29305231718579350, 65.30000000546236549, 19.10302069950537529 ) ) ;
#24735 = CARTESIAN_POINT ( 'NONE',  ( -8.601468415847515203, 77.17500000273118133, 11.83890561707634959 ) ) ;
#24736 = CARTESIAN_POINT ( 'NONE',  ( -14.01125832528328985, 51.95534749907602645, -24.18731323226223040 ) ) ;
#24737 = FACE_OUTER_BOUND ( 'NONE', #7275, .T. ) ;
#24738 = CARTESIAN_POINT ( 'NONE',  ( 10.04305231718578817, 13.90000000546237580, -30.90933677959249337 ) ) ;
#24739 = ORIENTED_EDGE ( 'NONE', *, *, #28947, .F. ) ;
#24740 = CARTESIAN_POINT ( 'NONE',  ( -20.75514604977248112, 43.67500000273119554, 28.56700777964554661 ) ) ;
#24741 = CARTESIAN_POINT ( 'NONE',  ( 23.41746824999999887, 3.224999997268806151, -7.608796670333727974 ) ) ;
#24742 =( GEOMETRIC_REPRESENTATION_CONTEXT ( 3 ) GLOBAL_UNCERTAINTY_ASSIGNED_CONTEXT ( ( #32572 ) ) GLOBAL_UNIT_ASSIGNED_CONTEXT ( ( #7800, #23259, #30617 ) ) REPRESENTATION_CONTEXT ( 'NONE', 'WORKASPACE' ) );
#24743 = CARTESIAN_POINT ( 'NONE',  ( -10.04305231718579172, 30.10000000546238397, -30.90933677959248982 ) ) ;
#24744 = VERTEX_POINT ( 'NONE', #7127 ) ;
#24745 = CARTESIAN_POINT ( 'NONE',  ( 7.505752307972854531, 36.63541666666666430, -28.01184896238303423 ) ) ;
#24747 = ORIENTED_EDGE ( 'NONE', *, *, #12800, .T. ) ;
#24746 = EDGE_CURVE ( 'NONE', #3731, #5367, #17608, .T. ) ;
#24748 = CARTESIAN_POINT ( 'NONE',  ( 20.08610463437158344, 26.70000000000000284, 27.64615127144129403 ) ) ;
#24749 = CARTESIAN_POINT ( 'NONE',  ( 27.16883889988623935, 52.32500000273118701, -19.73931689729374384 ) ) ;
#24750 = CARTESIAN_POINT ( 'NONE',  ( 28.01184896238304134, 58.11979166666665719, 7.505752307972846538 ) ) ;
#24751 = EDGE_CURVE ( 'NONE', #11875, #14813, #33214, .T. ) ;
#24752 = CARTESIAN_POINT ( 'NONE',  ( 10.04305231718579705, 9.100000005462376862, 30.90933677959248982 ) ) ;
#24753 = DIRECTION ( 'NONE',  ( 0.000000000000000000, 0.000000000000000000, -1.000000000000000000 ) ) ;
#24754 = CARTESIAN_POINT ( 'NONE',  ( -23.41746825000000243, 18.22499999726879238, 7.608796670333725309 ) ) ;
#24755 = CARTESIAN_POINT ( 'NONE',  ( -26.29305231718579350, 55.80000000000001847, -19.10302069950537884 ) ) ;
#24756 = CARTESIAN_POINT ( 'NONE',  ( -10.37757302488623701, 25.77500000273119696, 31.93888565452638417 ) ) ;
#24757 = CARTESIAN_POINT ( 'NONE',  ( -28.02196122052058413, 68.71315999907601224, -7.468012846824272799 ) ) ;
#24758 = CARTESIAN_POINT ( 'NONE',  ( -4.300734207923759378, 74.47500000273119269, -13.23629886949340495 ) ) ;
#24759 = CARTESIAN_POINT ( 'NONE',  ( 5.779280353836490358E-15, 56.49999999999998579, 32.49999999999999289 ) ) ;
#24760 = CARTESIAN_POINT ( 'NONE',  ( -1.778240108872766143E-15, 33.50000000000000000, -32.49999999999999289 ) ) ;
#24761 = CARTESIAN_POINT ( 'NONE',  ( -10.04305231718579172, 7.599999999999981881, -30.90933677959248982 ) ) ;
#24762 = ORIENTED_EDGE ( 'NONE', *, *, #3570, .F. ) ;
#24763 = CARTESIAN_POINT ( 'NONE',  ( 18.94512977948575738, 6.924999997268810326, 13.76444248337723408 ) ) ;
#24764 = CARTESIAN_POINT ( 'NONE',  ( 0.000000000000000000, 52.00000000000000711, 32.50000000000000000 ) ) ;
#24765 = CARTESIAN_POINT ( 'NONE',  ( 24.20753774853731244, 40.50260416666666430, -13.97622843553632599 ) ) ;
#24766 = CARTESIAN_POINT ( 'NONE',  ( 33.58253175000000823, 66.02500000273118985, 10.91162601494192863 ) ) ;
#24767 = CARTESIAN_POINT ( 'NONE',  ( 33.58253175000000113, 32.37500000273117706, -4.112674001490185761E-15 ) ) ;
#24768 = CARTESIAN_POINT ( 'NONE',  ( 10.37757302488624767, 13.97500000273120513, 31.93888565452638417 ) ) ;
#24769 = CARTESIAN_POINT ( 'NONE',  ( 10.37757302488624767, 9.975000002731187365, 31.93888565452638417 ) ) ;
#24770 = CARTESIAN_POINT ( 'NONE',  ( 13.94119854578937812, 63.42486083425730925, 24.22776226481240514 ) ) ;
#24771 = CARTESIAN_POINT ( 'NONE',  ( -28.01184896238304134, 56.40104166666666430, -7.505752307972844761 ) ) ;
#24772 = CARTESIAN_POINT ( 'NONE',  ( -13.91746824999999887, 80.87500000273118417, 0.000000000000000000 ) ) ;
#24773 = CARTESIAN_POINT ( 'NONE',  ( 2.688165632520823219E-15, 79.87500000273119838, 14.63369212191046209 ) ) ;
#24774 = CARTESIAN_POINT ( 'NONE',  ( -20.08610463437157989, 45.69999999999998863, -27.64615127144129758 ) ) ;
#24775 = CARTESIAN_POINT ( 'NONE',  ( 32.50000000000000000, 57.50000000546238965, -3.980102097228898626E-15 ) ) ;
#24776 = CARTESIAN_POINT ( 'NONE',  ( -20.75514604977248823, 54.82500000273118701, -28.56700777964554305 ) ) ;
#24777 = CARTESIAN_POINT ( 'NONE',  ( 23.41746825000000243, 2.724999997268822138, -7.608796670333727974 ) ) ;
#24778 = ORIENTED_EDGE ( 'NONE', *, *, #24561, .T. ) ;
#24779 = CARTESIAN_POINT ( 'NONE',  ( -27.16883889988623935, 59.57500000273117990, 19.73931689729374739 ) ) ;
#24780 = LINE ( 'NONE', #4018, #33325 ) ;
#24781 = AXIS2_PLACEMENT_3D ( 'NONE', #29299, #5799, #16608 ) ;
#24782 = CARTESIAN_POINT ( 'NONE',  ( -23.41746825000000598, 7.724999997268809260, 7.608796670333726198 ) ) ;
#24783 = CARTESIAN_POINT ( 'NONE',  ( 19.11951029504763611, 31.48475666759063074, -19.06425588902591173 ) ) ;
#24784 = ORIENTED_EDGE ( 'NONE', *, *, #29543, .F. ) ;
#24785 = CARTESIAN_POINT ( 'NONE',  ( 33.58253175000000113, 28.12500000273120193, -4.112674001490185761E-15 ) ) ;
#24786 = CARTESIAN_POINT ( 'NONE',  ( -26.29305231718579350, 34.30000000546237970, -19.10302069950537884 ) ) ;
#24787 = VERTEX_POINT ( 'NONE', #26009 ) ;
#24788 = CARTESIAN_POINT ( 'NONE',  ( 30.02300923189239512, 47.66406249999998579, -2.619432448724977703E-13 ) ) ;
#24789 = CARTESIAN_POINT ( 'NONE',  ( 10.37757302488624056, 62.77500000273117564, -31.93888565452638417 ) ) ;
#24790 = CARTESIAN_POINT ( 'NONE',  ( -15.00000000000000000, 76.00000000000001421, 0.000000000000000000 ) ) ;
#24791 = CARTESIAN_POINT ( 'NONE',  ( 33.58253175000000113, 74.22500000273119269, -10.91162601494193751 ) ) ;
#24792 = CARTESIAN_POINT ( 'NONE',  ( -7.505752307973343918, 29.47395833333332860, -28.01184896238290989 ) ) ;
#24793 = CARTESIAN_POINT ( 'NONE',  ( -24.50000000000000000, 5.000000000000004441, -3.000384657911015469E-15 ) ) ;
#24794 = CARTESIAN_POINT ( 'NONE',  ( -20.75514604977248112, 1.675000002731184434, 28.56700777964554661 ) ) ;
#24795 = EDGE_CURVE ( 'NONE', #21231, #31792, #10891, .T. ) ;
#24796 = CARTESIAN_POINT ( 'NONE',  ( 10.37757302488624056, 14.52500000273118630, -31.93888565452638417 ) ) ;
#24797 =( BOUNDED_CURVE ( )  B_SPLINE_CURVE ( 2, ( #784, #26878, #22520, #5779, #17215, #16586, #3373, #27042, #24144, #29278, #11266, #19166, #612 ),
 .UNSPECIFIED., .F., .T. ) 
 B_SPLINE_CURVE_WITH_KNOTS ( ( 3, 2, 2, 2, 2, 2, 3 ),
 ( 0.2500000000000000000, 0.2600000000000000089, 0.2800000000000000266, 0.2999999999999999889, 0.3200000000000000067, 0.3400000000000000244, 0.3500000000000000333 ),
 .UNSPECIFIED. ) 
 CURVE ( )  GEOMETRIC_REPRESENTATION_ITEM ( )  RATIONAL_B_SPLINE_CURVE ( ( 0.9755282581475768211, 0.9755282581475768211, 1.000000000000000000, 0.9510565162951535312, 1.000000000000000000, 0.9510565162951535312, 1.000000000000000000, 0.9510565162951535312, 1.000000000000000000, 0.9510565162951535312, 1.000000000000000000, 0.9755282581475767101, 0.9755282581475768211 ) ) 
 REPRESENTATION_ITEM ( '' )  );
#24798 = CARTESIAN_POINT ( 'NONE',  ( -13.91746824999999532, 72.97500000273117848, 4.522059556121122093 ) ) ;
#24799 = CARTESIAN_POINT ( 'NONE',  ( 15.04653450569339945, 43.36159749907602645, 25.98046417659831775 ) ) ;
#24800 = CARTESIAN_POINT ( 'NONE',  ( -15.00000000000000000, 79.90000000000001990, -4.873795443493594171 ) ) ;
#24801 = CARTESIAN_POINT ( 'NONE',  ( -7.505752307972844761, 58.97916666666666430, 28.01184896238304134 ) ) ;
#24802 = CARTESIAN_POINT ( 'NONE',  ( 5.147494310547426899, 53.94874572391552903, -32.50000000000000000 ) ) ;
#24803 = CARTESIAN_POINT ( 'NONE',  ( 7.570916362186207671, 9.349999994537617098, 23.30088464923126779 ) ) ;
#24804 = CARTESIAN_POINT ( 'NONE',  ( 4.635254915624209993, 75.65000000546237402, -14.26584774442730463 ) ) ;
#24805 = CARTESIAN_POINT ( 'NONE',  ( 24.22776226481265383, 67.13763916574266943, 13.94119854578893580 ) ) ;
#24806 = CARTESIAN_POINT ( 'NONE',  ( 20.75514604977248467, 36.42500000273118843, -28.56700777964554305 ) ) ;
#24807 = CARTESIAN_POINT ( 'NONE',  ( 8.601468415847516980, 74.17500000273122396, -11.83890561707634781 ) ) ;
#24808 = CARTESIAN_POINT ( 'NONE',  ( 20.75514604977248467, 50.67500000273117422, -28.56700777964554305 ) ) ;
#24809 = CARTESIAN_POINT ( 'NONE',  ( 33.58253175000000113, 28.37500000273118772, -4.112674001490185761E-15 ) ) ;
#24810 = EDGE_CURVE ( 'NONE', #24251, #32007, #13292, .T. ) ;
#24811 = CARTESIAN_POINT ( 'NONE',  ( 3.503834181885622456, 16.99999999999998934, 23.74784554439683149 ) ) ;
#24812 = AXIS2_PLACEMENT_3D ( 'NONE', #13090, #26302, #18757 ) ;
#24813 = CARTESIAN_POINT ( 'NONE',  ( -27.95245687107223276, 35.63281249999999289, 2.498001805406602216E-13 ) ) ;
#24814 = CARTESIAN_POINT ( 'NONE',  ( -4.223320258572821363E-15, 80.49999999999998579, 15.00000000000000355 ) ) ;
#24815 = CARTESIAN_POINT ( 'NONE',  ( 32.50000000000000000, 64.99999999999998579, -3.980102097228898626E-15 ) ) ;
#24816 = CARTESIAN_POINT ( 'NONE',  ( 7.236395654485760609, 13.02499999726880375, -22.27133577429736633 ) ) ;
#24817 = CARTESIAN_POINT ( 'NONE',  ( 7.543491769121922985, 29.75482666574269075, 28.00173670424535644 ) ) ;
#24818 = CARTESIAN_POINT ( 'NONE',  ( -2.375766604868045029, 77.55125428154684641, -14.99999999999999822 ) ) ;
#24819 = CARTESIAN_POINT ( 'NONE',  ( -14.01125832528328985, 41.64284749907602645, -24.18731323226223040 ) ) ;
#24820 = CARTESIAN_POINT ( 'NONE',  ( 10.37757302488624056, 14.52500000273118630, -31.93888565452638417 ) ) ;
#24821 = CARTESIAN_POINT ( 'NONE',  ( -18.94512977948575738, 7.924999997268811214, -13.76444248337723231 ) ) ;
#24822 = CARTESIAN_POINT ( 'NONE',  ( 27.95245687107222921, 57.97656249999997868, -2.463307335887066074E-13 ) ) ;
#24823 = ORIENTED_EDGE ( 'NONE', *, *, #4738, .F. ) ;
#24824 = CARTESIAN_POINT ( 'NONE',  ( -20.75514604977248823, 54.82500000273118701, -28.56700777964554305 ) ) ;
#24825 = CARTESIAN_POINT ( 'NONE',  ( -10.37757302488624411, 30.97500000273119269, -31.93888565452638417 ) ) ;
#24826 = VERTEX_POINT ( 'NONE', #31155 ) ;
#24827 = CARTESIAN_POINT ( 'NONE',  ( -20.50609665441004736, 25.74999999999999645, -20.50609665440969565 ) ) ;
#24828 = CARTESIAN_POINT ( 'NONE',  ( 28.00173670424549499, 25.18267333425730214, 7.543491769121417612 ) ) ;
#24829 = CARTESIAN_POINT ( 'NONE',  ( 5.779280353836490358E-15, 73.00000000546236834, 32.49999999999999289 ) ) ;
#24830 = CARTESIAN_POINT ( 'NONE',  ( 24.50000000000000000, 13.74999999453763166, 0.000000000000000000 ) ) ;
#24831 = AXIS2_PLACEMENT_3D ( 'NONE', #28089, #12474, #10072 ) ;
#24832 = CARTESIAN_POINT ( 'NONE',  ( -23.41746824999999887, 5.624999997268814944, -2.867812753649727150E-15 ) ) ;
#24833 = CARTESIAN_POINT ( 'NONE',  ( -2.162160676586881955E-15, 20.87500000273119127, -35.31076352940723240 ) ) ;
#24834 = CARTESIAN_POINT ( 'NONE',  ( 26.29305231718579350, 23.30000000546236905, 19.10302069950537529 ) ) ;
#24835 = CARTESIAN_POINT ( 'NONE',  ( 32.50000000000000000, 71.00000000000001421, -3.980102097228898626E-15 ) ) ;
#24836 = DIRECTION ( 'NONE',  ( 0.000000000000000000, -1.000000000000000000, 0.000000000000000000 ) ) ;
#24837 = CARTESIAN_POINT ( 'NONE',  ( 0.7848642672870491666, 74.00000000000002842, 14.13069591803647640 ) ) ;
#24838 = CARTESIAN_POINT ( 'NONE',  ( -7.468012846824771955, 54.97434000092398065, -28.02196122052045624 ) ) ;
#24839 = CARTESIAN_POINT ( 'NONE',  ( -27.16883889988623935, 33.57500000273120122, 19.73931689729374739 ) ) ;
#24840 = CARTESIAN_POINT ( 'NONE',  ( 33.58253175000000113, 56.12500000273119838, -4.112674001490185761E-15 ) ) ;
#24841 = CARTESIAN_POINT ( 'NONE',  ( -28.01184896238304134, 28.90104166666666785, -7.505752307972844761 ) ) ;
#24842 = SHAPE_REPRESENTATION_RELATIONSHIP ( 'NONE' , 'NONE' ,  #19696, #15260 ) ;
#24843 = CARTESIAN_POINT ( 'NONE',  ( -4.523095164977116484E-15, 8.624999997268810503, 24.62258325217400312 ) ) ;
#24844 = CARTESIAN_POINT ( 'NONE',  ( -10.04305231718579172, 17.60000000000000497, -30.90933677959248982 ) ) ;
#24845 = CARTESIAN_POINT ( 'NONE',  ( 24.50000000000000355, 9.900000000000007461, 7.960532557706212486 ) ) ;
#24846 = CARTESIAN_POINT ( 'NONE',  ( 13.94119854578893580, 42.21576416574269075, -24.22776226481265383 ) ) ;
#24847 = CARTESIAN_POINT ( 'NONE',  ( 33.58253175000000113, 56.22500000273117138, -10.91162601494193751 ) ) ;
#24848 = CARTESIAN_POINT ( 'NONE',  ( -27.16883889988624290, 47.17500000273119554, -19.73931689729374028 ) ) ;
#24849 = CARTESIAN_POINT ( 'NONE',  ( -18.94512977948576093, 7.824999997268822227, 13.76444248337722698 ) ) ;
#24850 = CARTESIAN_POINT ( 'NONE',  ( 23.95873412499999944, 0.3124999986344190184, 0.000000000000000000 ) ) ;
#24851 = CARTESIAN_POINT ( 'NONE',  ( 5.779280353836490358E-15, 6.500000000000002665, 32.49999999999999289 ) ) ;
#24852 = CARTESIAN_POINT ( 'NONE',  ( -26.06988505166735237, 50.96392333425730925, -7.025853678916388567 ) ) ;
#24853 = CARTESIAN_POINT ( 'NONE',  ( -24.50000000000000000, 4.649999994537640902, -7.960532557706207157 ) ) ;
#24854 = CYLINDRICAL_SURFACE ( 'NONE', #19860, 32.50000000000000000 ) ;
#24855 = CARTESIAN_POINT ( 'NONE',  ( 20.75514604977249178, 21.82500000273119056, 28.56700777964553950 ) ) ;
#24856 = LINE ( 'NONE', #1508, #15500 ) ;
#24857 = CARTESIAN_POINT ( 'NONE',  ( 32.50000000000000000, 53.00000000000000711, -3.980102097228898626E-15 ) ) ;
#24858 = VECTOR ( 'NONE', #26059, 1000.000000000000000 ) ;
#24859 = CARTESIAN_POINT ( 'NONE',  ( 24.50000000000000000, 14.00000000000001243, 0.000000000000000000 ) ) ;
#24860 = CARTESIAN_POINT ( 'NONE',  ( -0.04044903255042732459, 14.42930583240935505, -27.95245687107223986 ) ) ;
#24861 = CARTESIAN_POINT ( 'NONE',  ( 26.29305231718578995, 45.70000000546238539, -19.10302069950538240 ) ) ;
#24862 = CARTESIAN_POINT ( 'NONE',  ( -27.16883889988624290, 32.92500000273118843, -19.73931689729374028 ) ) ;
#24863 = CARTESIAN_POINT ( 'NONE',  ( 13.97622843553589966, 23.02864583333332149, -24.20753774853756113 ) ) ;
#24864 = ORIENTED_EDGE ( 'NONE', *, *, #17404, .T. ) ;
#24865 = CARTESIAN_POINT ( 'NONE',  ( 10.37757302488624767, 73.72500000273117848, 31.93888565452638417 ) ) ;
#24866 = CARTESIAN_POINT ( 'NONE',  ( 30.02300923189239512, 27.03906250000000000, -2.619432448724977703E-13 ) ) ;
#24867 = DIRECTION ( 'NONE',  ( -0.000000000000000000, -1.000000000000000000, -0.000000000000000000 ) ) ;
#24868 = ORIENTED_EDGE ( 'NONE', *, *, #31186, .T. ) ;
#24869 = CARTESIAN_POINT ( 'NONE',  ( -20.53372385742071771, 46.95350666759064495, 20.47846945139902530 ) ) ;
#24870 = CARTESIAN_POINT ( 'NONE',  ( -20.08610463437156923, 8.800000005462383257, 27.64615127144130113 ) ) ;
#24871 = CARTESIAN_POINT ( 'NONE',  ( 15.01150461594643204, 58.54947916666665009, 26.00068869287340334 ) ) ;
#24872 = CARTESIAN_POINT ( 'NONE',  ( 32.50000000000000000, 56.99999999999999289, -3.980102097228898626E-15 ) ) ;
#24873 = CARTESIAN_POINT ( 'NONE',  ( 20.75514604977248467, 42.67500000273119554, -28.56700777964554305 ) ) ;
#24874 = CARTESIAN_POINT ( 'NONE',  ( 20.08610463437157279, 47.80000000546239391, -27.64615127144129758 ) ) ;
#24875 = EDGE_CURVE ( 'NONE', #7013, #31666, #21617, .T. ) ;
#24876 = CARTESIAN_POINT ( 'NONE',  ( -4.300734207923755825, 71.77500000273117564, 13.23629886949340673 ) ) ;
#24877 = CARTESIAN_POINT ( 'NONE',  ( 27.16883889988623935, 28.32500000273119412, -19.73931689729374384 ) ) ;
#24878 = CARTESIAN_POINT ( 'NONE',  ( -1.778240108872766143E-15, 62.00000000546238255, -32.49999999999999289 ) ) ;
#24879 = VECTOR ( 'NONE', #30330, 1000.000000000000000 ) ;
#24880 = CARTESIAN_POINT ( 'NONE',  ( 33.58253175000000113, 58.37500000273118417, -4.112674001490185761E-15 ) ) ;
#24881 = CARTESIAN_POINT ( 'NONE',  ( 20.08610463437158344, 34.70000000000001705, 27.64615127144129403 ) ) ;
#24882 = CARTESIAN_POINT ( 'NONE',  ( 32.50000000000000000, 37.09999999999999432, -10.55989012756945833 ) ) ;
#24883 = CARTESIAN_POINT ( 'NONE',  ( -18.94512977948576093, 11.82499999726882578, 13.76444248337722698 ) ) ;
#24884 = CARTESIAN_POINT ( 'NONE',  ( 27.16883889988624290, 73.92500000273119554, 19.73931689729373673 ) ) ;
#24885 = CARTESIAN_POINT ( 'NONE',  ( 5.779280353836490358E-15, 2.500000000000005329, 32.49999999999999289 ) ) ;
#24886 = CARTESIAN_POINT ( 'NONE',  ( -8.960552108402744065E-16, 80.87500000273118417, -14.63369212191046209 ) ) ;
#24887 = CARTESIAN_POINT ( 'NONE',  ( 10.37757302488624056, 66.77500000273117564, -31.93888565452638417 ) ) ;
#24888 = CARTESIAN_POINT ( 'NONE',  ( 2.897257156509938333E-15, 78.75000000546236834, 15.77193336357400710 ) ) ;
#24889 = VERTEX_POINT ( 'NONE', #21044 ) ;
#24890 = FACE_OUTER_BOUND ( 'NONE', #7106, .T. ) ;
#24891 = CARTESIAN_POINT ( 'NONE',  ( -27.95245687107222921, 66.57031250000000000, 2.498001805406602216E-13 ) ) ;
#24892 = DIRECTION ( 'NONE',  ( -1.000000000000000000, 0.000000000000000000, 0.000000000000000000 ) ) ;
#24893 = CARTESIAN_POINT ( 'NONE',  ( 20.75514604977249178, 47.82500000273117990, 28.56700777964553950 ) ) ;
#24894 = CARTESIAN_POINT ( 'NONE',  ( -33.58253175000000113, 1.475000002731190474, 10.91162601494193929 ) ) ;
#24895 = CARTESIAN_POINT ( 'NONE',  ( 27.16883889988624290, 62.17500000273119554, 19.73931689729373673 ) ) ;
#24896 = CARTESIAN_POINT ( 'NONE',  ( 6.988114217768294445, 51.81770833333332860, 26.07999730980477437 ) ) ;
#24897 =( BOUNDED_CURVE ( )  B_SPLINE_CURVE ( 2, ( #32602, #3623, #9263, #29685, #9101, #13758, #12703, #12014, #25232, #30711, #2058, #23003, #9786 ),
 .UNSPECIFIED., .F., .T. ) 
 B_SPLINE_CURVE_WITH_KNOTS ( ( 3, 2, 2, 2, 2, 2, 3 ),
 ( 0.09615384615384615918, 0.09743589743589743668, 0.1000000000000000056, 0.1025641025641025605, 0.1051282051282051294, 0.1076923076923076983, 0.1089743589743589758 ),
 .UNSPECIFIED. ) 
 CURVE ( )  GEOMETRIC_REPRESENTATION_ITEM ( )  RATIONAL_B_SPLINE_CURVE ( ( 0.9755282581475767101, 0.9755282581475768211, 1.000000000000000000, 0.9510565162951535312, 1.000000000000000000, 0.9510565162951535312, 1.000000000000000000, 0.9510565162951535312, 1.000000000000000000, 0.9510565162951535312, 1.000000000000000000, 0.9755282581475768211, 0.9755282581475768211 ) ) 
 REPRESENTATION_ITEM ( '' )  );
#24898 = CARTESIAN_POINT ( 'NONE',  ( 25.98046417659858420, 39.07590250092398065, 15.04653450569292872 ) ) ;
#24899 = CARTESIAN_POINT ( 'NONE',  ( 15.04653450569339945, 26.17409749907601935, 25.98046417659831775 ) ) ;
#24900 = CARTESIAN_POINT ( 'NONE',  ( -2.092463501923844636E-15, 70.00000000546239676, -34.17252228774368916 ) ) ;
#24901 = AXIS2_PLACEMENT_3D ( 'NONE', #14723, #9736, #30840 ) ;
#24902 = CARTESIAN_POINT ( 'NONE',  ( 13.91746825000000065, 71.77500000273117564, 4.522059556121114987 ) ) ;
#24903 =( BOUNDED_CURVE ( )  B_SPLINE_CURVE ( 2, ( #30269, #25307, #25131, #19817, #22229, #12257, #30096, #6603, #33007, #3862, #4027, #22734, #20168 ),
 .UNSPECIFIED., .F., .T. ) 
 B_SPLINE_CURVE_WITH_KNOTS ( ( 3, 2, 2, 2, 2, 2, 3 ),
 ( 0.5320512820512820484, 0.5333333333333333259, 0.5358974358974358809, 0.5384615384615384359, 0.5410256410256409909, 0.5435897435897435459, 0.5448717948717948234 ),
 .UNSPECIFIED. ) 
 CURVE ( )  GEOMETRIC_REPRESENTATION_ITEM ( )  RATIONAL_B_SPLINE_CURVE ( ( 0.9755282581475768211, 0.9755282581475768211, 1.000000000000000000, 0.9510565162951535312, 1.000000000000000000, 0.9510565162951535312, 1.000000000000000000, 0.9510565162951535312, 1.000000000000000000, 0.9510565162951535312, 1.000000000000000000, 0.9755282581475768211, 0.9755282581475768211 ) ) 
 REPRESENTATION_ITEM ( '' )  );
#24904 = CARTESIAN_POINT ( 'NONE',  ( 14.01125832528330051, 53.67409749907601935, 24.18731323226221974 ) ) ;
#24905 = CARTESIAN_POINT ( 'NONE',  ( -10.04305231718579172, 57.59999999999998721, -30.90933677959248982 ) ) ;
#24906 = CARTESIAN_POINT ( 'NONE',  ( -1.778240108872766143E-15, 35.49999999999998579, -32.49999999999999289 ) ) ;
#24907 = ORIENTED_EDGE ( 'NONE', *, *, #3887, .T. ) ;
#24908 = CARTESIAN_POINT ( 'NONE',  ( 27.16883889988623935, 38.57500000273118701, -19.73931689729374384 ) ) ;
#24909 = CARTESIAN_POINT ( 'NONE',  ( -5.147494310547418017, 75.55125428154684641, -32.50000000000000000 ) ) ;
#24910 = CARTESIAN_POINT ( 'NONE',  ( 10.04305231718579705, 33.10000000546238397, 30.90933677959248982 ) ) ;
#24911 = VERTEX_POINT ( 'NONE', #33905 ) ;
#24912 = CARTESIAN_POINT ( 'NONE',  ( -20.50609665441004736, 32.62500000000000000, -20.50609665440969565 ) ) ;
#24913 = ORIENTED_EDGE ( 'NONE', *, *, #15322, .F. ) ;
#24914 = ORIENTED_EDGE ( 'NONE', *, *, #2379, .F. ) ;
#24915 = CARTESIAN_POINT ( 'NONE',  ( 26.29305231718578995, 27.20000000000000284, -19.10302069950538240 ) ) ;
#24916 = CARTESIAN_POINT ( 'NONE',  ( -2.162160676586881955E-15, 46.62500000273119127, -35.31076352940723240 ) ) ;
#24917 = CARTESIAN_POINT ( 'NONE',  ( 20.50609665440969565, 60.98437499999999289, -20.50609665441004736 ) ) ;
#24918 = CARTESIAN_POINT ( 'NONE',  ( 6.277390505771533514E-15, 15.00000000546237722, 34.17252228774368916 ) ) ;
#24919 = CARTESIAN_POINT ( 'NONE',  ( -10.37757302488623701, 65.52500000273118985, 31.93888565452638417 ) ) ;
#24920 = CARTESIAN_POINT ( 'NONE',  ( -14.47279130897151767, 15.82499999726881512, -19.92008829642072598 ) ) ;
#24921 = CARTESIAN_POINT ( 'NONE',  ( 20.08610463437157279, 51.29999999999997584, -27.64615127144129758 ) ) ;
#24922 = DIRECTION ( 'NONE',  ( 0.000000000000000000, 0.000000000000000000, 1.000000000000000000 ) ) ;
#24923 = CARTESIAN_POINT ( 'NONE',  ( 6.486482029760649416E-15, 21.87500000273118062, 35.31076352940723240 ) ) ;
#24924 = CARTESIAN_POINT ( 'NONE',  ( -5.147494310547423346, 24.94874572391553613, 32.50000000000000000 ) ) ;
#24925 = CARTESIAN_POINT ( 'NONE',  ( 7.025853678916867295, 19.44232666574268364, 26.06988505166722803 ) ) ;
#24926 = CARTESIAN_POINT ( 'NONE',  ( -8.601468415847518756, 74.57500000273117280, -11.83890561707634781 ) ) ;
#24927 = CARTESIAN_POINT ( 'NONE',  ( 5.779280353836490358E-15, 36.49999999999998579, 32.49999999999999289 ) ) ;
#24928 = CARTESIAN_POINT ( 'NONE',  ( -32.50000000000000000, 28.50000000546237899, 0.000000000000000000 ) ) ;
#24929 = CARTESIAN_POINT ( 'NONE',  ( -20.08610463437156923, 4.299999999999994493, 27.64615127144130113 ) ) ;
#24930 = ORIENTED_EDGE ( 'NONE', *, *, #13366, .F. ) ;
#24931 = CARTESIAN_POINT ( 'NONE',  ( -14.47279130897152122, 8.424999997268816543, 19.92008829642072243 ) ) ;
#24932 = DIRECTION ( 'NONE',  ( -0.000000000000000000, -1.000000000000000000, -0.000000000000000000 ) ) ;
#24933 = CARTESIAN_POINT ( 'NONE',  ( -24.20753774853730889, 42.22135416666666430, 13.97622843553633842 ) ) ;
#24934 = CARTESIAN_POINT ( 'NONE',  ( -20.75514604977248823, 66.82500000273118701, -28.56700777964554305 ) ) ;
#24935 = CARTESIAN_POINT ( 'NONE',  ( -27.16883889988623935, 25.57500000273120477, 19.73931689729374739 ) ) ;
#24936 = CARTESIAN_POINT ( 'NONE',  ( 6.486482029760649416E-15, 19.87500000273119483, 35.31076352940723240 ) ) ;
#24937 = CARTESIAN_POINT ( 'NONE',  ( -33.58253175000000113, 9.375000002731169957, 0.000000000000000000 ) ) ;
#24938 = CARTESIAN_POINT ( 'NONE',  ( -25.98046417659859486, 13.29465250092397532, -15.04653450569291628 ) ) ;
#24939 = CARTESIAN_POINT ( 'NONE',  ( -15.01150461594642138, 56.83072916666665009, -26.00068869287340334 ) ) ;
#24940 = EDGE_CURVE ( 'NONE', #27857, #5086, #25434, .T. ) ;
#24941 = CARTESIAN_POINT ( 'NONE',  ( 13.91746824999999532, 76.47500000273117848, -4.522059556121118540 ) ) ;
#24942 = CARTESIAN_POINT ( 'NONE',  ( -32.50000000000000000, 46.00000000000000000, 0.000000000000000000 ) ) ;
#24943 = VECTOR ( 'NONE', #9306, 1000.000000000000000 ) ;
#24944 = CARTESIAN_POINT ( 'NONE',  ( -15.14183272437242067, 2.449999994537622960, -20.84094480462497856 ) ) ;
#24945 = CARTESIAN_POINT ( 'NONE',  ( -27.16883889988624290, 52.92500000273120264, -19.73931689729374028 ) ) ;
#24946 = EDGE_CURVE ( 'NONE', #4618, #33963, #22710, .T. ) ;
#24947 = CARTESIAN_POINT ( 'NONE',  ( 1.507698388325705758E-15, 1.124999997268814722, -24.62258325217400312 ) ) ;
#24948 = ORIENTED_EDGE ( 'NONE', *, *, #27898, .F. ) ;
#24949 = CARTESIAN_POINT ( 'NONE',  ( 10.37757302488624056, 62.77500000273118985, -31.93888565452638417 ) ) ;
#24950 = CARTESIAN_POINT ( 'NONE',  ( 5.147494310547426899, 17.44874571845315359, -32.50000000000000000 ) ) ;
#24951 = CARTESIAN_POINT ( 'NONE',  ( 14.47279130897151767, 12.92499999726881832, -19.92008829642072598 ) ) ;
#24952 = CARTESIAN_POINT ( 'NONE',  ( 27.95245687107223986, 31.91444416759064495, 0.04044903254993640479 ) ) ;
#24953 = ORIENTED_EDGE ( 'NONE', *, *, #9492, .F. ) ;
#24954 = CARTESIAN_POINT ( 'NONE',  ( -33.58253175000000113, 31.02500000273118630, -10.91162601494193218 ) ) ;
#24955 = CARTESIAN_POINT ( 'NONE',  ( -12.13525491562420910, 74.19999999999998863, 8.816778784387098611 ) ) ;
#24956 = ORIENTED_EDGE ( 'NONE', *, *, #1024, .F. ) ;
#24957 = CARTESIAN_POINT ( 'NONE',  ( -20.50609665440969209, 59.26562500000000000, 20.50609665441005092 ) ) ;
#24958 = CARTESIAN_POINT ( 'NONE',  ( 27.16883889988623935, 58.57500000273119412, -19.73931689729374384 ) ) ;
#24959 =( GEOMETRIC_REPRESENTATION_CONTEXT ( 3 ) GLOBAL_UNCERTAINTY_ASSIGNED_CONTEXT ( ( #33516 ) ) GLOBAL_UNIT_ASSIGNED_CONTEXT ( ( #16877, #3495, #27676 ) ) REPRESENTATION_CONTEXT ( 'NONE', 'WORKASPACE' ) );
#24960 = DIRECTION ( 'NONE',  ( -0.000000000000000000, -1.000000000000000000, -0.000000000000000000 ) ) ;
#24961 = CARTESIAN_POINT ( 'NONE',  ( 6.486482029760649416E-15, 67.62500000273119838, 35.31076352940723240 ) ) ;
#24962 = VECTOR ( 'NONE', #31992, 1000.000000000000000 ) ;
#24963 = CARTESIAN_POINT ( 'NONE',  ( -28.01184896238290278, 32.05208333333332860, 7.505752307973363457 ) ) ;
#24964 = CARTESIAN_POINT ( 'NONE',  ( -24.50000000000000000, 15.00000000000001421, -3.000384657911015469E-15 ) ) ;
#24965 = CARTESIAN_POINT ( 'NONE',  ( 33.58253175000000113, 4.375000002731193938, -4.112674001490185761E-15 ) ) ;
#24966 = CARTESIAN_POINT ( 'NONE',  ( -27.16883889988624290, 18.92500000273117422, -19.73931689729374028 ) ) ;
#24967 = CARTESIAN_POINT ( 'NONE',  ( 5.779280353836490358E-15, 1.000000005462375885, 32.49999999999999289 ) ) ;
#24968 = CARTESIAN_POINT ( 'NONE',  ( 20.53372385742108008, 46.65586833240934794, 20.47846945139866648 ) ) ;
#24969 = CARTESIAN_POINT ( 'NONE',  ( -4.635254915624211769, 81.60000000000000853, -14.26584774442730286 ) ) ;
#24970 = CARTESIAN_POINT ( 'NONE',  ( -15.01150461594595775, 59.12239583333333570, 26.00068869287368756 ) ) ;
#24971 = FACE_OUTER_BOUND ( 'NONE', #20200, .T. ) ;
#24972 = CARTESIAN_POINT ( 'NONE',  ( 24.50000000000000000, 3.749999994537622783, 0.000000000000000000 ) ) ;
#24973 = CARTESIAN_POINT ( 'NONE',  ( 4.635254915624212657, 74.85000000546237686, 14.26584774442730286 ) ) ;
#24974 = CARTESIAN_POINT ( 'NONE',  ( 26.07999730980490227, 13.43229166666666607, 6.988114217767821046 ) ) ;
#24975 = CARTESIAN_POINT ( 'NONE',  ( -10.37757302488624411, 36.72500000273118559, -31.93888565452638417 ) ) ;
#24976 = CARTESIAN_POINT ( 'NONE',  ( -11.25946833292375793, 74.67500000273119554, -8.180482586598733619 ) ) ;
#24977 = CARTESIAN_POINT ( 'NONE',  ( -27.16883889988624290, 51.17500000273118843, -19.73931689729374028 ) ) ;
#24978 = CARTESIAN_POINT ( 'NONE',  ( -10.37757302488624411, 26.97500000273117493, -31.93888565452638417 ) ) ;
#24979 = CARTESIAN_POINT ( 'NONE',  ( -10.04305231718579172, 12.10000000546238041, -30.90933677959248982 ) ) ;
#24980 = CARTESIAN_POINT ( 'NONE',  ( -32.50000000000000000, 8.400000005462382902, -10.55989012756945300 ) ) ;
#24981 = EDGE_CURVE ( 'NONE', #24889, #27958, #17919, .T. ) ;
#24982 = FACE_OUTER_BOUND ( 'NONE', #6600, .T. ) ;
#24983 = CARTESIAN_POINT ( 'NONE',  ( 10.04305231718578817, 65.40000000000000568, -30.90933677959249337 ) ) ;
#24984 = AXIS2_PLACEMENT_3D ( 'NONE', #9657, #19621, #20137 ) ;
#24985 = CARTESIAN_POINT ( 'NONE',  ( 23.41746824999999887, 10.62499999726881938, 0.000000000000000000 ) ) ;
#24986 = CARTESIAN_POINT ( 'NONE',  ( -15.04653450569338524, 21.01784749907601579, -25.98046417659831775 ) ) ;
#24987 = EDGE_CURVE ( 'NONE', #11703, #6044, #19209, .T. ) ;
#24988 = CARTESIAN_POINT ( 'NONE',  ( -23.41746825000000243, 2.024999997268815299, -7.608796670333730638 ) ) ;
#24989 = CARTESIAN_POINT ( 'NONE',  ( -0.04044903255042732459, 35.05430583240935505, -27.95245687107223986 ) ) ;
#24990 = CARTESIAN_POINT ( 'NONE',  ( 20.75514604977248467, 78.67500000273116711, -28.56700777964554305 ) ) ;
#24991 = CARTESIAN_POINT ( 'NONE',  ( -33.58253175000000113, 11.12500000273120015, 0.000000000000000000 ) ) ;
#24992 = CARTESIAN_POINT ( 'NONE',  ( 7.236395654485755280, 12.72499999726881015, 22.27133577429736988 ) ) ;
#24993 = CARTESIAN_POINT ( 'NONE',  ( 24.20753774853756113, 58.26302083333332149, 13.97622843553589789 ) ) ;
#24994 = VERTEX_POINT ( 'NONE', #7636 ) ;
#24995 = CARTESIAN_POINT ( 'NONE',  ( -27.16883889988624290, 46.92500000273118133, -19.73931689729374028 ) ) ;
#24996 = CARTESIAN_POINT ( 'NONE',  ( -27.16883889988624290, 25.17500000273119198, -19.73931689729374028 ) ) ;
#24997 =( BOUNDED_CURVE ( )  B_SPLINE_CURVE ( 2, ( #21112, #10128, #5483, #20778, #5313, #7547, #18372 ),
 .UNSPECIFIED., .F., .T. ) 
 B_SPLINE_CURVE_WITH_KNOTS ( ( 3, 2, 2, 3 ),
 ( 0.000000000000000000, 0.02000000000000000042, 0.04000000000000000083, 0.05000000000000000971 ),
 .UNSPECIFIED. ) 
 CURVE ( )  GEOMETRIC_REPRESENTATION_ITEM ( )  RATIONAL_B_SPLINE_CURVE ( ( 1.000000000000000000, 0.9510565162951535312, 1.000000000000000000, 0.9510565162951535312, 1.000000000000000000, 0.9755282581475768211, 0.9755282581475768211 ) ) 
 REPRESENTATION_ITEM ( '' )  );
#24998 = ORIENTED_EDGE ( 'NONE', *, *, #20285, .T. ) ;
#24999 = CARTESIAN_POINT ( 'NONE',  ( 20.50609665440969565, 30.04687500000000000, -20.50609665441004736 ) ) ;
#25000 = CARTESIAN_POINT ( 'NONE',  ( -26.02091320914849959, 29.90923583425730925, 14.97647472619947528 ) ) ;
#25001 = CARTESIAN_POINT ( 'NONE',  ( -24.50000000000000000, 8.749999994537628112, -3.000384657911015469E-15 ) ) ;
#25002 = CARTESIAN_POINT ( 'NONE',  ( -4.732186688966233175E-15, 19.24999999453764232, 25.76082449383753925 ) ) ;
#25003 = CARTESIAN_POINT ( 'NONE',  ( 23.41746825000000243, 6.524999997268818852, 7.608796670333735079 ) ) ;
#25004 = CARTESIAN_POINT ( 'NONE',  ( -20.75514604977248112, 21.67500000273119554, 28.56700777964554661 ) ) ;
#25005 = CARTESIAN_POINT ( 'NONE',  ( 6.277390505771533514E-15, 23.00000000546238610, 34.17252228774368916 ) ) ;
#25006 = CARTESIAN_POINT ( 'NONE',  ( 10.04305231718578817, 71.40000000000001990, -30.90933677959249337 ) ) ;
#25007 = CARTESIAN_POINT ( 'NONE',  ( 5.779280353836490358E-15, 33.00000000546238965, 32.49999999999999289 ) ) ;
#25008 = CARTESIAN_POINT ( 'NONE',  ( -16.87750156402132617, 66.99999999999998579, -29.11635311643979662 ) ) ;
#25009 = CARTESIAN_POINT ( 'NONE',  ( -28.00173670424549499, 57.83892333425730214, -7.543491769121417612 ) ) ;
#25010 = CARTESIAN_POINT ( 'NONE',  ( 33.58253175000000113, 36.47500000273119269, -10.91162601494193751 ) ) ;
#25011 = CARTESIAN_POINT ( 'NONE',  ( -2.162160676586882350E-15, 54.62500000273116996, -35.31076352940722529 ) ) ;
#25012 = CARTESIAN_POINT ( 'NONE',  ( 20.50609665441005092, 30.90624999999999645, 20.50609665440969209 ) ) ;
#25013 =( NAMED_UNIT ( * ) SI_UNIT ( $, .STERADIAN. ) SOLID_ANGLE_UNIT ( ) );
#25014 = AXIS2_PLACEMENT_3D ( 'NONE', #26601, #2589, #26263 ) ;
#25015 = CARTESIAN_POINT ( 'NONE',  ( -23.41746824999999887, 12.12499999726882116, -2.867812753649727150E-15 ) ) ;
#25016 = CARTESIAN_POINT ( 'NONE',  ( -32.50000000000000000, 14.09999999999999254, 10.55989012756946366 ) ) ;
#25017 = CARTESIAN_POINT ( 'NONE',  ( -1.089172066684569321E-14, 76.75000000546238255, 15.00000000000000000 ) ) ;
#25018 = CARTESIAN_POINT ( 'NONE',  ( 0.04044903255044120238, 43.64805583240936215, 27.95245687107223276 ) ) ;
#25019 = CARTESIAN_POINT ( 'NONE',  ( 6.486482029760649416E-15, 57.62500000273119127, 35.31076352940723240 ) ) ;
#25020 = CARTESIAN_POINT ( 'NONE',  ( -33.58253175000000113, 47.27500000273116854, -10.91162601494193041 ) ) ;
#25021 = CARTESIAN_POINT ( 'NONE',  ( 32.50000000000000711, 44.90000000000001279, 10.55989012756945122 ) ) ;
#25022 = FACE_OUTER_BOUND ( 'NONE', #21554, .T. ) ;
#25023 = DIRECTION ( 'NONE',  ( -1.224646799147353454E-16, 1.000000000000000000, -0.000000000000000000 ) ) ;
#25024 = CARTESIAN_POINT ( 'NONE',  ( 14.01125832528286352, 51.96652750092398065, -24.18731323226246843 ) ) ;
#25025 = CARTESIAN_POINT ( 'NONE',  ( 21.64573397815488676, 16.99999999999998579, 8.935324268693841887 ) ) ;
#25026 = CARTESIAN_POINT ( 'NONE',  ( -4.223320258572819786E-15, 3.500000000000004441, 24.50000000000000000 ) ) ;
#25027 = CARTESIAN_POINT ( 'NONE',  ( -10.37757302488624411, 18.72500000273118204, -31.93888565452638417 ) ) ;
#25028 = FACE_OUTER_BOUND ( 'NONE', #6030, .T. ) ;
#25029 = DIRECTION ( 'NONE',  ( 0.7069718413157916048, 0.01953538259431456675, -0.7069718413158002646 ) ) ;
#25030 = CARTESIAN_POINT ( 'NONE',  ( 0.000000000000000000, 80.00000000000001421, -32.50000000000000000 ) ) ;
#25031 = CARTESIAN_POINT ( 'NONE',  ( 28.00173670424535644, 63.27045166574269075, -7.543491769121920321 ) ) ;
#25032 = CARTESIAN_POINT ( 'NONE',  ( -20.08610463437157989, 40.20000000546235697, -27.64615127144129758 ) ) ;
#25033 = CARTESIAN_POINT ( 'NONE',  ( 15.00000000000000000, 71.25000000546238255, -1.836970198721029589E-15 ) ) ;
#25034 = CARTESIAN_POINT ( 'NONE',  ( 27.16883889988623935, 34.32500000273120122, -19.73931689729374384 ) ) ;
#25035 = CARTESIAN_POINT ( 'NONE',  ( 10.37757302488624767, 65.97500000273119269, 31.93888565452638417 ) ) ;
#25036 = CARTESIAN_POINT ( 'NONE',  ( 26.07999730980490227, 34.05729166666666430, 6.988114217767821046 ) ) ;
#25037 = ORIENTED_EDGE ( 'NONE', *, *, #2221, .F. ) ;
#25038 = CARTESIAN_POINT ( 'NONE',  ( 33.58253175000000823, 66.02500000273118985, 10.91162601494192863 ) ) ;
#25039 = CARTESIAN_POINT ( 'NONE',  ( 26.00068869287367335, 44.51302083333331439, 15.01150461594596308 ) ) ;
#25040 = CARTESIAN_POINT ( 'NONE',  ( 0.000000000000000000, -20.99999999999998934, 0.000000000000000000 ) ) ;
#25041 = ORIENTED_EDGE ( 'NONE', *, *, #26052, .F. ) ;
#25042 = CARTESIAN_POINT ( 'NONE',  ( 20.53372385742072481, 52.10975666759065206, -20.47846945139902175 ) ) ;
#25043 = CARTESIAN_POINT ( 'NONE',  ( -26.29305231718578995, 8.700000005462380059, 19.10302069950538595 ) ) ;
#25044 = AXIS2_PLACEMENT_3D ( 'NONE', #22382, #1259, #6761 ) ;
#25045 = CARTESIAN_POINT ( 'NONE',  ( 7.505752307973351023, 58.69270833333332860, 28.01184896238290278 ) ) ;
#25046 = CARTESIAN_POINT ( 'NONE',  ( 10.04305231718578817, 57.40000000000000568, -30.90933677959249337 ) ) ;
#25047 = CARTESIAN_POINT ( 'NONE',  ( -10.37757302488624411, 40.97500000273118559, -31.93888565452638417 ) ) ;
#25048 = CARTESIAN_POINT ( 'NONE',  ( 6.277390505771533514E-15, 43.00000000546236123, 34.17252228774368916 ) ) ;
#25049 = CARTESIAN_POINT ( 'NONE',  ( -4.635254915624208216, 80.39999999999997726, 14.26584774442730463 ) ) ;
#25050 = CARTESIAN_POINT ( 'NONE',  ( -2.162160676586881955E-15, 30.62500000273119838, -35.31076352940723240 ) ) ;
#25051 = CARTESIAN_POINT ( 'NONE',  ( -32.50000000000000000, 23.99999999999999289, 0.000000000000000000 ) ) ;
#25052 = CARTESIAN_POINT ( 'NONE',  ( 27.16883889988624290, 54.17500000273117422, 19.73931689729373673 ) ) ;
#25053 = CARTESIAN_POINT ( 'NONE',  ( -20.08610463437157989, 33.70000000000001705, -27.64615127144129758 ) ) ;
#25054 = CARTESIAN_POINT ( 'NONE',  ( 32.50000000000000711, 32.89999999999997726, 10.55989012756945122 ) ) ;
#25055 = CARTESIAN_POINT ( 'NONE',  ( 15.14183272437241889, 1.700000000000004396, 20.84094480462498211 ) ) ;
#25056 = CARTESIAN_POINT ( 'NONE',  ( 27.16883889988624290, 77.92500000273116711, 19.73931689729373673 ) ) ;
#25057 = CARTESIAN_POINT ( 'NONE',  ( 0.000000000000000000, 122.0000000000000000, -9.000000000000001776 ) ) ;
#25058 = CARTESIAN_POINT ( 'NONE',  ( 4.300734207923757602, 76.77500000273118985, -13.23629886949340673 ) ) ;
#25059 = CARTESIAN_POINT ( 'NONE',  ( 27.16883889988623935, 68.57500000273120122, -19.73931689729374384 ) ) ;
#25060 = CARTESIAN_POINT ( 'NONE',  ( 4.635254915624212657, 78.85000000546239107, 14.26584774442730286 ) ) ;
#25061 = ORIENTED_EDGE ( 'NONE', *, *, #18602, .F. ) ;
#25062 = DIRECTION ( 'NONE',  ( -0.000000000000000000, 1.000000000000000000, -0.000000000000000000 ) ) ;
#25063 = CARTESIAN_POINT ( 'NONE',  ( 27.95245687107223986, 21.60194416759064495, 0.04044903254993640479 ) ) ;
#25064 = CARTESIAN_POINT ( 'NONE',  ( 24.50000000000000000, 7.649999994537632908, 7.960532557706212486 ) ) ;
#25065 = CARTESIAN_POINT ( 'NONE',  ( -2.162160676586881955E-15, 38.62500000273118417, -35.31076352940723240 ) ) ;
#25066 = CARTESIAN_POINT ( 'NONE',  ( 27.16883889988623935, 6.575000002731187898, -19.73931689729374384 ) ) ;
#25067 = CARTESIAN_POINT ( 'NONE',  ( -33.58253175000000113, 57.37500000273119838, 0.000000000000000000 ) ) ;
#25068 = CARTESIAN_POINT ( 'NONE',  ( -13.97622843553588901, 55.68489583333332860, 24.20753774853756823 ) ) ;
#25069 = CARTESIAN_POINT ( 'NONE',  ( 7.468012846824777284, 42.94309000092397355, 28.02196122052045268 ) ) ;
#25070 = CARTESIAN_POINT ( 'NONE',  ( -20.47846945139866648, 33.76524333240934084, 20.53372385742108008 ) ) ;
#25071 = CARTESIAN_POINT ( 'NONE',  ( 32.50000000000000711, 69.40000000546235981, 10.55989012756945122 ) ) ;
#25072 = CARTESIAN_POINT ( 'NONE',  ( -8.601468415847515203, 73.17500000273119554, 11.83890561707634959 ) ) ;
#25073 = CARTESIAN_POINT ( 'NONE',  ( 6.950374756619257965, 55.82253499907601935, -26.09010956794244507 ) ) ;
#25074 = CARTESIAN_POINT ( 'NONE',  ( -34.92499999999992610, 0.000000000000000000, 0.000000000000000000 ) ) ;
#25075 = EDGE_CURVE ( 'NONE', #8792, #16699, #6249, .T. ) ;
#25076 = CARTESIAN_POINT ( 'NONE',  ( -10.37757302488624411, 42.97500000273117848, -31.93888565452638417 ) ) ;
#25077 = CARTESIAN_POINT ( 'NONE',  ( -23.41746824999999887, 2.124999997268811391, -2.867812753649727150E-15 ) ) ;
#25078 = VERTEX_POINT ( 'NONE', #2317 ) ;
#25079 = CARTESIAN_POINT ( 'NONE',  ( 10.04305231718579705, 29.10000000546238041, 30.90933677959248982 ) ) ;
#25080 = ORIENTED_EDGE ( 'NONE', *, *, #16923, .F. ) ;
#25081 = ADVANCED_FACE ( 'NONE', ( #12790 ), #23264, .T. ) ;
#25082 = ADVANCED_FACE ( 'NONE', ( #9523 ), #7289, .T. ) ;
#25083 = CARTESIAN_POINT ( 'NONE',  ( 30.02300923189239512, 30.47656250000000355, -2.619432448724977703E-13 ) ) ;
#25084 = CARTESIAN_POINT ( 'NONE',  ( 32.50000000000000000, 61.50000000546238255, -3.980102097228898626E-15 ) ) ;
#25085 = EDGE_LOOP ( 'NONE', ( #26983, #15358, #16990, #12343 ) ) ;
#25086 = CARTESIAN_POINT ( 'NONE',  ( -12.11000150615021553, -45.00000000000001421, 1.679354548928025724E-15 ) ) ;
#25087 = CARTESIAN_POINT ( 'NONE',  ( -33.58253175000000113, 51.02500000273119696, -10.91162601494193218 ) ) ;
#25088 = CARTESIAN_POINT ( 'NONE',  ( 20.08610463437158344, 55.20000000546238539, 27.64615127144129403 ) ) ;
#25089 = DIRECTION ( 'NONE',  ( -1.000000000000000000, 0.000000000000000000, 0.000000000000000000 ) ) ;
#25090 = CARTESIAN_POINT ( 'NONE',  ( 26.29305231718579350, 13.30000000546238681, 19.10302069950537529 ) ) ;
#25091 = EDGE_CURVE ( 'NONE', #19067, #7360, #9572, .T. ) ;
#25092 = CARTESIAN_POINT ( 'NONE',  ( -27.16883889988623935, 65.32500000273118701, 19.73931689729374739 ) ) ;
#25093 = CARTESIAN_POINT ( 'NONE',  ( -18.94512977948575738, 17.92499999726882010, -13.76444248337723231 ) ) ;
#25094 = AXIS2_PLACEMENT_3D ( 'NONE', #24484, #628, #958 ) ;
#25095 = CARTESIAN_POINT ( 'NONE',  ( 6.277390505771533514E-15, 50.50000000000000000, 34.17252228774368916 ) ) ;
#25096 = CARTESIAN_POINT ( 'NONE',  ( 7.570916362186207671, 1.599999999999990319, 23.30088464923126779 ) ) ;
#25097 = CARTESIAN_POINT ( 'NONE',  ( 27.16883889988624290, 20.17500000273120264, 19.73931689729373673 ) ) ;
#25098 = CARTESIAN_POINT ( 'NONE',  ( 15.00000000000000000, 77.09999999999998010, -4.873795443493596835 ) ) ;
#25099 = CARTESIAN_POINT ( 'NONE',  ( 26.09010956794244507, 25.74440999907601935, 6.950374756619249084 ) ) ;
#25100 = CARTESIAN_POINT ( 'NONE',  ( 13.91746825000000065, 71.77500000273120406, 4.522059556121114987 ) ) ;
#25101 = CARTESIAN_POINT ( 'NONE',  ( -3.880418787951142701, 13.44874571845315536, 24.49999999999999645 ) ) ;
#25102 = CARTESIAN_POINT ( 'NONE',  ( -32.50000000000000000, 22.09999999999999787, 10.55989012756946366 ) ) ;
#25103 =( BOUNDED_SURFACE ( )  B_SPLINE_SURFACE ( 1, 2, ( 
 ( #15801, #7722, #13209, #13047, #23519, #28484, #10640, #33978, #20950, #31562, #31399, #7889, #26257, #5490, #15969, #13386, #23859, #4378, #14853, #14513, #24972, #25319, #12271, #33019, #1620, #32850, #3253, #29324, #1454, #27551, #22745, #19665, #6950, #13723, #6614, #9345, #6452, #18875, #4211, #19500, #11933, #20006, #30110, #22241, #33196, #9525, #30453, #30280, #5826, #4039, #17434, #24188, #27895, #27723, #29948, #1793, #9181, #14683, #16926, #27384, #3873, #22402, #17092, #19828, #6782, #16305, #17260, #660, #9018, #26761, #25144, #11148, #22074, #12098, #32519, #14347, #24803, #22569, #1281, #11760, #32686, #28741, #5237, #4894, #15374, #15721, #2670, #23437, #26001, #23266, #28063, #28404, #12792, #33728, #20348, #7473, #10226, #30973, #7119, #7807, #7639, #12449, #17955, #26176, #10389, #15200, #4550, #13129, #22919, #20706, #33548, #25829, #20530, #2319, #31148, #15029, #25494, #18123, #17601, #28568, #33375, #5064, #15549, #23603, #2494, #9870, #12963, #33898, #20867, #31315, #10049, #30798, #18296, #9699, #20179, #30623, #25664, #1974, #2143, #7291, #23085, #17776, #28234, #4720, #12618, #18966, #21037, #5746, #29410, #13971, #3007, #3177, #28907, #70, #18636, #13808, #16389, #13646, #18463, #18798, #24110, #578, #10728, #31816, #11068, #21372, #31487, #32151, #31982, #2832, #8307, #16550, #744, #5577, #5408, #19129, #13301, #21534, #23944, #16227, #10899 ),
 ( #29073, #15887, #13479, #8479, #29566, #26343, #24276, #7977, #26681, #6067, #26513, #5912, #413, #10558, #23776, #26842, #242, #3337, #21205, #31649, #8147, #11229, #21705, #29242, #27003, #8644, #16058, #3501, #19967, #27175, #14647, #1241, #1582, #9305, #17224, #14142, #19789, #27858, #3833, #27513, #27683, #16884, #4173, #32317, #14474, #4340, #29909, #6239, #11390, #14307, #30413, #32980, #19291, #32812, #24434, #4001, #19461, #27347, #24763, #24598, #21867, #9484, #6913, #25106, #8808, #17394, #8979, #1072, #22202, #6577, #17051, #6412, #11552, #24931, #11719, #30238, #12059, #16720, #22365, #1416, #32649, #22529, #3668, #6743, #911, #29734, #22034, #32478, #11894, #9143, #19626, #30071, #25628, #28368, #30586, #10014, #12409, #25791, #4511, #17916, #2280, #10354, #12755, #14985, #20668, #31108, #7602, #4856, #15162, #25455, #18082, #2456, #28703, #30936, #20310, #20485, #30760, #12922, #28195, #23227, #1752, #23050, #12580, #33686, #12232, #7429, #10185, #14814, #17737, #15336, #9661, #25279, #33336, #22706, #28530, #33509, #7770, #2107, #23399, #20142, #5025, #15510, #1931, #33158, #25962, #22879, #33860, #20832, #31277, #4683, #7082, #18257, #17566, #28023, #9833, #7250, #5871, #10521, #29372, #13608, #15849, #21662, #29035, #539, #26305, #5368, #2794, #8268, #26473, #2967, #13436, #15684, #23903, #23567, #28872, #32107, #375, #3300, #26134, #10860, #18925 ) ),
 .UNSPECIFIED., .F., .F., .T. ) 
 B_SPLINE_SURFACE_WITH_KNOTS ( ( 2, 2 ),
 ( 3, 2, 2, 2, 2, 2, 2, 2, 2, 2, 2, 2, 2, 2, 2, 2, 2, 2, 2, 2, 2, 2, 2, 2, 2, 2, 2, 2, 2, 2, 2, 2, 2, 2, 2, 2, 2, 2, 2, 2, 2, 2, 2, 2, 2, 2, 2, 2, 2, 2, 2, 2, 2, 2, 2, 2, 2, 2, 2, 2, 2, 2, 2, 2, 2, 2, 2, 2, 2, 2, 2, 2, 2, 2, 2, 2, 2, 2, 2, 2, 2, 2, 2, 2, 2, 2, 2, 2, 2, 2, 3 ),
 ( 0.000000000000000000, 1.000000000000000000 ),
 ( 0.000000000000000000, 0.01111111111111111154, 0.02222222222222222307, 0.03333333333333333287, 0.04444444444444444614, 0.05555555555555555247, 0.06666666666666666574, 0.07777777777777777901, 0.08888888888888889228, 0.1000000000000000056, 0.1111111111111111049, 0.1222222222222222182, 0.1333333333333333315, 0.1444444444444444309, 0.1555555555555555580, 0.1666666666666666574, 0.1777777777777777846, 0.1888888888888888840, 0.2000000000000000111, 0.2111111111111111105, 0.2222222222222222099, 0.2333333333333333370, 0.2444444444444444364, 0.2555555555555555358, 0.2666666666666666630, 0.2777777777777777901, 0.2888888888888888618, 0.2999999999999999889, 0.3111111111111111160, 0.3222222222222222432, 0.3333333333333333148, 0.3444444444444444420, 0.3555555555555555691, 0.3666666666666666408, 0.3777777777777777679, 0.3888888888888888951, 0.4000000000000000222, 0.4111111111111110938, 0.4222222222222222210, 0.4333333333333333481, 0.4444444444444444198, 0.4555555555555555469, 0.4666666666666666741, 0.4777777777777778012, 0.4888888888888888729, 0.5000000000000000000, 0.5111111111111110716, 0.5222222222222222543, 0.5333333333333333259, 0.5444444444444443976, 0.5555555555555555802, 0.5666666666666666519, 0.5777777777777777235, 0.5888888888888889062, 0.5999999999999999778, 0.6111111111111111605, 0.6222222222222222321, 0.6333333333333333037, 0.6444444444444444864, 0.6555555555555555580, 0.6666666666666666297, 0.6777777777777778123, 0.6888888888888888840, 0.6999999999999999556, 0.7111111111111111382, 0.7222222222222222099, 0.7333333333333332815, 0.7444444444444444642, 0.7555555555555555358, 0.7666666666666667185, 0.7777777777777777901, 0.7888888888888888618, 0.8000000000000000444, 0.8111111111111111160, 0.8222222222222221877, 0.8333333333333333703, 0.8444444444444444420, 0.8555555555555555136, 0.8666666666666666963, 0.8777777777777777679, 0.8888888888888888395, 0.9000000000000000222, 0.9111111111111110938, 0.9222222222222222765, 0.9333333333333333481, 0.9444444444444444198, 0.9555555555555556024, 0.9666666666666666741, 0.9777777777777777457, 0.9888888888888889284, 1.000000000000000000 ),
 .UNSPECIFIED. ) 
 GEOMETRIC_REPRESENTATION_ITEM ( )  RATIONAL_B_SPLINE_SURFACE ( (
 ( 1.000000000000000000, 0.9510565162951535312, 1.000000000000000000, 0.9510565162951535312, 1.000000000000000000, 0.9510565162951535312, 1.000000000000000000, 0.9510565162951535312, 1.000000000000000000, 0.9510565162951535312, 1.000000000000000000, 0.9510565162951535312, 1.000000000000000000, 0.9510565162951535312, 1.000000000000000000, 0.9510565162951535312, 1.000000000000000000, 0.9510565162951535312, 1.000000000000000000, 0.9510565162951535312, 1.000000000000000000, 0.9510565162951535312, 1.000000000000000000, 0.9510565162951535312, 1.000000000000000000, 0.9510565162951535312, 1.000000000000000000, 0.9510565162951535312, 1.000000000000000000, 0.9510565162951535312, 1.000000000000000000, 0.9510565162951535312, 1.000000000000000000, 0.9510565162951535312, 1.000000000000000000, 0.9510565162951535312, 1.000000000000000000, 0.9510565162951535312, 1.000000000000000000, 0.9510565162951535312, 1.000000000000000000, 0.9510565162951535312, 1.000000000000000000, 0.9510565162951535312, 1.000000000000000000, 0.9510565162951535312, 1.000000000000000000, 0.9510565162951535312, 1.000000000000000000, 0.9510565162951535312, 1.000000000000000000, 0.9510565162951535312, 1.000000000000000000, 0.9510565162951535312, 1.000000000000000000, 0.9510565162951535312, 1.000000000000000000, 0.9510565162951535312, 1.000000000000000000, 0.9510565162951535312, 1.000000000000000000, 0.9510565162951535312, 1.000000000000000000, 0.9510565162951535312, 1.000000000000000000, 0.9510565162951535312, 1.000000000000000000, 0.9510565162951535312, 1.000000000000000000, 0.9510565162951535312, 1.000000000000000000, 0.9510565162951535312, 1.000000000000000000, 0.9510565162951535312, 1.000000000000000000, 0.9510565162951535312, 1.000000000000000000, 0.9510565162951535312, 1.000000000000000000, 0.9510565162951535312, 1.000000000000000000, 0.9510565162951535312, 1.000000000000000000, 0.9510565162951535312, 1.000000000000000000, 0.9510565162951535312, 1.000000000000000000, 0.9510565162951535312, 1.000000000000000000, 0.9510565162951535312, 1.000000000000000000, 0.9510565162951535312, 1.000000000000000000, 0.9510565162951535312, 1.000000000000000000, 0.9510565162951535312, 1.000000000000000000, 0.9510565162951535312, 1.000000000000000000, 0.9510565162951535312, 1.000000000000000000, 0.9510565162951535312, 1.000000000000000000, 0.9510565162951535312, 1.000000000000000000, 0.9510565162951535312, 1.000000000000000000, 0.9510565162951535312, 1.000000000000000000, 0.9510565162951535312, 1.000000000000000000, 0.9510565162951535312, 1.000000000000000000, 0.9510565162951535312, 1.000000000000000000, 0.9510565162951535312, 1.000000000000000000, 0.9510565162951535312, 1.000000000000000000, 0.9510565162951535312, 1.000000000000000000, 0.9510565162951535312, 1.000000000000000000, 0.9510565162951535312, 1.000000000000000000, 0.9510565162951535312, 1.000000000000000000, 0.9510565162951535312, 1.000000000000000000, 0.9510565162951535312, 1.000000000000000000, 0.9510565162951535312, 1.000000000000000000, 0.9510565162951535312, 1.000000000000000000, 0.9510565162951535312, 1.000000000000000000, 0.9510565162951535312, 1.000000000000000000, 0.9510565162951535312, 1.000000000000000000, 0.9510565162951535312, 1.000000000000000000, 0.9510565162951535312, 1.000000000000000000, 0.9510565162951535312, 1.000000000000000000, 0.9510565162951535312, 1.000000000000000000, 0.9510565162951535312, 1.000000000000000000, 0.9510565162951535312, 1.000000000000000000, 0.9510565162951535312, 1.000000000000000000, 0.9510565162951535312, 1.000000000000000000, 0.9510565162951535312, 1.000000000000000000, 0.9510565162951535312, 1.000000000000000000, 0.9510565162951535312, 1.000000000000000000, 0.9510565162951535312, 1.000000000000000000, 0.9510565162951535312, 1.000000000000000000, 0.9510565162951535312, 1.000000000000000000, 0.9510565162951535312, 1.000000000000000000, 0.9510565162951535312, 1.000000000000000000, 0.9510565162951535312, 1.000000000000000000, 0.9510565162951535312, 1.000000000000000000, 0.9510565162951535312, 1.000000000000000000, 0.9510565162951535312, 1.000000000000000000),
 ( 1.000000000000000000, 0.9510565162951535312, 1.000000000000000000, 0.9510565162951535312, 1.000000000000000000, 0.9510565162951535312, 1.000000000000000000, 0.9510565162951535312, 1.000000000000000000, 0.9510565162951535312, 1.000000000000000000, 0.9510565162951535312, 1.000000000000000000, 0.9510565162951535312, 1.000000000000000000, 0.9510565162951535312, 1.000000000000000000, 0.9510565162951535312, 1.000000000000000000, 0.9510565162951535312, 1.000000000000000000, 0.9510565162951535312, 1.000000000000000000, 0.9510565162951535312, 1.000000000000000000, 0.9510565162951535312, 1.000000000000000000, 0.9510565162951535312, 1.000000000000000000, 0.9510565162951535312, 1.000000000000000000, 0.9510565162951535312, 1.000000000000000000, 0.9510565162951535312, 1.000000000000000000, 0.9510565162951535312, 1.000000000000000000, 0.9510565162951535312, 1.000000000000000000, 0.9510565162951535312, 1.000000000000000000, 0.9510565162951535312, 1.000000000000000000, 0.9510565162951535312, 1.000000000000000000, 0.9510565162951535312, 1.000000000000000000, 0.9510565162951535312, 1.000000000000000000, 0.9510565162951535312, 1.000000000000000000, 0.9510565162951535312, 1.000000000000000000, 0.9510565162951535312, 1.000000000000000000, 0.9510565162951535312, 1.000000000000000000, 0.9510565162951535312, 1.000000000000000000, 0.9510565162951535312, 1.000000000000000000, 0.9510565162951535312, 1.000000000000000000, 0.9510565162951535312, 1.000000000000000000, 0.9510565162951535312, 1.000000000000000000, 0.9510565162951535312, 1.000000000000000000, 0.9510565162951535312, 1.000000000000000000, 0.9510565162951535312, 1.000000000000000000, 0.9510565162951535312, 1.000000000000000000, 0.9510565162951535312, 1.000000000000000000, 0.9510565162951535312, 1.000000000000000000, 0.9510565162951535312, 1.000000000000000000, 0.9510565162951535312, 1.000000000000000000, 0.9510565162951535312, 1.000000000000000000, 0.9510565162951535312, 1.000000000000000000, 0.9510565162951535312, 1.000000000000000000, 0.9510565162951535312, 1.000000000000000000, 0.9510565162951535312, 1.000000000000000000, 0.9510565162951535312, 1.000000000000000000, 0.9510565162951535312, 1.000000000000000000, 0.9510565162951535312, 1.000000000000000000, 0.9510565162951535312, 1.000000000000000000, 0.9510565162951535312, 1.000000000000000000, 0.9510565162951535312, 1.000000000000000000, 0.9510565162951535312, 1.000000000000000000, 0.9510565162951535312, 1.000000000000000000, 0.9510565162951535312, 1.000000000000000000, 0.9510565162951535312, 1.000000000000000000, 0.9510565162951535312, 1.000000000000000000, 0.9510565162951535312, 1.000000000000000000, 0.9510565162951535312, 1.000000000000000000, 0.9510565162951535312, 1.000000000000000000, 0.9510565162951535312, 1.000000000000000000, 0.9510565162951535312, 1.000000000000000000, 0.9510565162951535312, 1.000000000000000000, 0.9510565162951535312, 1.000000000000000000, 0.9510565162951535312, 1.000000000000000000, 0.9510565162951535312, 1.000000000000000000, 0.9510565162951535312, 1.000000000000000000, 0.9510565162951535312, 1.000000000000000000, 0.9510565162951535312, 1.000000000000000000, 0.9510565162951535312, 1.000000000000000000, 0.9510565162951535312, 1.000000000000000000, 0.9510565162951535312, 1.000000000000000000, 0.9510565162951535312, 1.000000000000000000, 0.9510565162951535312, 1.000000000000000000, 0.9510565162951535312, 1.000000000000000000, 0.9510565162951535312, 1.000000000000000000, 0.9510565162951535312, 1.000000000000000000, 0.9510565162951535312, 1.000000000000000000, 0.9510565162951535312, 1.000000000000000000, 0.9510565162951535312, 1.000000000000000000, 0.9510565162951535312, 1.000000000000000000, 0.9510565162951535312, 1.000000000000000000, 0.9510565162951535312, 1.000000000000000000, 0.9510565162951535312, 1.000000000000000000, 0.9510565162951535312, 1.000000000000000000, 0.9510565162951535312, 1.000000000000000000, 0.9510565162951535312, 1.000000000000000000, 0.9510565162951535312, 1.000000000000000000, 0.9510565162951535312, 1.000000000000000000, 0.9510565162951535312, 1.000000000000000000) ) ) 
 REPRESENTATION_ITEM ( '' )  SURFACE ( )  );
#25104 = CARTESIAN_POINT ( 'NONE',  ( 32.50000000000000711, 2.899999999999995470, 10.55989012756945122 ) ) ;
#25105 = ORIENTED_EDGE ( 'NONE', *, *, #32006, .T. ) ;
#25106 = CARTESIAN_POINT ( 'NONE',  ( 14.47279130897151767, 7.424999997268820096, -19.92008829642072598 ) ) ;
#25107 = CARTESIAN_POINT ( 'NONE',  ( 8.601468415847516980, 72.17500000273118133, -11.83890561707634781 ) ) ;
#25108 = CARTESIAN_POINT ( 'NONE',  ( 19.09188309203661049, 47.23437499999999289, -19.09188309203694445 ) ) ;
#25109 =( BOUNDED_CURVE ( )  B_SPLINE_CURVE ( 2, ( #29596, #11582, #8675, #22063, #604, #29269, #5772, #32010, #16252, #26708, #26871, #24137, #8505 ),
 .UNSPECIFIED., .F., .T. ) 
 B_SPLINE_CURVE_WITH_KNOTS ( ( 3, 2, 2, 2, 2, 2, 3 ),
 ( 0.1388888888888888673, 0.1444444444444444309, 0.1555555555555555580, 0.1666666666666666574, 0.1777777777777777846, 0.1888888888888888840, 0.1944444444444444475 ),
 .UNSPECIFIED. ) 
 CURVE ( )  GEOMETRIC_REPRESENTATION_ITEM ( )  RATIONAL_B_SPLINE_CURVE ( ( 0.9755282581475768211, 0.9755282581475768211, 1.000000000000000000, 0.9510565162951535312, 1.000000000000000000, 0.9510565162951535312, 1.000000000000000000, 0.9510565162951535312, 1.000000000000000000, 0.9510565162951535312, 1.000000000000000000, 0.9755282581475768211, 0.9755282581475768211 ) ) 
 REPRESENTATION_ITEM ( '' )  );
#25110 = CARTESIAN_POINT ( 'NONE',  ( -2.162160676586881955E-15, 60.62500000273117706, -35.31076352940723240 ) ) ;
#25111 = CARTESIAN_POINT ( 'NONE',  ( 10.37757302488624767, 21.97500000273118559, 31.93888565452638417 ) ) ;
#25112 = CARTESIAN_POINT ( 'NONE',  ( -33.58253175000000113, 9.375000002731184168, 0.000000000000000000 ) ) ;
#25113 = CARTESIAN_POINT ( 'NONE',  ( -33.58253175000000113, 5.275000002731187188, -10.91162601494193041 ) ) ;
#25114 = CARTESIAN_POINT ( 'NONE',  ( -20.53372385742071771, 12.57850666759064140, 20.47846945139902530 ) ) ;
#25115 = CARTESIAN_POINT ( 'NONE',  ( -15.01150461594642138, 60.26822916666665009, -26.00068869287340334 ) ) ;
#25116 = CARTESIAN_POINT ( 'NONE',  ( 5.779280353836490358E-15, 62.50000000000000000, 32.49999999999999289 ) ) ;
#25117 = CARTESIAN_POINT ( 'NONE',  ( -2.092463501923844636E-15, 49.50000000000001421, -34.17252228774368916 ) ) ;
#25118 = CARTESIAN_POINT ( 'NONE',  ( -20.75514604977248112, 53.42500000273117422, 28.56700777964554661 ) ) ;
#25119 = CARTESIAN_POINT ( 'NONE',  ( -14.47279130897152122, 1.924999997268818541, 19.92008829642072243 ) ) ;
#25120 = VERTEX_POINT ( 'NONE', #25998 ) ;
#25121 = CARTESIAN_POINT ( 'NONE',  ( -20.75514604977248823, 61.07500000273119412, -28.56700777964554305 ) ) ;
#25122 = CARTESIAN_POINT ( 'NONE',  ( 5.147494310547434893, 16.55125428154684641, 32.49999999999999289 ) ) ;
#25123 = CARTESIAN_POINT ( 'NONE',  ( 23.41746824999999887, 10.62499999726881938, 0.000000000000000000 ) ) ;
#25124 = CARTESIAN_POINT ( 'NONE',  ( 26.09010956794232428, 35.20871500092396644, -6.950374756619718042 ) ) ;
#25125 = ORIENTED_EDGE ( 'NONE', *, *, #18079, .T. ) ;
#25126 = CARTESIAN_POINT ( 'NONE',  ( 20.75514604977249178, 27.82500000273116925, 28.56700777964553950 ) ) ;
#25127 = CARTESIAN_POINT ( 'NONE',  ( -2.375766604868041476, 74.44874571845313938, 14.99999999999999822 ) ) ;
#25128 = ORIENTED_EDGE ( 'NONE', *, *, #1644, .T. ) ;
#25129 = CARTESIAN_POINT ( 'NONE',  ( 20.50609665441005092, 65.28125000000000000, 20.50609665440969209 ) ) ;
#25130 = CARTESIAN_POINT ( 'NONE',  ( 20.75514604977248467, 58.67500000273118843, -28.56700777964554305 ) ) ;
#25131 = CARTESIAN_POINT ( 'NONE',  ( -10.04305231718578462, 36.90000000546236691, 30.90933677959249337 ) ) ;
#25132 = CARTESIAN_POINT ( 'NONE',  ( -20.75514604977248823, 70.82500000273117280, -28.56700777964554305 ) ) ;
#25133 = CARTESIAN_POINT ( 'NONE',  ( -2.584737979205441561E-13, 33.05468750000000000, -30.02300923189239512 ) ) ;
#25134 = CARTESIAN_POINT ( 'NONE',  ( -7.570916362186215665, 13.39999999999999503, 23.30088464923126423 ) ) ;
#25135 = CARTESIAN_POINT ( 'NONE',  ( -10.37757302488624411, 2.975000002731182036, -31.93888565452638417 ) ) ;
#25136 = EDGE_CURVE ( 'NONE', #5936, #30261, #26227, .T. ) ;
#25137 = CARTESIAN_POINT ( 'NONE',  ( -33.58253175000000113, 11.12500000273120015, 0.000000000000000000 ) ) ;
#25138 = CARTESIAN_POINT ( 'NONE',  ( -8.601468415847515203, 73.17500000273119554, 11.83890561707634959 ) ) ;
#25139 = CARTESIAN_POINT ( 'NONE',  ( 30.02300923189239867, 49.66368083240936215, -0.04044903255044467877 ) ) ;
#25140 = CARTESIAN_POINT ( 'NONE',  ( 20.08610463437157279, 37.30000000000001137, -27.64615127144129758 ) ) ;
#25141 = CARTESIAN_POINT ( 'NONE',  ( -26.00068869287340334, 59.40885416666666430, 15.01150461594643559 ) ) ;
#25142 = CARTESIAN_POINT ( 'NONE',  ( 10.04305231718579705, 54.59999999999999432, 30.90933677959248982 ) ) ;
#25143 = CARTESIAN_POINT ( 'NONE',  ( 10.04305231718578817, 61.90000000546235981, -30.90933677959249337 ) ) ;
#25144 = CARTESIAN_POINT ( 'NONE',  ( -24.50000000000000000, 8.749999994537628112, -3.000384657911015469E-15 ) ) ;
#25145 = FACE_OUTER_BOUND ( 'NONE', #33753, .T. ) ;
#25146 = CARTESIAN_POINT ( 'NONE',  ( -13.97622843553588901, 17.87239583333332149, 24.20753774853756823 ) ) ;
#25147 = CARTESIAN_POINT ( 'NONE',  ( 33.58253175000000113, 40.22500000273119269, -10.91162601494193751 ) ) ;
#25148 = CARTESIAN_POINT ( 'NONE',  ( 11.25946833292375793, 76.07500000273120122, -8.180482586598735395 ) ) ;
#25149 = CARTESIAN_POINT ( 'NONE',  ( 27.16883889988624290, 40.17500000273120975, 19.73931689729373673 ) ) ;
#25150 = CARTESIAN_POINT ( 'NONE',  ( 27.16883889988624290, 26.17500000273118133, 19.73931689729373673 ) ) ;
#25151 = CARTESIAN_POINT ( 'NONE',  ( -1.778240108872766143E-15, 41.49999999999999289, -32.49999999999999289 ) ) ;
#25152 = CARTESIAN_POINT ( 'NONE',  ( -5.147494310547640062, 8.948745723915518369, 32.49999999999992895 ) ) ;
#25153 = CARTESIAN_POINT ( 'NONE',  ( 5.147494310547429563, 79.44874571845315359, -32.50000000000000000 ) ) ;
#25154 = CARTESIAN_POINT ( 'NONE',  ( 32.50000000000000000, 69.09999999999998010, -10.55989012756945833 ) ) ;
#25155 = CARTESIAN_POINT ( 'NONE',  ( 14.47279130897151944, 8.924999997268800556, -19.92008829642072598 ) ) ;
#25156 = CARTESIAN_POINT ( 'NONE',  ( 20.47846945139867003, 25.17149333240934439, -20.53372385742107653 ) ) ;
#25157 = CARTESIAN_POINT ( 'NONE',  ( 23.41746824999999887, 3.124999997268812280, 0.000000000000000000 ) ) ;
#25158 = CARTESIAN_POINT ( 'NONE',  ( 26.06988505166722803, 35.77045166574266943, -7.025853678916862854 ) ) ;
#25159 = CARTESIAN_POINT ( 'NONE',  ( 20.75514604977249178, 78.07500000273117280, 28.56700777964553950 ) ) ;
#25160 = CARTESIAN_POINT ( 'NONE',  ( -33.58253175000000113, 13.12500000273120193, 0.000000000000000000 ) ) ;
#25161 = CARTESIAN_POINT ( 'NONE',  ( -14.47279130897152122, 12.42499999726880766, 19.92008829642072243 ) ) ;
#25162 = CARTESIAN_POINT ( 'NONE',  ( -24.20753774853756823, 59.98177083333332149, -13.97622843553588723 ) ) ;
#25163 = ORIENTED_EDGE ( 'NONE', *, *, #21114, .F. ) ;
#25164 = CARTESIAN_POINT ( 'NONE',  ( 33.58253175000000113, 52.12500000273119838, -4.112674001490185761E-15 ) ) ;
#25165 = CARTESIAN_POINT ( 'NONE',  ( 27.16883889988624290, 20.17500000273118843, 19.73931689729373673 ) ) ;
#25166 = ORIENTED_EDGE ( 'NONE', *, *, #4965, .F. ) ;
#25167 = CARTESIAN_POINT ( 'NONE',  ( 20.50609665440969565, 36.92187499999999289, -20.50609665441004736 ) ) ;
#25168 = CARTESIAN_POINT ( 'NONE',  ( -7.468012846824771955, 34.34934000092397355, -28.02196122052045624 ) ) ;
#25169 = CARTESIAN_POINT ( 'NONE',  ( -7.570916362186210335, 8.349999994537615322, -23.30088464923126779 ) ) ;
#25170 = CARTESIAN_POINT ( 'NONE',  ( -24.50000000000000355, 16.64999999453763735, -7.960532557706207157 ) ) ;
#25171 = CARTESIAN_POINT ( 'NONE',  ( 7.236395654485755280, 12.22499999726881015, 22.27133577429736988 ) ) ;
#25172 = PRODUCT_DEFINITION_SHAPE ( 'NONE', 'NONE',  #33995 ) ;
#25173 = CARTESIAN_POINT ( 'NONE',  ( 33.58253175000000823, 20.27500000273117564, 10.91162601494192863 ) ) ;
#25174 = CARTESIAN_POINT ( 'NONE',  ( 10.04305231718579705, 23.10000000546236265, 30.90933677959248982 ) ) ;
#25175 = EDGE_CURVE ( 'NONE', #3077, #24457, #15713, .T. ) ;
#25176 = CARTESIAN_POINT ( 'NONE',  ( -20.08610463437156923, 70.30000000000001137, 27.64615127144130113 ) ) ;
#25177 = CARTESIAN_POINT ( 'NONE',  ( 20.08610463437157279, 47.80000000546238681, -27.64615127144129758 ) ) ;
#25178 = CARTESIAN_POINT ( 'NONE',  ( -7.755784534690364218, 74.00000000000002842, 12.20123439012139954 ) ) ;
#25179 = CARTESIAN_POINT ( 'NONE',  ( -15.04653450569291984, 57.12277750092398065, 25.98046417659859486 ) ) ;
#25180 = CARTESIAN_POINT ( 'NONE',  ( -10.37757302488624411, 38.97500000273118559, -31.93888565452638417 ) ) ;
#25181 = CARTESIAN_POINT ( 'NONE',  ( -8.601468415847518756, 81.07500000273120122, -11.83890561707634781 ) ) ;
#25182 = CARTESIAN_POINT ( 'NONE',  ( 28.01184896238290278, 26.89583333333332860, -7.505752307973347470 ) ) ;
#25183 = DIRECTION ( 'NONE',  ( 0.06081447046640141990, 0.000000000000000000, 0.9981490871517598729 ) ) ;
#25184 = EDGE_CURVE ( 'NONE', #33362, #26368, #8472, .T. ) ;
#25185 = CARTESIAN_POINT ( 'NONE',  ( -4.523095164977116484E-15, 12.62499999726879985, 24.62258325217400312 ) ) ;
#25186 = CARTESIAN_POINT ( 'NONE',  ( 10.04305231718579705, 12.59999999999999964, 30.90933677959248982 ) ) ;
#25187 = CARTESIAN_POINT ( 'NONE',  ( 7.570916362186207671, 15.60000000000000320, 23.30088464923126779 ) ) ;
#25188 = CARTESIAN_POINT ( 'NONE',  ( 6.950374756619257965, 45.51003499907601935, -26.09010956794244507 ) ) ;
#25189 = CARTESIAN_POINT ( 'NONE',  ( -10.37757302488624411, 58.72500000273117848, -31.93888565452638417 ) ) ;
#25190 = CARTESIAN_POINT ( 'NONE',  ( -2.162160676586882350E-15, 48.87500000273117706, -35.31076352940722529 ) ) ;
#25191 = FACE_OUTER_BOUND ( 'NONE', #174, .T. ) ;
#25192 = CARTESIAN_POINT ( 'NONE',  ( 5.485887633599118468E-07, 52.00000000000003553, -32.49999999999999289 ) ) ;
#25193 = CARTESIAN_POINT ( 'NONE',  ( 20.75514604977249178, 1.825000002731179460, 28.56700777964553950 ) ) ;
#25194 = CARTESIAN_POINT ( 'NONE',  ( 19.11951029504763611, 48.67225666759065206, -19.06425588902591173 ) ) ;
#25195 = CARTESIAN_POINT ( 'NONE',  ( 22.19496127021523435, 16.99999999999998579, 7.506443533373466259 ) ) ;
#25196 = CARTESIAN_POINT ( 'NONE',  ( -26.29305231718578995, 42.20000000000001705, 19.10302069950538595 ) ) ;
#25197 = CARTESIAN_POINT ( 'NONE',  ( 33.58253175000000113, 20.12500000273119483, -4.112674001490185761E-15 ) ) ;
#25198 = DIRECTION ( 'NONE',  ( -0.000000000000000000, -1.000000000000000000, -0.000000000000000000 ) ) ;
#25199 = CARTESIAN_POINT ( 'NONE',  ( -9.270509831248419985, 78.55000000546236549, 12.75976212528060039 ) ) ;
#25200 = CARTESIAN_POINT ( 'NONE',  ( 5.147494310547434893, 41.05125428700921475, 32.49999999999999289 ) ) ;
#25201 = CARTESIAN_POINT ( 'NONE',  ( 0.04044903255045854962, 60.83555583240935505, 30.02300923189239867 ) ) ;
#25202 = CARTESIAN_POINT ( 'NONE',  ( 6.277390505771533514E-15, 43.00000000546236123, 34.17252228774368916 ) ) ;
#25203 =( BOUNDED_CURVE ( )  B_SPLINE_CURVE ( 2, ( #20223, #30663, #7160, #17643, #25535, #27343, #29113, #18504, #18674, #28950, #1068, #26384, #21411 ),
 .UNSPECIFIED., .F., .T. ) 
 B_SPLINE_CURVE_WITH_KNOTS ( ( 3, 2, 2, 2, 2, 2, 3 ),
 ( 0.02777777777777777624, 0.03333333333333333287, 0.04444444444444444614, 0.05555555555555555247, 0.06666666666666667962, 0.07777777777777777901, 0.08333333333333334259 ),
 .UNSPECIFIED. ) 
 CURVE ( )  GEOMETRIC_REPRESENTATION_ITEM ( )  RATIONAL_B_SPLINE_CURVE ( ( 0.9755282581475768211, 0.9755282581475768211, 1.000000000000000000, 0.9510565162951535312, 1.000000000000000000, 0.9510565162951535312, 1.000000000000000000, 0.9510565162951535312, 1.000000000000000000, 0.9510565162951535312, 1.000000000000000000, 0.9755282581475767101, 0.9755282581475768211 ) ) 
 REPRESENTATION_ITEM ( '' )  );
#25204 = CARTESIAN_POINT ( 'NONE',  ( -32.50000000000000000, 60.50000000546237544, 0.000000000000000000 ) ) ;
#25205 = CARTESIAN_POINT ( 'NONE',  ( -2.162160676586882350E-15, 30.62500000273119838, -35.31076352940722529 ) ) ;
#25206 = CARTESIAN_POINT ( 'NONE',  ( 6.486482029760648627E-15, 65.87500000273119838, 35.31076352940722529 ) ) ;
#25207 = CARTESIAN_POINT ( 'NONE',  ( -6.988114217767819270, 31.47916666666666075, 26.07999730980490583 ) ) ;
#25208 = ORIENTED_EDGE ( 'NONE', *, *, #23447, .T. ) ;
#25209 = CARTESIAN_POINT ( 'NONE',  ( 6.486482029760649416E-15, 67.62500000273119838, 35.31076352940723240 ) ) ;
#25210 = CARTESIAN_POINT ( 'NONE',  ( -20.50609665441004736, 39.49999999999999289, -20.50609665440969565 ) ) ;
#25211 = CARTESIAN_POINT ( 'NONE',  ( -1.778240108872766143E-15, 69.49999999999998579, -32.49999999999999289 ) ) ;
#25212 = EDGE_LOOP ( 'NONE', ( #17664, #2042, #26132, #3643 ) ) ;
#25213 = CARTESIAN_POINT ( 'NONE',  ( 20.53372385742072481, 62.42225666759065206, -20.47846945139902175 ) ) ;
#25214 = CARTESIAN_POINT ( 'NONE',  ( -27.95245687107223986, 61.13319416759063785, -0.04044903254993292840 ) ) ;
#25215 = CARTESIAN_POINT ( 'NONE',  ( -27.16883889988624290, 12.92500000273118310, -19.73931689729374028 ) ) ;
#25216 =( GEOMETRIC_REPRESENTATION_CONTEXT ( 3 ) GLOBAL_UNCERTAINTY_ASSIGNED_CONTEXT ( ( #24034 ) ) GLOBAL_UNIT_ASSIGNED_CONTEXT ( ( #19868, #12136, #25013 ) ) REPRESENTATION_CONTEXT ( 'NONE', 'WORKASPACE' ) );
#25217 = CARTESIAN_POINT ( 'NONE',  ( 7.505752307972854531, 57.26041666666666430, -28.01184896238303423 ) ) ;
#25218 = LINE ( 'NONE', #2212, #6964 ) ;
#25219 = CARTESIAN_POINT ( 'NONE',  ( 10.37757302488624056, 38.77500000273118275, -31.93888565452638417 ) ) ;
#25220 = CARTESIAN_POINT ( 'NONE',  ( -26.29305231718579350, 42.30000000546238681, -19.10302069950537884 ) ) ;
#25221 = CARTESIAN_POINT ( 'NONE',  ( -11.25946833292375793, 73.57500000273120122, 8.180482586598737171 ) ) ;
#25222 = CARTESIAN_POINT ( 'NONE',  ( 33.58253175000000113, 32.12500000273119127, -4.112674001490185761E-15 ) ) ;
#25223 = CARTESIAN_POINT ( 'NONE',  ( -40.00000000000000711, 52.00000000000000711, -23.09401076758504345 ) ) ;
#25224 = CARTESIAN_POINT ( 'NONE',  ( -33.58253175000000113, 53.27500000273117564, -10.91162601494193218 ) ) ;
#25225 = PRESENTATION_STYLE_ASSIGNMENT (( #4630 ) ) ;
#25226 = EDGE_CURVE ( 'NONE', #13932, #15993, #29705, .T. ) ;
#25227 = CARTESIAN_POINT ( 'NONE',  ( 10.04305231718578817, 35.39999999999999858, -30.90933677959249337 ) ) ;
#25228 = ADVANCED_FACE ( 'NONE', ( #24273 ), #10644, .F. ) ;
#25229 = CARTESIAN_POINT ( 'NONE',  ( 6.277390505771533514E-15, 32.49999999999999289, 34.17252228774368916 ) ) ;
#25230 = CARTESIAN_POINT ( 'NONE',  ( -23.41746824999999887, 17.62499999726882649, -2.867812753649727150E-15 ) ) ;
#25231 = CARTESIAN_POINT ( 'NONE',  ( 10.37757302488624056, 78.52500000273118985, -31.93888565452638417 ) ) ;
#25232 = CARTESIAN_POINT ( 'NONE',  ( -26.29305231718579350, 70.30000000546237970, -19.10302069950537884 ) ) ;
#25233 = CARTESIAN_POINT ( 'NONE',  ( -32.50000000000000000, 38.00000000000000711, 0.000000000000000000 ) ) ;
#25234 = CARTESIAN_POINT ( 'NONE',  ( 27.16883889988624290, 68.17500000273119554, 19.73931689729373673 ) ) ;
#25235 = CARTESIAN_POINT ( 'NONE',  ( 15.00000000000000355, 75.15000000546237402, 4.873795443493592394 ) ) ;
#25236 = ORIENTED_EDGE ( 'NONE', *, *, #9886, .T. ) ;
#25237 = CARTESIAN_POINT ( 'NONE',  ( -33.58253175000000113, 15.22500000273119447, 10.91162601494193929 ) ) ;
#25238 = CARTESIAN_POINT ( 'NONE',  ( 15.14183272437242245, 8.049999994537621717, -20.84094480462497856 ) ) ;
#25239 = CARTESIAN_POINT ( 'NONE',  ( -13.94119854578936923, 20.45611083425730925, -24.22776226481241224 ) ) ;
#25240 = DIRECTION ( 'NONE',  ( -0.000000000000000000, -1.000000000000000000, -0.000000000000000000 ) ) ;
#25241 = CARTESIAN_POINT ( 'NONE',  ( -10.37757302488623701, 43.52500000273119696, 31.93888565452638417 ) ) ;
#25242 = CARTESIAN_POINT ( 'NONE',  ( 10.37757302488624767, 1.975000002731180926, 31.93888565452638417 ) ) ;
#25243 = CARTESIAN_POINT ( 'NONE',  ( -10.37757302488624411, 54.97500000273118559, -31.93888565452638417 ) ) ;
#25244 = CARTESIAN_POINT ( 'NONE',  ( 7.543491769121427382, 44.94829833425730925, -28.00173670424548433 ) ) ;
#25245 = CARTESIAN_POINT ( 'NONE',  ( 20.53372385742108008, 39.78086833240934794, 20.47846945139866648 ) ) ;
#25246 = CARTESIAN_POINT ( 'NONE',  ( -32.50000000000000000, 58.60000000546236976, 10.55989012756946366 ) ) ;
#25247 = CARTESIAN_POINT ( 'NONE',  ( 8.601468415847520532, 80.07500000273120122, 11.83890561707634781 ) ) ;
#25248 = CARTESIAN_POINT ( 'NONE',  ( 13.94119854578893580, 66.27826416574268364, -24.22776226481265383 ) ) ;
#25249 = DIRECTION ( 'NONE',  ( -0.000000000000000000, -1.000000000000000000, -0.000000000000000000 ) ) ;
#25250 = CARTESIAN_POINT ( 'NONE',  ( -32.50000000000000000, 74.60000000546234844, 10.55989012756946366 ) ) ;
#25251 = CARTESIAN_POINT ( 'NONE',  ( 20.50609665441005092, 13.71874999999999467, 20.50609665440969209 ) ) ;
#25252 = CARTESIAN_POINT ( 'NONE',  ( -2.162160676586881955E-15, 42.87500000273119127, -35.31076352940723240 ) ) ;
#25253 = CARTESIAN_POINT ( 'NONE',  ( 14.47279130897151767, 6.824999997268808904, 19.92008829642072953 ) ) ;
#25254 = ORIENTED_EDGE ( 'NONE', *, *, #2863, .F. ) ;
#25255 = CARTESIAN_POINT ( 'NONE',  ( 27.16883889988624290, 72.17500000273119554, 19.73931689729373673 ) ) ;
#25256 = CARTESIAN_POINT ( 'NONE',  ( -32.50000000000000000, 32.40000000546238113, -10.55989012756945478 ) ) ;
#25257 = EDGE_LOOP ( 'NONE', ( #27346, #3854, #27664, #4574 ) ) ;
#25258 = CARTESIAN_POINT ( 'NONE',  ( 26.00068869287340334, 30.19010416666665719, -15.01150461594642316 ) ) ;
#25259 = CARTESIAN_POINT ( 'NONE',  ( 26.29305231718578995, 65.70000000546238539, -19.10302069950538240 ) ) ;
#25260 = ORIENTED_EDGE ( 'NONE', *, *, #6275, .T. ) ;
#25261 = CARTESIAN_POINT ( 'NONE',  ( -24.50000000000000000, 12.64999999453762136, -7.960532557706207157 ) ) ;
#25262 = AXIS2_PLACEMENT_3D ( 'NONE', #23469, #23638, #10422 ) ;
#25263 = CARTESIAN_POINT ( 'NONE',  ( -10.37757302488623701, 47.52500000273118985, 31.93888565452638417 ) ) ;
#25264 = CARTESIAN_POINT ( 'NONE',  ( 23.41746825000000243, 16.72499999726881725, -7.608796670333727974 ) ) ;
#25265 = CARTESIAN_POINT ( 'NONE',  ( -30.02300923189239512, 63.13281250000000000, 2.654126918244515359E-13 ) ) ;
#25266 = CARTESIAN_POINT ( 'NONE',  ( -32.50000000000000000, 8.500000005462361230, 0.000000000000000000 ) ) ;
#25267 = CARTESIAN_POINT ( 'NONE',  ( -20.75514604977248823, 64.82500000273120122, -28.56700777964554305 ) ) ;
#25268 = CARTESIAN_POINT ( 'NONE',  ( 28.01184896238304134, 13.43229166666666607, 7.505752307972846538 ) ) ;
#25269 = CARTESIAN_POINT ( 'NONE',  ( -2.092463501923844636E-15, 55.49999999999999289, -34.17252228774368916 ) ) ;
#25270 = CARTESIAN_POINT ( 'NONE',  ( 7.570916362186213000, 2.400000000000013234, -23.30088464923126423 ) ) ;
#25271 = CARTESIAN_POINT ( 'NONE',  ( -10.37757302488623701, 17.77500000273118985, 31.93888565452638417 ) ) ;
#25272 = CARTESIAN_POINT ( 'NONE',  ( 24.50000000000000000, 0.000000000000000000, 0.000000000000000000 ) ) ;
#25273 = CARTESIAN_POINT ( 'NONE',  ( 27.95245687107223276, 22.16368083240936215, -0.04044903255042905932 ) ) ;
#25274 = CARTESIAN_POINT ( 'NONE',  ( 11.25946833292375793, 72.07500000273120122, -8.180482586598735395 ) ) ;
#25275 = CARTESIAN_POINT ( 'NONE',  ( 24.50000000000000000, 8.000000000000007105, 0.000000000000000000 ) ) ;
#25276 = CARTESIAN_POINT ( 'NONE',  ( -32.50000000000000000, 43.99999999999998579, 0.000000000000000000 ) ) ;
#25277 = CARTESIAN_POINT ( 'NONE',  ( -20.08610463437156923, 6.300000000000004263, 27.64615127144130113 ) ) ;
#25278 = ORIENTED_EDGE ( 'NONE', *, *, #32216, .T. ) ;
#25279 = CARTESIAN_POINT ( 'NONE',  ( -23.41746825000000598, 14.22499999726880660, 7.608796670333726198 ) ) ;
#25280 = CARTESIAN_POINT ( 'NONE',  ( -4.934616302121927505E-14, 71.00000000546238255, 32.50000000000000000 ) ) ;
#25281 = AXIS2_PLACEMENT_3D ( 'NONE', #27319, #3809, #14280 ) ;
#25282 = CARTESIAN_POINT ( 'NONE',  ( -26.07999730980490583, 49.52604166666666430, -6.988114217767815717 ) ) ;
#25283 = CARTESIAN_POINT ( 'NONE',  ( -33.58253175000000113, 63.12500000273117706, 0.000000000000000000 ) ) ;
#25284 = CARTESIAN_POINT ( 'NONE',  ( -2.162160676586881955E-15, 22.87500000273118062, -35.31076352940723240 ) ) ;
#25285 = CARTESIAN_POINT ( 'NONE',  ( -10.37757302488623701, 11.77500000273117031, 31.93888565452638417 ) ) ;
#25286 = CARTESIAN_POINT ( 'NONE',  ( -20.75514604977248823, 3.075000002731198112, -28.56700777964554305 ) ) ;
#25287 = CARTESIAN_POINT ( 'NONE',  ( -30.02300923189239867, 16.44569416759064140, -0.04044903254991731589 ) ) ;
#25288 = CARTESIAN_POINT ( 'NONE',  ( 7.505752307973351023, 58.69270833333332860, 28.01184896238290278 ) ) ;
#25289 = CARTESIAN_POINT ( 'NONE',  ( -2.162160676586881955E-15, 2.625000002731183724, -35.31076352940723240 ) ) ;
#25290 = CARTESIAN_POINT ( 'NONE',  ( 26.29305231718579350, 68.79999999999999716, 19.10302069950537529 ) ) ;
#25291 = CARTESIAN_POINT ( 'NONE',  ( -32.50000000000000000, 43.90000000000001279, -10.55989012756945478 ) ) ;
#25292 = AXIS2_PLACEMENT_3D ( 'NONE', #26386, #284, #10772 ) ;
#25293 = AXIS2_PLACEMENT_3D ( 'NONE', #24180, #6141, #18868 ) ;
#25294 = CARTESIAN_POINT ( 'NONE',  ( -27.16883889988624290, 42.92500000273119554, -19.73931689729374028 ) ) ;
#25295 = CARTESIAN_POINT ( 'NONE',  ( 23.41746824999999887, 0.6249999972688102812, 0.000000000000000000 ) ) ;
#25296 = EDGE_CURVE ( 'NONE', #2254, #20157, #25976, .T. ) ;
#25297 = CARTESIAN_POINT ( 'NONE',  ( -26.07999730980477437, 66.42708333333332860, 6.988114217768305103 ) ) ;
#25298 = ORIENTED_EDGE ( 'NONE', *, *, #8324, .T. ) ;
#25299 = CARTESIAN_POINT ( 'NONE',  ( 33.58253175000000823, 60.27500000273116143, 10.91162601494192863 ) ) ;
#25300 = CARTESIAN_POINT ( 'NONE',  ( 32.50000000000000711, 16.89999999999998792, 10.55989012756945122 ) ) ;
#25301 = CARTESIAN_POINT ( 'NONE',  ( 7.236395654485755280, 12.22499999726881015, 22.27133577429736988 ) ) ;
#25302 = CARTESIAN_POINT ( 'NONE',  ( -24.18731323226248264, 30.48215250092397710, -14.01125832528284931 ) ) ;
#25303 = VERTEX_POINT ( 'NONE', #30068 ) ;
#25304 = CARTESIAN_POINT ( 'NONE',  ( -10.37757302488624411, 28.72500000273118914, -31.93888565452638417 ) ) ;
#25305 = DIRECTION ( 'NONE',  ( -0.000000000000000000, -1.000000000000000000, -0.000000000000000000 ) ) ;
#25306 = ORIENTED_EDGE ( 'NONE', *, *, #21821, .T. ) ;
#25307 = CARTESIAN_POINT ( 'NONE',  ( -5.147494310547423346, 36.94874572391552903, 32.50000000000000000 ) ) ;
#25308 = CARTESIAN_POINT ( 'NONE',  ( 27.16883889988623935, 66.32500000273117280, -19.73931689729374384 ) ) ;
#25309 = CARTESIAN_POINT ( 'NONE',  ( -20.50609665441004736, 36.06250000000000000, -20.50609665440969565 ) ) ;
#25310 = CARTESIAN_POINT ( 'NONE',  ( 24.50000000000000000, 10.00000000000000888, 0.000000000000000000 ) ) ;
#25311 = CARTESIAN_POINT ( 'NONE',  ( 20.75514604977249178, 2.075000002731171467, 28.56700777964553950 ) ) ;
#25312 = CARTESIAN_POINT ( 'NONE',  ( 10.37757302488624767, 7.725000002731185589, 31.93888565452638417 ) ) ;
#25313 = CARTESIAN_POINT ( 'NONE',  ( 20.08610463437157279, 29.30000000000000782, -27.64615127144129758 ) ) ;
#25314 = CARTESIAN_POINT ( 'NONE',  ( 7.468012846824281681, 55.82253499907601935, -28.02196122052058058 ) ) ;
#25315 = CARTESIAN_POINT ( 'NONE',  ( 15.00000000000000355, 72.90000000000000568, 4.873795443493592394 ) ) ;
#25316 = CARTESIAN_POINT ( 'NONE',  ( 26.00068869287367690, 58.26302083333332860, 15.01150461594596486 ) ) ;
#25317 = CARTESIAN_POINT ( 'NONE',  ( 5.779280353836490358E-15, 54.49999999999999289, 32.49999999999999289 ) ) ;
#25318 = CARTESIAN_POINT ( 'NONE',  ( -26.29305231718578995, 52.20000000000000995, 19.10302069950538595 ) ) ;
#25319 = CARTESIAN_POINT ( 'NONE',  ( 24.50000000000000355, 3.849999994537637082, -7.960532557706203605 ) ) ;
#25320 = CARTESIAN_POINT ( 'NONE',  ( 15.00000000000000355, 77.15000000546240244, 4.873795443493592394 ) ) ;
#25321 = CARTESIAN_POINT ( 'NONE',  ( -27.95245687107222921, 25.32031250000000000, 2.498001805406602216E-13 ) ) ;
#25322 = CARTESIAN_POINT ( 'NONE',  ( -10.37757302488623701, 37.52500000273117564, 31.93888565452638417 ) ) ;
#25323 = CARTESIAN_POINT ( 'NONE',  ( 8.601468415847520532, 71.57500000273118701, 11.83890561707634781 ) ) ;
#25324 = CARTESIAN_POINT ( 'NONE',  ( -10.37757302488623701, 45.77500000273119696, 31.93888565452638417 ) ) ;
#25325 = CARTESIAN_POINT ( 'NONE',  ( -33.58253175000000113, 23.27500000273116854, -10.91162601494193041 ) ) ;
#25326 = CARTESIAN_POINT ( 'NONE',  ( -32.50000000000000000, 18.00000000000001421, 0.000000000000000000 ) ) ;
#25327 = CARTESIAN_POINT ( 'NONE',  ( -20.08610463437156923, 58.29999999999999716, 27.64615127144130113 ) ) ;
#25328 = VECTOR ( 'NONE', #29792, 1000.000000000000000 ) ;
#25329 = CARTESIAN_POINT ( 'NONE',  ( -14.47279130897152299, 11.92499999726882187, 19.92008829642072243 ) ) ;
#25330 = CARTESIAN_POINT ( 'NONE',  ( 14.97647472619900455, 28.46576416574268720, -26.02091320914876960 ) ) ;
#25331 = CARTESIAN_POINT ( 'NONE',  ( 14.47279130897151767, 1.424999997268804997, -19.92008829642072598 ) ) ;
#25332 = CARTESIAN_POINT ( 'NONE',  ( 14.01125832528330051, 39.92409749907602645, 24.18731323226221974 ) ) ;
#25333 = CARTESIAN_POINT ( 'NONE',  ( -10.37757302488624411, 78.97500000273120691, -31.93888565452638417 ) ) ;
#25334 = CARTESIAN_POINT ( 'NONE',  ( 33.58253175000000113, 16.12500000273120548, -4.112674001490185761E-15 ) ) ;
#25335 = CARTESIAN_POINT ( 'NONE',  ( 14.47279130897151767, 11.42499999726880944, -19.92008829642072598 ) ) ;
#25336 = CARTESIAN_POINT ( 'NONE',  ( 6.988114217767829928, 60.69791666666667140, -26.07999730980489872 ) ) ;
#25337 = CIRCLE ( 'NONE', #20354, 31.91025403784435710 ) ;
#25338 = ORIENTED_EDGE ( 'NONE', *, *, #27400, .F. ) ;
#25339 = CARTESIAN_POINT ( 'NONE',  ( 10.37757302488624056, 50.52500000273117564, -31.93888565452638417 ) ) ;
#25340 = CARTESIAN_POINT ( 'NONE',  ( -27.16883889988623935, 21.57500000273120122, 19.73931689729374739 ) ) ;
#25341 = EDGE_LOOP ( 'NONE', ( #27662, #14457, #31546, #10875 ) ) ;
#25342 = CARTESIAN_POINT ( 'NONE',  ( -2.584737979205441561E-13, 29.61718749999999645, -30.02300923189239512 ) ) ;
#25343 = CARTESIAN_POINT ( 'NONE',  ( 20.53372385742072481, 31.48475666759063074, -20.47846945139902175 ) ) ;
#25344 = CARTESIAN_POINT ( 'NONE',  ( 14.47279130897151767, 1.424999997268804997, -19.92008829642072598 ) ) ;
#25345 = CARTESIAN_POINT ( 'NONE',  ( -18.94512977948576093, 13.82499999726882756, 13.76444248337722698 ) ) ;
#25346 = CARTESIAN_POINT ( 'NONE',  ( -33.58253175000000113, 21.37500000273118062, 0.000000000000000000 ) ) ;
#25347 = CARTESIAN_POINT ( 'NONE',  ( -26.29305231718579350, 22.30000000546239391, -19.10302069950537884 ) ) ;
#25348 = VECTOR ( 'NONE', #4518, 1000.000000000000000 ) ;
#25349 = CARTESIAN_POINT ( 'NONE',  ( -26.29305231718579350, 65.79999999999999716, -19.10302069950537884 ) ) ;
#25350 = CARTESIAN_POINT ( 'NONE',  ( -12.11000150615021198, -45.00000000000000000, 0.000000000000000000 ) ) ;
#25351 = CARTESIAN_POINT ( 'NONE',  ( 5.348221797398307942, 74.00000000000001421, 12.84883053416113974 ) ) ;
#25352 = CARTESIAN_POINT ( 'NONE',  ( 26.00068869287340334, 13.00260416666666430, -15.01150461594642316 ) ) ;
#25353 = CARTESIAN_POINT ( 'NONE',  ( -27.16883889988623935, 37.57500000273117280, 19.73931689729374739 ) ) ;
#25354 = CARTESIAN_POINT ( 'NONE',  ( 10.04305231718578817, 43.90000000546237402, -30.90933677959249337 ) ) ;
#25355 = CARTESIAN_POINT ( 'NONE',  ( -30.02300923189239867, 32.19531250000000000, 2.654126918244514854E-13 ) ) ;
#25356 = PRODUCT_CONTEXT ( 'NONE', #12045, 'mechanical' ) ;
#25357 = CIRCLE ( 'NONE', #23158, 16.50000000000002842 ) ;
#25358 = CARTESIAN_POINT ( 'NONE',  ( -7.236395654485763274, 14.52499999726880553, 22.27133577429736633 ) ) ;
#25359 = CARTESIAN_POINT ( 'NONE',  ( 26.29305231718578995, 11.19999999999998863, -19.10302069950538240 ) ) ;
#25360 = CARTESIAN_POINT ( 'NONE',  ( 24.50000000000000000, 17.99999999999998934, 0.000000000000000000 ) ) ;
#25361 = CARTESIAN_POINT ( 'NONE',  ( -24.22776226481266448, 55.10638916574269786, -13.94119854578892514 ) ) ;
#25362 = CARTESIAN_POINT ( 'NONE',  ( -2.162160676586881955E-15, 54.62500000273116996, -35.31076352940723240 ) ) ;
#25363 = CARTESIAN_POINT ( 'NONE',  ( -33.58253175000000113, 59.27500000273119696, -10.91162601494193218 ) ) ;
#25364 = CARTESIAN_POINT ( 'NONE',  ( -33.58253175000000113, 41.27500000273118275, -10.91162601494193041 ) ) ;
#25365 = LINE ( 'NONE', #30498, #27694 ) ;
#25366 = CARTESIAN_POINT ( 'NONE',  ( 3.880418787951178228, 10.44874571845314293, -24.49999999999998224 ) ) ;
#25367 = CARTESIAN_POINT ( 'NONE',  ( -26.50000000000000000, -23.00000000000000355, 0.000000000000000000 ) ) ;
#25368 = CARTESIAN_POINT ( 'NONE',  ( 27.95245687107223986, 52.53944416759064495, 0.04044903254993640479 ) ) ;
#25369 = CARTESIAN_POINT ( 'NONE',  ( -24.32582046900600758, 17.00000000000000000, -2.464910051867566843 ) ) ;
#25370 = CARTESIAN_POINT ( 'NONE',  ( -20.08610463437156923, 42.30000000000000426, 27.64615127144130113 ) ) ;
#25371 = CARTESIAN_POINT ( 'NONE',  ( 10.37757302488624767, 21.72500000273118559, 31.93888565452638417 ) ) ;
#25372 = CARTESIAN_POINT ( 'NONE',  ( -4.405589869732278832E-13, 31.00000000546236834, 32.50000000000000000 ) ) ;
#25373 = CARTESIAN_POINT ( 'NONE',  ( -1.778240108872766143E-15, 53.50000000000000000, -32.49999999999999289 ) ) ;
#25374 = FACE_OUTER_BOUND ( 'NONE', #24256, .T. ) ;
#25375 = CARTESIAN_POINT ( 'NONE',  ( 7.543491769121922985, 67.56732666574268364, 28.00173670424535644 ) ) ;
#25376 = CARTESIAN_POINT ( 'NONE',  ( 20.08610463437158344, 39.20000000546237118, 27.64615127144129403 ) ) ;
#25377 = EDGE_CURVE ( 'NONE', #4064, #11228, #29799, .T. ) ;
#25378 = CARTESIAN_POINT ( 'NONE',  ( 5.147494310547434893, 34.55125428154683220, 32.49999999999999289 ) ) ;
#25380 = CARTESIAN_POINT ( 'NONE',  ( 27.16883889988623935, 32.32500000273119412, -19.73931689729374384 ) ) ;
#25379 = CIRCLE ( 'NONE', #13335, 24.50000000000000000 ) ;
#25381 = CARTESIAN_POINT ( 'NONE',  ( -24.20753774853730889, 38.78385416666665719, 13.97622843553633842 ) ) ;
#25382 = EDGE_CURVE ( 'NONE', #19851, #31882, #3859, .T. ) ;
#25383 = ORIENTED_EDGE ( 'NONE', *, *, #22154, .T. ) ;
#25384 = AXIS2_PLACEMENT_3D ( 'NONE', #3172, #8302, #3333 ) ;
#25385 = CARTESIAN_POINT ( 'NONE',  ( -33.58253175000000113, 67.22500000273117848, 10.91162601494193929 ) ) ;
#25386 = CARTESIAN_POINT ( 'NONE',  ( -15.01150461594595775, 38.49739583333332860, 26.00068869287368756 ) ) ;
#25387 = CARTESIAN_POINT ( 'NONE',  ( -26.29305231718579350, 16.30000000546239036, -19.10302069950537884 ) ) ;
#25388 = ORIENTED_EDGE ( 'NONE', *, *, #31175, .F. ) ;
#25389 = CARTESIAN_POINT ( 'NONE',  ( -28.00173670424549499, 61.27642333425730925, -7.543491769121417612 ) ) ;
#25390 = CARTESIAN_POINT ( 'NONE',  ( 19.06425588902592239, 56.40663166759065206, 19.11951029504763611 ) ) ;
#25391 = CARTESIAN_POINT ( 'NONE',  ( -33.58253175000000113, 11.22500000273118559, 10.91162601494193929 ) ) ;
#25392 = CARTESIAN_POINT ( 'NONE',  ( 30.02300923189239867, 15.28868083240935505, -0.04044903255044467877 ) ) ;
#25393 = CARTESIAN_POINT ( 'NONE',  ( 9.270509831248425314, 78.95000000546235697, 12.75976212528059683 ) ) ;
#25394 = CARTESIAN_POINT ( 'NONE',  ( -33.58253175000000113, 43.37500000273119838, 0.000000000000000000 ) ) ;
#25395 = CARTESIAN_POINT ( 'NONE',  ( 10.04305231718579705, 45.10000000546238397, 30.90933677959248982 ) ) ;
#25396 = CARTESIAN_POINT ( 'NONE',  ( 15.00000000000000000, 79.10000000000000853, -4.873795443493596835 ) ) ;
#25397 = CARTESIAN_POINT ( 'NONE',  ( 27.16883889988624290, 29.92500000273118488, 19.73931689729373673 ) ) ;
#25398 = CARTESIAN_POINT ( 'NONE',  ( 5.779280353836490358E-15, 65.00000000546236834, 32.49999999999999289 ) ) ;
#25399 = CARTESIAN_POINT ( 'NONE',  ( -27.16883889988623935, 55.57500000273118701, 19.73931689729374739 ) ) ;
#25400 = CARTESIAN_POINT ( 'NONE',  ( -32.50000000000000000, 28.00000000000001066, 0.000000000000000000 ) ) ;
#25401 = CARTESIAN_POINT ( 'NONE',  ( 10.04305231718579705, 32.59999999999998721, 30.90933677959248982 ) ) ;
#25402 = CARTESIAN_POINT ( 'NONE',  ( -4.523095164977116484E-15, 18.12499999726882649, 24.62258325217400312 ) ) ;
#25403 = CARTESIAN_POINT ( 'NONE',  ( 33.58253175000000823, 76.02500000273118985, 10.91162601494192863 ) ) ;
#25404 = CARTESIAN_POINT ( 'NONE',  ( 0.000000000000000000, -20.99999999999998934, 0.000000000000000000 ) ) ;
#25405 = CYLINDRICAL_SURFACE ( 'NONE', #19365, 30.00000000000000000 ) ;
#25406 = CARTESIAN_POINT ( 'NONE',  ( 33.58253175000000113, 68.47500000273119269, -10.91162601494193574 ) ) ;
#25407 = CARTESIAN_POINT ( 'NONE',  ( -9.657523855033125146E-16, 75.75000000546241097, -15.77193336357400710 ) ) ;
#25408 = VECTOR ( 'NONE', #19221, 1000.000000000000114 ) ;
#25409 = EDGE_LOOP ( 'NONE', ( #8370, #28590, #23965, #8372 ) ) ;
#25410 = CARTESIAN_POINT ( 'NONE',  ( 10.37757302488624056, 20.52500000273119340, -31.93888565452638417 ) ) ;
#25411 = CARTESIAN_POINT ( 'NONE',  ( 7.570916362186207671, 11.34999999453761887, 23.30088464923126779 ) ) ;
#25412 = CARTESIAN_POINT ( 'NONE',  ( -24.22776226481240514, 23.03423583425731280, 13.94119854578937812 ) ) ;
#25413 =( BOUNDED_CURVE ( )  B_SPLINE_CURVE ( 2, ( #17964, #9881, #33909, #20878, #33384, #10235, #31497, #4728, #20716, #31326, #20539, #7301, #15731 ),
 .UNSPECIFIED., .F., .T. ) 
 B_SPLINE_CURVE_WITH_KNOTS ( ( 3, 2, 2, 2, 2, 2, 3 ),
 ( 0.1730769230769230727, 0.1743589743589743501, 0.1769230769230769329, 0.1794871794871794879, 0.1820512820512820429, 0.1846153846153846256, 0.1858974358974359031 ),
 .UNSPECIFIED. ) 
 CURVE ( )  GEOMETRIC_REPRESENTATION_ITEM ( )  RATIONAL_B_SPLINE_CURVE ( ( 0.9755282581475768211, 0.9755282581475768211, 1.000000000000000000, 0.9510565162951535312, 1.000000000000000000, 0.9510565162951535312, 1.000000000000000000, 0.9510565162951535312, 1.000000000000000000, 0.9510565162951535312, 1.000000000000000000, 0.9755282581475768211, 0.9755282581475768211 ) ) 
 REPRESENTATION_ITEM ( '' )  );
#25414 = CARTESIAN_POINT ( 'NONE',  ( -15.00000000000000000, 74.35000000546239107, 4.873795443493597723 ) ) ;
#25415 = CARTESIAN_POINT ( 'NONE',  ( 33.58253175000000823, 44.02500000273118275, 10.91162601494192863 ) ) ;
#25416 = CARTESIAN_POINT ( 'NONE',  ( 33.58253175000000823, 6.275000002731184523, 10.91162601494192863 ) ) ;
#25417 = CARTESIAN_POINT ( 'NONE',  ( 10.37757302488624767, 55.97500000273118559, 31.93888565452638417 ) ) ;
#25418 = CARTESIAN_POINT ( 'NONE',  ( 30.02300923189239867, 49.10194416759064495, 0.04044903254992252006 ) ) ;
#25419 = CARTESIAN_POINT ( 'NONE',  ( -1.137977401836464321E-14, 66.99999999999998579, 46.18802153517007270 ) ) ;
#25420 = CARTESIAN_POINT ( 'NONE',  ( -15.04653450569338524, 34.76784749907601935, -25.98046417659831775 ) ) ;
#25421 = CARTESIAN_POINT ( 'NONE',  ( 26.29305231718578995, 61.70000000546237118, -19.10302069950538240 ) ) ;
#25422 = EDGE_CURVE ( 'NONE', #23066, #9545, #23241, .T. ) ;
#25423 = CARTESIAN_POINT ( 'NONE',  ( 8.601468415847516980, 72.17500000273116711, -11.83890561707634781 ) ) ;
#25424 = CARTESIAN_POINT ( 'NONE',  ( -14.01125832528328985, 62.26784749907602645, -24.18731323226223040 ) ) ;
#25425 = CARTESIAN_POINT ( 'NONE',  ( -5.147494310547430452, 53.55125428154684641, -32.49999999999999289 ) ) ;
#25426 = CARTESIAN_POINT ( 'NONE',  ( -2.092463501923844636E-15, 78.00000000546238255, -34.17252228774368916 ) ) ;
#25427 = CARTESIAN_POINT ( 'NONE',  ( -15.01150461594642138, 15.58072916666666607, -26.00068869287340334 ) ) ;
#25428 = CARTESIAN_POINT ( 'NONE',  ( -20.75514604977248823, 37.07500000273120122, -28.56700777964554305 ) ) ;
#25429 = CARTESIAN_POINT ( 'NONE',  ( 7.236395654485760609, 7.524999997268827734, -22.27133577429736633 ) ) ;
#25430 = ORIENTED_EDGE ( 'NONE', *, *, #32216, .F. ) ;
#25431 = CARTESIAN_POINT ( 'NONE',  ( -27.16883889988624290, 73.17500000273119554, -19.73931689729374028 ) ) ;
#25432 = AXIS2_PLACEMENT_3D ( 'NONE', #23355, #2586, #23522 ) ;
#25433 = CARTESIAN_POINT ( 'NONE',  ( -26.29305231718578995, 26.70000000546236762, 19.10302069950538595 ) ) ;
#25434 = CIRCLE ( 'NONE', #12269, 30.00000000000004974 ) ;
#25435 = CARTESIAN_POINT ( 'NONE',  ( -15.01150461594595775, 41.93489583333333570, 26.00068869287368756 ) ) ;
#25436 = CARTESIAN_POINT ( 'NONE',  ( 32.50000000000000000, 63.60000000546238397, -10.55989012756945833 ) ) ;
#25437 = ORIENTED_EDGE ( 'NONE', *, *, #21950, .F. ) ;
#25438 = CARTESIAN_POINT ( 'NONE',  ( 10.04305231718578817, 27.40000000000000924, -30.90933677959249337 ) ) ;
#25439 = CARTESIAN_POINT ( 'NONE',  ( 10.37757302488624767, 47.72500000273119269, 31.93888565452638417 ) ) ;
#25440 = CARTESIAN_POINT ( 'NONE',  ( -4.523095164977116484E-15, 16.12499999726880873, 24.62258325217400312 ) ) ;
#25441 = APPLICATION_CONTEXT ( 'automotive_design' ) ;
#25442 = CARTESIAN_POINT ( 'NONE',  ( 26.29305231718579350, 7.300000005462381480, 19.10302069950537529 ) ) ;
#25443 = CARTESIAN_POINT ( 'NONE',  ( -4.635254915624211769, 77.60000000000000853, -14.26584774442730286 ) ) ;
#25444 = CARTESIAN_POINT ( 'NONE',  ( -15.01150461594642316, 15.58072916666666430, -26.00068869287341045 ) ) ;
#25445 = CARTESIAN_POINT ( 'NONE',  ( -26.29305231718578995, 50.19999999999999574, 19.10302069950538595 ) ) ;
#25446 = CARTESIAN_POINT ( 'NONE',  ( 7.236395654485760609, 1.024999997268821739, -22.27133577429736633 ) ) ;
#25447 = CARTESIAN_POINT ( 'NONE',  ( 20.75514604977249178, 16.07500000273119412, 28.56700777964553950 ) ) ;
#25448 = CARTESIAN_POINT ( 'NONE',  ( -20.08610463437156923, 74.30000000000001137, 27.64615127144130113 ) ) ;
#25449 = CARTESIAN_POINT ( 'NONE',  ( 26.06988505166722803, 25.45795166574268364, -7.025853678916862854 ) ) ;
#25450 = CARTESIAN_POINT ( 'NONE',  ( 13.91746825000000065, 78.27500000273116143, 4.522059556121114987 ) ) ;
#25451 = CARTESIAN_POINT ( 'NONE',  ( 19.82091636218621034, 7.800000000000001599, 14.40073868116559730 ) ) ;
#25452 = CARTESIAN_POINT ( 'NONE',  ( 20.52662985655321393, 52.00000000000000000, 26.66963712870524716 ) ) ;
#25453 = CARTESIAN_POINT ( 'NONE',  ( 20.08610463437157279, 5.300000000000006928, -27.64615127144129758 ) ) ;
#25454 = ORIENTED_EDGE ( 'NONE', *, *, #4609, .F. ) ;
#25455 = CARTESIAN_POINT ( 'NONE',  ( -23.41746825000000243, 12.02499999726881974, -7.608796670333730638 ) ) ;
#25456 = CARTESIAN_POINT ( 'NONE',  ( 18.94512977948576093, 0.8249999972688160099, -13.76444248337722875 ) ) ;
#25457 = PRESENTATION_LAYER_ASSIGNMENT (  '', '', ( #31478 ) ) ;
#25458 = CARTESIAN_POINT ( 'NONE',  ( 26.07999730980477437, 50.95833333333332860, -6.988114217768290004 ) ) ;
#25459 = CARTESIAN_POINT ( 'NONE',  ( -10.37757302488623701, 57.52500000273118275, 31.93888565452638417 ) ) ;
#25460 = CARTESIAN_POINT ( 'NONE',  ( 20.75514604977249178, 24.07500000273120122, 28.56700777964553950 ) ) ;
#25461 = CARTESIAN_POINT ( 'NONE',  ( -10.37757302488624411, 12.97500000273120513, -31.93888565452638417 ) ) ;
#25462 = CARTESIAN_POINT ( 'NONE',  ( -26.07999730980477437, 28.61458333333333215, 6.988114217768305103 ) ) ;
#25463 = CARTESIAN_POINT ( 'NONE',  ( -10.37757302488623701, 5.775000002731179194, 31.93888565452638417 ) ) ;
#25464 = CARTESIAN_POINT ( 'NONE',  ( -28.02196122052045268, 19.73996500092397355, 7.468012846824790607 ) ) ;
#25465 = CARTESIAN_POINT ( 'NONE',  ( -2.584737979205441561E-13, 63.99218749999997868, -30.02300923189239512 ) ) ;
#25466 = CARTESIAN_POINT ( 'NONE',  ( -33.58253175000000113, 1.225000002731198467, 10.91162601494193929 ) ) ;
#25467 = CARTESIAN_POINT ( 'NONE',  ( 10.04305231718578817, 69.40000000000001990, -30.90933677959249337 ) ) ;
#25468 = CARTESIAN_POINT ( 'NONE',  ( 20.08610463437157279, 41.30000000000001137, -27.64615127144129758 ) ) ;
#25469 = CARTESIAN_POINT ( 'NONE',  ( 20.75514604977249178, 47.82500000273117990, 28.56700777964553950 ) ) ;
#25470 = CARTESIAN_POINT ( 'NONE',  ( 14.47279130897151767, 2.924999997268815655, -19.92008829642072598 ) ) ;
#25471 = DIRECTION ( 'NONE',  ( 0.000000000000000000, -0.000000000000000000, -1.000000000000000000 ) ) ;
#25472 = ORIENTED_EDGE ( 'NONE', *, *, #29829, .T. ) ;
#25473 = CARTESIAN_POINT ( 'NONE',  ( 10.37757302488624056, 58.77500000273121117, -31.93888565452638417 ) ) ;
#25474 = CARTESIAN_POINT ( 'NONE',  ( 5.779280353836490358E-15, 5.000000005462372776, 32.49999999999999289 ) ) ;
#25475 = CARTESIAN_POINT ( 'NONE',  ( 18.94512977948575738, 14.42499999726881654, 13.76444248337723408 ) ) ;
#25476 = CARTESIAN_POINT ( 'NONE',  ( 14.01125832528286352, 31.34152750092398421, -24.18731323226246843 ) ) ;
#25477 = CARTESIAN_POINT ( 'NONE',  ( -27.16883889988623935, 77.57500000273121543, 19.73931689729374739 ) ) ;
#25478 = VERTEX_POINT ( 'NONE', #11716 ) ;
#25479 = CARTESIAN_POINT ( 'NONE',  ( 6.486482029760649416E-15, 29.62500000273120193, 35.31076352940723240 ) ) ;
#25480 = CARTESIAN_POINT ( 'NONE',  ( -5.147494310547423346, 34.94874572391554324, 32.50000000000000000 ) ) ;
#25481 = PRESENTATION_LAYER_ASSIGNMENT (  '', '', ( #18367 ) ) ;
#25482 = EDGE_LOOP ( 'NONE', ( #33312, #15787, #10880, #4402 ) ) ;
#25483 = CARTESIAN_POINT ( 'NONE',  ( -4.635254915624208216, 76.40000000000001990, 14.26584774442730463 ) ) ;
#25484 = CARTESIAN_POINT ( 'NONE',  ( 27.16883889988624290, 65.92500000273118133, 19.73931689729373673 ) ) ;
#25485 = CARTESIAN_POINT ( 'NONE',  ( -15.01150461594642138, 39.64322916666667140, -26.00068869287340334 ) ) ;
#25486 = CARTESIAN_POINT ( 'NONE',  ( -19.82091636218621034, 12.80000000000000604, -14.40073868116559552 ) ) ;
#25487 = CARTESIAN_POINT ( 'NONE',  ( 7.236395654485755280, 4.724999997268803043, 22.27133577429736988 ) ) ;
#25488 = CARTESIAN_POINT ( 'NONE',  ( -33.58253175000000113, 7.025000002731188964, -10.91162601494193218 ) ) ;
#25489 = SURFACE_SIDE_STYLE ('',( #20860 ) ) ;
#25490 = CARTESIAN_POINT ( 'NONE',  ( -20.53372385742107653, 51.81211833240936215, -20.47846945139867003 ) ) ;
#25491 = CARTESIAN_POINT ( 'NONE',  ( 12.13525491562421088, 72.79999999999999716, 8.816778784387095058 ) ) ;
#25492 = CARTESIAN_POINT ( 'NONE',  ( 7.505752307973351023, 65.56770833333332860, 28.01184896238290278 ) ) ;
#25493 = PLANE ( 'NONE',  #31049 ) ;
#25494 = CARTESIAN_POINT ( 'NONE',  ( 7.570916362186207671, 13.34999999453762065, 23.30088464923126779 ) ) ;
#25495 = CARTESIAN_POINT ( 'NONE',  ( 12.13525491562421088, 75.05000000546237970, 8.816778784387095058 ) ) ;
#25496 = CARTESIAN_POINT ( 'NONE',  ( -6.988114217767819270, 24.60416666666666430, 26.07999730980490583 ) ) ;
#25497 = CARTESIAN_POINT ( 'NONE',  ( 10.37757302488624056, 30.52500000273117209, -31.93888565452638417 ) ) ;
#25498 = CARTESIAN_POINT ( 'NONE',  ( -33.58253175000000113, 79.02500000273118985, -10.91162601494193218 ) ) ;
#25499 = CARTESIAN_POINT ( 'NONE',  ( -10.37757302488624411, 42.97500000273117848, -31.93888565452638417 ) ) ;
#25500 = CARTESIAN_POINT ( 'NONE',  ( -10.37757302488623701, 19.77500000273118985, 31.93888565452638417 ) ) ;
#25501 = CARTESIAN_POINT ( 'NONE',  ( 32.50000000000000000, 41.00000000000000711, -3.980102097228898626E-15 ) ) ;
#25502 = CARTESIAN_POINT ( 'NONE',  ( -19.82091636218621034, 14.54999999453762705, -14.40073868116559552 ) ) ;
#25503 = CIRCLE ( 'NONE', #13460, 0.9999999999999988898 ) ;
#25504 = CARTESIAN_POINT ( 'NONE',  ( 0.000000000000000000, -23.00000000000000000, 0.000000000000000000 ) ) ;
#25505 = CARTESIAN_POINT ( 'NONE',  ( -20.08610463437156923, 62.29999999999997584, 27.64615127144130113 ) ) ;
#25506 = CARTESIAN_POINT ( 'NONE',  ( -23.41746824999999887, 9.524999997268810858, -7.608796670333730638 ) ) ;
#25507 = CARTESIAN_POINT ( 'NONE',  ( 10.37757302488624767, 65.72500000273117848, 31.93888565452638417 ) ) ;
#25508 = CARTESIAN_POINT ( 'NONE',  ( 19.11951029504797006, 32.90586833240934794, 19.06425588902558133 ) ) ;
#25509 = CARTESIAN_POINT ( 'NONE',  ( -33.58253175000000113, 79.37500000273119838, 0.000000000000000000 ) ) ;
#25510 = CARTESIAN_POINT ( 'NONE',  ( -27.16883889988624290, 6.925000002731191096, -19.73931689729374028 ) ) ;
#25511 = CARTESIAN_POINT ( 'NONE',  ( -14.47279130897151589, 9.824999997268802687, -19.92008829642072598 ) ) ;
#25512 = CARTESIAN_POINT ( 'NONE',  ( -6.988114217768288228, 60.41145833333332149, -26.07999730980477437 ) ) ;
#25513 = EDGE_CURVE ( 'NONE', #11893, #19899, #7371, .T. ) ;
#25514 = ORIENTED_EDGE ( 'NONE', *, *, #2396, .F. ) ;
#25515 = CARTESIAN_POINT ( 'NONE',  ( 10.37757302488624767, 49.72500000273117848, 31.93888565452638417 ) ) ;
#25516 = CARTESIAN_POINT ( 'NONE',  ( 20.75514604977248467, 24.67500000273118843, -28.56700777964554305 ) ) ;
#25517 = VERTEX_POINT ( 'NONE', #29905 ) ;
#25518 = CARTESIAN_POINT ( 'NONE',  ( 28.01184896238290278, 33.77083333333333570, -7.505752307973347470 ) ) ;
#25519 = CARTESIAN_POINT ( 'NONE',  ( -15.04653450569291984, 29.62277750092397355, 25.98046417659859486 ) ) ;
#25520 = CARTESIAN_POINT ( 'NONE',  ( 7.570916362186207671, 9.599999999999997868, 23.30088464923126779 ) ) ;
#25521 = CYLINDRICAL_SURFACE ( 'NONE', #19476, 12.00000000000000178 ) ;
#25522 = CARTESIAN_POINT ( 'NONE',  ( 23.41746825000000243, 5.224999997268802154, -7.608796670333727974 ) ) ;
#25523 = EDGE_CURVE ( 'NONE', #2254, #16950, #213, .T. ) ;
#25524 = EDGE_CURVE ( 'NONE', #21829, #25478, #20313, .T. ) ;
#25525 = CARTESIAN_POINT ( 'NONE',  ( -7.236395654485763274, 14.02499999726880553, 22.27133577429736633 ) ) ;
#25526 = CARTESIAN_POINT ( 'NONE',  ( -33.58253175000000113, 15.37500000273117706, 0.000000000000000000 ) ) ;
#25527 = CARTESIAN_POINT ( 'NONE',  ( 10.04305231718579705, 27.10000000546236620, 30.90933677959248982 ) ) ;
#25528 = CARTESIAN_POINT ( 'NONE',  ( -20.08610463437157989, 67.70000000000000284, -27.64615127144129758 ) ) ;
#25529 = CARTESIAN_POINT ( 'NONE',  ( 0.000000000000000000, 102.0000000000000284, -12.00000000000000178 ) ) ;
#25530 = CARTESIAN_POINT ( 'NONE',  ( -26.72982461517107566, 67.00000000000000000, -20.44820386143222635 ) ) ;
#25531 = CARTESIAN_POINT ( 'NONE',  ( 28.01184896238290278, 13.14583333333332860, -7.505752307973347470 ) ) ;
#25532 = CARTESIAN_POINT ( 'NONE',  ( -33.58253175000000113, 29.37500000273118772, 0.000000000000000000 ) ) ;
#25533 = FACE_OUTER_BOUND ( 'NONE', #7143, .T. ) ;
#25534 = CARTESIAN_POINT ( 'NONE',  ( -7.505752307972844761, 28.04166666666666075, 28.01184896238304134 ) ) ;
#25535 = CARTESIAN_POINT ( 'NONE',  ( -19.82091636218621034, 0.7999999999999951594, -14.40073868116559552 ) ) ;
#25536 = CARTESIAN_POINT ( 'NONE',  ( 10.04305231718579705, 6.599999999999994316, 30.90933677959248982 ) ) ;
#25537 = FACE_OUTER_BOUND ( 'NONE', #9282, .T. ) ;
#25538 = CARTESIAN_POINT ( 'NONE',  ( 19.11951029504797006, 56.96836833240936215, 19.06425588902558133 ) ) ;
#25539 = CARTESIAN_POINT ( 'NONE',  ( 20.75514604977248467, 54.42500000273117422, -28.56700777964554305 ) ) ;
#25540 = CIRCLE ( 'NONE', #23342, 26.50000000000000355 ) ;
#25541 = CARTESIAN_POINT ( 'NONE',  ( -27.16883889988624290, 65.17500000273116711, -19.73931689729374028 ) ) ;
#25542 = CARTESIAN_POINT ( 'NONE',  ( 33.58253175000000823, 42.27500000273118275, 10.91162601494192685 ) ) ;
#25543 = CARTESIAN_POINT ( 'NONE',  ( 7.236395654485760609, 15.02499999726880731, -22.27133577429736633 ) ) ;
#25544 = DIRECTION ( 'NONE',  ( 1.224646799147353454E-16, -1.000000000000000000, 0.000000000000000000 ) ) ;
#25545 = DIRECTION ( 'NONE',  ( -1.000000000000000000, -1.239088197126291063E-16, 0.000000000000000000 ) ) ;
#25546 = CARTESIAN_POINT ( 'NONE',  ( 22.82331083168796582, 16.99999999999998934, 5.297087881879605220 ) ) ;
#25547 = CARTESIAN_POINT ( 'NONE',  ( 10.04305231718578817, 79.40000000000000568, -30.90933677959249337 ) ) ;
#25548 = CARTESIAN_POINT ( 'NONE',  ( 33.58253175000000113, 22.22500000273117493, -10.91162601494193751 ) ) ;
#25549 = CARTESIAN_POINT ( 'NONE',  ( 4.300734207923757602, 80.77500000273118985, -13.23629886949340673 ) ) ;
#25550 = CARTESIAN_POINT ( 'NONE',  ( 20.08610463437158344, 55.20000000546238539, 27.64615127144129403 ) ) ;
#25551 = CARTESIAN_POINT ( 'NONE',  ( 0.000000000000000000, 0.000000000000000000, 24.50000000000000000 ) ) ;
#25552 = CARTESIAN_POINT ( 'NONE',  ( 7.543491769121922985, 60.69232666574269075, 28.00173670424535644 ) ) ;
#25553 = CARTESIAN_POINT ( 'NONE',  ( -20.08610463437156923, 38.80000000546237260, 27.64615127144130113 ) ) ;
#25554 = CARTESIAN_POINT ( 'NONE',  ( -20.50609665441004736, 67.00000000000000000, -20.50609665440969565 ) ) ;
#25555 = CARTESIAN_POINT ( 'NONE',  ( 27.16883889988624290, 33.92500000273118843, 19.73931689729373673 ) ) ;
#25556 = CARTESIAN_POINT ( 'NONE',  ( 26.07999730980490227, 37.49479166666666430, 6.988114217767821046 ) ) ;
#25557 = VERTEX_POINT ( 'NONE', #739 ) ;
#25558 = ORIENTED_EDGE ( 'NONE', *, *, #19308, .F. ) ;
#25559 = CARTESIAN_POINT ( 'NONE',  ( -27.16883889988623935, 67.32500000273118701, 19.73931689729374739 ) ) ;
#25560 = CARTESIAN_POINT ( 'NONE',  ( -15.01150461594642138, 36.20572916666666430, -26.00068869287340334 ) ) ;
#25561 = CARTESIAN_POINT ( 'NONE',  ( -1.778240108872766143E-15, 5.500000000000003553, -32.49999999999999289 ) ) ;
#25562 = ORIENTED_EDGE ( 'NONE', *, *, #10218, .F. ) ;
#25563 = CARTESIAN_POINT ( 'NONE',  ( 25.98046417659858420, 59.70090250092397355, 15.04653450569292872 ) ) ;
#25564 = CARTESIAN_POINT ( 'NONE',  ( -13.94119854578936923, 61.70611083425731636, -24.22776226481241224 ) ) ;
#25565 = CARTESIAN_POINT ( 'NONE',  ( -10.37757302488623701, 11.52500000273119696, 31.93888565452638417 ) ) ;
#25566 = CARTESIAN_POINT ( 'NONE',  ( 14.97647472619900455, 18.15326416574268720, -26.02091320914876960 ) ) ;
#25567 = CARTESIAN_POINT ( 'NONE',  ( 8.891200544363830713E-16, 79.75000000546238255, -15.00000000000000000 ) ) ;
#25568 = CARTESIAN_POINT ( 'NONE',  ( 33.58253175000000113, 44.37500000273119838, -4.112674001490185761E-15 ) ) ;
#25569 = CARTESIAN_POINT ( 'NONE',  ( 20.08610463437158344, 41.20000000546236407, 27.64615127144129403 ) ) ;
#25570 = CARTESIAN_POINT ( 'NONE',  ( -4.635254915624208216, 76.40000000000001990, 14.26584774442730463 ) ) ;
#25571 = CARTESIAN_POINT ( 'NONE',  ( -2.162160676586881955E-15, 24.62500000273118772, -35.31076352940723240 ) ) ;
#25572 = CARTESIAN_POINT ( 'NONE',  ( 7.570916362186207671, 13.34999999453762065, 23.30088464923126779 ) ) ;
#25573 = CARTESIAN_POINT ( 'NONE',  ( 33.58253175000000823, 46.27500000273120406, 10.91162601494192863 ) ) ;
#25574 = CARTESIAN_POINT ( 'NONE',  ( -2.092463501923844636E-15, 29.49999999999999645, -34.17252228774368916 ) ) ;
#25575 = CARTESIAN_POINT ( 'NONE',  ( -10.04305231718579172, 27.60000000000001208, -30.90933677959248982 ) ) ;
#25576 = CARTESIAN_POINT ( 'NONE',  ( -24.50000000000000000, 1.000000000000000888, -3.000384657911015469E-15 ) ) ;
#25577 = EDGE_CURVE ( 'NONE', #22733, #4956, #11226, .T. ) ;
#25578 = CARTESIAN_POINT ( 'NONE',  ( -33.58253175000000113, 79.12500000273119838, 0.000000000000000000 ) ) ;
#25579 = CARTESIAN_POINT ( 'NONE',  ( -11.25946833292375793, 75.17500000273119554, -8.180482586598733619 ) ) ;
#25580 = CARTESIAN_POINT ( 'NONE',  ( 6.486482029760648627E-15, 59.87500000273118417, 35.31076352940722529 ) ) ;
#25581 = CARTESIAN_POINT ( 'NONE',  ( 4.635254915624212657, 74.85000000546237686, 14.26584774442730286 ) ) ;
#25582 = ORIENTED_EDGE ( 'NONE', *, *, #20645, .F. ) ;
#25583 = CARTESIAN_POINT ( 'NONE',  ( 27.16883889988623935, 20.32500000273118701, -19.73931689729374384 ) ) ;
#25584 = CARTESIAN_POINT ( 'NONE',  ( -24.50000000000000355, 8.649999994537630243, -7.960532557706207157 ) ) ;
#25585 = CARTESIAN_POINT ( 'NONE',  ( 13.94119854578937812, 18.73736083425731636, 24.22776226481240514 ) ) ;
#25586 = CARTESIAN_POINT ( 'NONE',  ( 19.82091636218621389, 7.949999994537631842, -14.40073868116559197 ) ) ;
#25587 = CARTESIAN_POINT ( 'NONE',  ( 27.16883889988624290, 37.92500000273117422, 19.73931689729373673 ) ) ;
#25588 = CARTESIAN_POINT ( 'NONE',  ( -20.75514604977248823, 3.075000002731183901, -28.56700777964554305 ) ) ;
#25589 = CARTESIAN_POINT ( 'NONE',  ( 33.58253175000000113, 54.37500000273119838, -4.112674001490185761E-15 ) ) ;
#25590 = CARTESIAN_POINT ( 'NONE',  ( -7.468012846824771955, 44.66184000092397355, -28.02196122052045624 ) ) ;
#25591 = CARTESIAN_POINT ( 'NONE',  ( 19.82091636218621389, 16.19999999999999218, -14.40073868116559197 ) ) ;
#25592 = AXIS2_PLACEMENT_3D ( 'NONE', #33782, #13179, #5116 ) ;
#25593 = CARTESIAN_POINT ( 'NONE',  ( -28.02196122052058413, 41.21315999907602645, -7.468012846824272799 ) ) ;
#25594 = CARTESIAN_POINT ( 'NONE',  ( -10.04305231718578462, 58.90000000546240244, 30.90933677959249337 ) ) ;
#25595 = CARTESIAN_POINT ( 'NONE',  ( 11.25946833292375793, 80.57500000273121543, -8.180482586598735395 ) ) ;
#25596 = CARTESIAN_POINT ( 'NONE',  ( 5.779280353836490358E-15, 62.50000000000000000, 32.49999999999999289 ) ) ;
#25597 = CARTESIAN_POINT ( 'NONE',  ( 13.94119854578893580, 62.84076416574269786, -24.22776226481265383 ) ) ;
#25598 = CARTESIAN_POINT ( 'NONE',  ( -1.778240108872766143E-15, 58.00000000546237544, -32.49999999999999289 ) ) ;
#25599 = AXIS2_PLACEMENT_3D ( 'NONE', #22410, #32858, #6958 ) ;
#25600 = CARTESIAN_POINT ( 'NONE',  ( 26.29305231718578995, 73.70000000546239960, -19.10302069950538240 ) ) ;
#25601 = CARTESIAN_POINT ( 'NONE',  ( 9.270509831248425314, 78.70000000000001705, 12.75976212528059683 ) ) ;
#25602 = CARTESIAN_POINT ( 'NONE',  ( -33.58253175000000113, 33.47500000273119269, 10.91162601494193929 ) ) ;
#25603 = CARTESIAN_POINT ( 'NONE',  ( 23.41746824999999887, 5.224999997268801266, -7.608796670333727974 ) ) ;
#25604 = ORIENTED_EDGE ( 'NONE', *, *, #29081, .F. ) ;
#25605 = CARTESIAN_POINT ( 'NONE',  ( -33.58253175000000113, 75.47500000273116427, 10.91162601494193929 ) ) ;
#25606 = CARTESIAN_POINT ( 'NONE',  ( 32.50000000000000000, 23.50000000546238610, -3.980102097228898626E-15 ) ) ;
#25607 = CARTESIAN_POINT ( 'NONE',  ( 28.01184896238290278, 40.64583333333332860, -7.505752307973347470 ) ) ;
#25608 = CARTESIAN_POINT ( 'NONE',  ( 10.04305231718579705, 63.10000000546239818, 30.90933677959248982 ) ) ;
#25609 = ORIENTED_EDGE ( 'NONE', *, *, #24339, .F. ) ;
#25610 = DIRECTION ( 'NONE',  ( 0.000000000000000000, 0.000000000000000000, -1.000000000000000000 ) ) ;
#25611 = CARTESIAN_POINT ( 'NONE',  ( -33.58253175000000113, 43.02500000273118275, -10.91162601494193218 ) ) ;
#25612 = CARTESIAN_POINT ( 'NONE',  ( 23.41746824999999887, 18.62499999726882649, 0.000000000000000000 ) ) ;
#25613 = CARTESIAN_POINT ( 'NONE',  ( -32.50000000000000000, 6.400000005462388231, -10.55989012756945478 ) ) ;
#25614 = DIRECTION ( 'NONE',  ( 1.000000000000000000, 0.000000000000000000, 0.000000000000000000 ) ) ;
#25615 = CARTESIAN_POINT ( 'NONE',  ( 28.01184896238304134, 16.86979166666666075, 7.505752307972846538 ) ) ;
#25616 = CARTESIAN_POINT ( 'NONE',  ( 32.50000000000000000, 46.99999999999998579, -3.980102097228898626E-15 ) ) ;
#25617 = EDGE_CURVE ( 'NONE', #5086, #27857, #8424, .T. ) ;
#25618 = CARTESIAN_POINT ( 'NONE',  ( -18.94512977948576093, 1.824999997268816898, 13.76444248337722698 ) ) ;
#25619 = CARTESIAN_POINT ( 'NONE',  ( -20.75514604977248823, 15.07500000273116747, -28.56700777964554305 ) ) ;
#25620 = CYLINDRICAL_SURFACE ( 'NONE', #14560, 24.50000000000000000 ) ;
#25621 = CARTESIAN_POINT ( 'NONE',  ( -7.025853678916861966, 21.16107666574269075, -26.06988505166722803 ) ) ;
#25622 = CARTESIAN_POINT ( 'NONE',  ( 4.300734207923757602, 76.77500000273118985, -13.23629886949340673 ) ) ;
#25623 = CARTESIAN_POINT ( 'NONE',  ( -4.223320258572819786E-15, 3.500000000000004441, 24.50000000000000000 ) ) ;
#25624 = CARTESIAN_POINT ( 'NONE',  ( 32.50000000000000000, 53.60000000546238397, -10.55989012756945833 ) ) ;
#25625 = ADVANCED_FACE ( 'NONE', ( #9830 ), #27680, .F. ) ;
#25626 = CARTESIAN_POINT ( 'NONE',  ( -27.16883889988624290, 73.17500000273118133, -19.73931689729374028 ) ) ;
#25627 = ORIENTED_EDGE ( 'NONE', *, *, #618, .F. ) ;
#25628 = CARTESIAN_POINT ( 'NONE',  ( -18.94512977948576093, 10.32499999726882400, 13.76444248337722698 ) ) ;
#25629 = CARTESIAN_POINT ( 'NONE',  ( -7.236395654485763274, 4.024999997268824181, 22.27133577429736633 ) ) ;
#25630 = CARTESIAN_POINT ( 'NONE',  ( 2.584737979205441561E-13, 51.96093750000000000, 27.95245687107222921 ) ) ;
#25631 = CARTESIAN_POINT ( 'NONE',  ( 10.37757302488624056, 58.52500000273118275, -31.93888565452638417 ) ) ;
#25632 = CARTESIAN_POINT ( 'NONE',  ( 33.58253175000000113, 26.47500000273118559, -10.91162601494193751 ) ) ;
#25633 = CARTESIAN_POINT ( 'NONE',  ( -20.75514604977248823, 13.07500000273118879, -28.56700777964554305 ) ) ;
#25634 = CARTESIAN_POINT ( 'NONE',  ( -6.988114217767819270, 31.47916666666666075, 26.07999730980490583 ) ) ;
#25635 = CARTESIAN_POINT ( 'NONE',  ( 26.02091320914851025, 21.31548583425730925, -14.97647472619946463 ) ) ;
#25636 = CARTESIAN_POINT ( 'NONE',  ( 28.01184896238290278, 64.70833333333334281, -7.505752307973347470 ) ) ;
#25637 = CARTESIAN_POINT ( 'NONE',  ( -20.75514604977248112, 5.425000002731182214, 28.56700777964554661 ) ) ;
#25638 = CARTESIAN_POINT ( 'NONE',  ( -13.91746824999999532, 71.47500000273120691, 4.522059556121122093 ) ) ;
#25639 = CARTESIAN_POINT ( 'NONE',  ( -20.08610463437157989, 41.69999999999999574, -27.64615127144129758 ) ) ;
#25640 = CARTESIAN_POINT ( 'NONE',  ( -27.16883889988623935, 47.32500000273117990, 19.73931689729374739 ) ) ;
#25641 = CARTESIAN_POINT ( 'NONE',  ( -23.41746825000000598, 7.724999997268809260, 7.608796670333726198 ) ) ;
#25642 = CARTESIAN_POINT ( 'NONE',  ( 12.13525491562421088, 78.80000000000001137, 8.816778784387095058 ) ) ;
#25643 = VERTEX_POINT ( 'NONE', #4337 ) ;
#25644 = CARTESIAN_POINT ( 'NONE',  ( 33.58253175000000113, 56.47500000273116427, -10.91162601494193751 ) ) ;
#25645 = CARTESIAN_POINT ( 'NONE',  ( 5.779280353836490358E-15, 59.00000000546238255, 32.49999999999999289 ) ) ;
#25646 = CARTESIAN_POINT ( 'NONE',  ( -26.09010956794232428, 43.80246500092398776, 6.950374756619732253 ) ) ;
#25647 = CARTESIAN_POINT ( 'NONE',  ( 27.16883889988624290, 78.17500000273119554, 19.73931689729373673 ) ) ;
#25648 = VERTEX_POINT ( 'NONE', #4508 ) ;
#25649 = CARTESIAN_POINT ( 'NONE',  ( -27.16883889988623935, 21.32500000273117280, 19.73931689729374739 ) ) ;
#25650 = CARTESIAN_POINT ( 'NONE',  ( 15.01150461594596308, 12.71614583333333037, -26.00068869287367335 ) ) ;
#25651 = VERTEX_POINT ( 'NONE', #7426 ) ;
#25652 = DIRECTION ( 'NONE',  ( -0.000000000000000000, -1.000000000000000000, -0.000000000000000000 ) ) ;
#25653 = CARTESIAN_POINT ( 'NONE',  ( 33.58253175000000113, 68.22500000273116427, -10.91162601494193751 ) ) ;
#25654 = CARTESIAN_POINT ( 'NONE',  ( 20.50609665441005092, 37.78124999999999289, 20.50609665440969209 ) ) ;
#25655 = CARTESIAN_POINT ( 'NONE',  ( -4.732186688966233175E-15, 9.499999999999991118, 25.76082449383753925 ) ) ;
#25656 = CARTESIAN_POINT ( 'NONE',  ( 7.236395654485760609, 3.524999997268824181, -22.27133577429736633 ) ) ;
#25657 = CARTESIAN_POINT ( 'NONE',  ( -20.75514604977248112, 9.425000002731202642, 28.56700777964554661 ) ) ;
#25658 = CARTESIAN_POINT ( 'NONE',  ( -19.82091636218621389, 6.949999994537630954, 14.40073868116558842 ) ) ;
#25659 = CARTESIAN_POINT ( 'NONE',  ( 15.04653450569339945, 50.23659749907603356, 25.98046417659831775 ) ) ;
#25660 = CARTESIAN_POINT ( 'NONE',  ( -15.00000000000000000, 73.90000000000003411, -4.873795443493594171 ) ) ;
#25661 = CARTESIAN_POINT ( 'NONE',  ( 28.01184896238304134, 64.99479166666665719, 7.505752307972846538 ) ) ;
#25662 = CARTESIAN_POINT ( 'NONE',  ( -24.50000000000000000, 14.64999999453761603, -7.960532557706207157 ) ) ;
#25663 = CARTESIAN_POINT ( 'NONE',  ( -5.147494310547531704, 52.44874571845314648, 32.49999999999996447 ) ) ;
#25664 = CARTESIAN_POINT ( 'NONE',  ( 7.570916362186207671, 15.34999999453762243, 23.30088464923126779 ) ) ;
#25665 = CARTESIAN_POINT ( 'NONE',  ( 15.00000000000000000, 73.25000000546239676, -1.836970198721029589E-15 ) ) ;
#25666 = CARTESIAN_POINT ( 'NONE',  ( 13.97622843553589966, 23.02864583333332149, -24.20753774853756113 ) ) ;
#25667 = CARTESIAN_POINT ( 'NONE',  ( -20.75514604977248823, 30.82500000273119767, -28.56700777964554305 ) ) ;
#25668 = CARTESIAN_POINT ( 'NONE',  ( 33.58253175000000113, 78.12500000273118417, -4.112674001490185761E-15 ) ) ;
#25669 = CARTESIAN_POINT ( 'NONE',  ( -10.37757302488623701, 41.77500000273119696, 31.93888565452638417 ) ) ;
#25670 = CARTESIAN_POINT ( 'NONE',  ( -20.75514604977248112, 21.67500000273119198, 28.56700777964554661 ) ) ;
#25671 = CARTESIAN_POINT ( 'NONE',  ( -26.29305231718578995, 68.19999999999998863, 19.10302069950538595 ) ) ;
#25672 = CARTESIAN_POINT ( 'NONE',  ( -10.37757302488623701, 73.52500000273121827, 31.93888565452638417 ) ) ;
#25673 = CARTESIAN_POINT ( 'NONE',  ( 32.50000000000000711, 58.90000000000000568, 10.55989012756945122 ) ) ;
#25674 = CARTESIAN_POINT ( 'NONE',  ( -4.000000000000003553, 0.000000000000000000, 30.00000000000004974 ) ) ;
#25675 = CARTESIAN_POINT ( 'NONE',  ( -33.58253175000000113, 67.12500000273119838, 0.000000000000000000 ) ) ;
#25676 = CARTESIAN_POINT ( 'NONE',  ( -18.94512977948576093, 10.32499999726882400, 13.76444248337722698 ) ) ;
#25677 = EDGE_CURVE ( 'NONE', #2966, #16286, #11975, .T. ) ;
#25678 = CARTESIAN_POINT ( 'NONE',  ( 20.75514604977249178, 74.07500000273120122, 28.56700777964553950 ) ) ;
#25679 = CARTESIAN_POINT ( 'NONE',  ( 6.486482029760648627E-15, 9.625000002731196602, 35.31076352940722529 ) ) ;
#25680 = CARTESIAN_POINT ( 'NONE',  ( 1.507698388325705758E-15, 11.62499999726880340, -24.62258325217400312 ) ) ;
#25681 = CARTESIAN_POINT ( 'NONE',  ( 19.09188309203661049, 64.42187499999998579, -19.09188309203694445 ) ) ;
#25682 = ORIENTED_EDGE ( 'NONE', *, *, #2853, .T. ) ;
#25683 = CARTESIAN_POINT ( 'NONE',  ( -10.37757302488623701, 47.52500000273117564, 31.93888565452638417 ) ) ;
#25684 = ORIENTED_EDGE ( 'NONE', *, *, #21442, .F. ) ;
#25685 = CARTESIAN_POINT ( 'NONE',  ( -26.00068869287340334, 31.90885416666666430, 15.01150461594643382 ) ) ;
#25686 = DIRECTION ( 'NONE',  ( -1.224646799147353454E-16, 1.000000000000000000, -0.000000000000000000 ) ) ;
#25687 = CARTESIAN_POINT ( 'NONE',  ( 10.04305231718578817, 13.90000000546236159, -30.90933677959249337 ) ) ;
#25688 = CARTESIAN_POINT ( 'NONE',  ( 5.334720326618300005E-14, 72.00000000546238255, -32.50000000000000000 ) ) ;
#25689 = CARTESIAN_POINT ( 'NONE',  ( 7.236395654485760609, 5.524999997268825958, -22.27133577429736633 ) ) ;
#25690 = CARTESIAN_POINT ( 'NONE',  ( 23.41746825000000243, 14.72499999726881903, -7.608796670333727974 ) ) ;
#25691 = CARTESIAN_POINT ( 'NONE',  ( -33.58253175000000113, 17.27500000273118630, -10.91162601494193218 ) ) ;
#25692 = CARTESIAN_POINT ( 'NONE',  ( 26.29305231718578995, 17.70000000546237473, -19.10302069950538240 ) ) ;
#25693 = CARTESIAN_POINT ( 'NONE',  ( 32.50000000000000000, 63.10000000000001563, -10.55989012756945833 ) ) ;
#25694 = CARTESIAN_POINT ( 'NONE',  ( 15.00000000000000355, 77.15000000546240244, 4.873795443493592394 ) ) ;
#25695 = CARTESIAN_POINT ( 'NONE',  ( 26.29305231718578995, 73.70000000546239960, -19.10302069950538240 ) ) ;
#25696 = CARTESIAN_POINT ( 'NONE',  ( 2.740863092043355209E-13, 14.14843749999999289, 30.02300923189239512 ) ) ;
#25697 = CARTESIAN_POINT ( 'NONE',  ( -2.162160676586881955E-15, 30.87500000273119483, -35.31076352940723240 ) ) ;
#25698 = CARTESIAN_POINT ( 'NONE',  ( -10.04305231718578462, 32.90000000546239534, 30.90933677959249337 ) ) ;
#25699 = CARTESIAN_POINT ( 'NONE',  ( -26.00068869287368756, 35.91927083333332860, -15.01150461594595775 ) ) ;
#25700 = DIRECTION ( 'NONE',  ( 1.000000000000000000, 0.000000000000000000, 0.000000000000000000 ) ) ;
#25701 = CARTESIAN_POINT ( 'NONE',  ( 1.507698388325705758E-15, 13.62499999726882827, -24.62258325217400312 ) ) ;
#25702 = CARTESIAN_POINT ( 'NONE',  ( -26.29305231718578995, 8.199999999999985079, 19.10302069950538595 ) ) ;
#25703 = CARTESIAN_POINT ( 'NONE',  ( 7.570916362186213000, 16.39999999999999858, -23.30088464923126423 ) ) ;
#25704 = CARTESIAN_POINT ( 'NONE',  ( -0.04044903255042732459, 55.67930583240935505, -27.95245687107223986 ) ) ;
#25705 = CARTESIAN_POINT ( 'NONE',  ( 27.16883889988623935, 50.32500000273118701, -19.73931689729374384 ) ) ;
#25706 = CARTESIAN_POINT ( 'NONE',  ( -20.75514604977248112, 61.67500000273117422, 28.56700777964554661 ) ) ;
#25707 = CARTESIAN_POINT ( 'NONE',  ( 33.58253175000000113, 42.47500000273119980, -10.91162601494193574 ) ) ;
#25708 = CARTESIAN_POINT ( 'NONE',  ( -1.778240108872766143E-15, 13.50000000000000355, -32.49999999999999289 ) ) ;
#25709 = ADVANCED_FACE ( 'NONE', ( #19786 ), #17390, .T. ) ;
#25710 = CARTESIAN_POINT ( 'NONE',  ( -13.97622843553588901, 14.43489583333332860, 24.20753774853756823 ) ) ;
#25711 = CARTESIAN_POINT ( 'NONE',  ( 5.779280353836490358E-15, 62.50000000000000000, 32.49999999999999289 ) ) ;
#25712 = DIRECTION ( 'NONE',  ( -1.000000000000000000, -1.122425893913996568E-16, 0.000000000000000000 ) ) ;
#25713 = CARTESIAN_POINT ( 'NONE',  ( 20.75514604977249178, 15.82500000273117102, 28.56700777964553950 ) ) ;
#25714 = CARTESIAN_POINT ( 'NONE',  ( 5.779280353836490358E-15, 6.500000000000002665, 32.49999999999999289 ) ) ;
#25715 = DIRECTION ( 'NONE',  ( 0.000000000000000000, -1.000000000000000000, 0.000000000000000000 ) ) ;
#25716 = EDGE_CURVE ( 'NONE', #30177, #2261, #64, .T. ) ;
#25717 = FACE_OUTER_BOUND ( 'NONE', #29968, .T. ) ;
#25718 = CARTESIAN_POINT ( 'NONE',  ( -24.18731323226221974, 23.59597249907602290, 14.01125832528330406 ) ) ;
#25719 = CARTESIAN_POINT ( 'NONE',  ( -32.50000000000000000, 42.50000000546237544, 0.000000000000000000 ) ) ;
#25720 = CARTESIAN_POINT ( 'NONE',  ( 20.08610463437157279, 11.29999999999999361, -27.64615127144129758 ) ) ;
#25721 = CARTESIAN_POINT ( 'NONE',  ( -33.58253175000000113, 27.02500000273119340, -10.91162601494193041 ) ) ;
#25722 = CARTESIAN_POINT ( 'NONE',  ( -6.988114217767819270, 38.35416666666666430, 26.07999730980490583 ) ) ;
#25723 = EDGE_CURVE ( 'NONE', #33045, #1732, #27317, .T. ) ;
#25724 = ORIENTED_EDGE ( 'NONE', *, *, #13072, .T. ) ;
#25725 = CARTESIAN_POINT ( 'NONE',  ( 27.16883889988623935, 70.32500000273118701, -19.73931689729374384 ) ) ;
#25726 = CARTESIAN_POINT ( 'NONE',  ( -20.50609665441004736, 36.06250000000000000, -20.50609665440969565 ) ) ;
#25727 = CARTESIAN_POINT ( 'NONE',  ( 0.000000000000000000, 122.0000000000000000, 0.000000000000000000 ) ) ;
#25728 = ORIENTED_EDGE ( 'NONE', *, *, #25377, .F. ) ;
#25729 = CARTESIAN_POINT ( 'NONE',  ( -28.02196122052045268, 57.55246500092398065, 7.468012846824790607 ) ) ;
#25730 = CARTESIAN_POINT ( 'NONE',  ( 7.025853678916403666, 58.69829833425730925, -26.06988505166735237 ) ) ;
#25731 = CARTESIAN_POINT ( 'NONE',  ( -2.162160676586881955E-15, 10.62500000273119127, -35.31076352940723240 ) ) ;
#25732 = CARTESIAN_POINT ( 'NONE',  ( -20.53372385742107653, 17.43711833240935505, -20.47846945139867003 ) ) ;
#25733 = DIRECTION ( 'NONE',  ( 1.224646799147353454E-16, -1.000000000000000000, 0.000000000000000000 ) ) ;
#25734 = CARTESIAN_POINT ( 'NONE',  ( 20.75514604977249178, 36.07500000273117990, 28.56700777964553950 ) ) ;
#25735 = CARTESIAN_POINT ( 'NONE',  ( 6.277390505771533514E-15, 45.00000000546235412, 34.17252228774368916 ) ) ;
#25736 = CARTESIAN_POINT ( 'NONE',  ( 9.270509831248423538, 75.30000000000001137, -12.75976212528059861 ) ) ;
#25737 = CARTESIAN_POINT ( 'NONE',  ( -27.16883889988623935, 23.32500000273118701, 19.73931689729374739 ) ) ;
#25738 = CARTESIAN_POINT ( 'NONE',  ( 7.570916362186213000, 14.14999999453761603, -23.30088464923126423 ) ) ;
#25739 = CARTESIAN_POINT ( 'NONE',  ( -20.75514604977248823, 51.07500000273116569, -28.56700777964554305 ) ) ;
#25740 = CARTESIAN_POINT ( 'NONE',  ( 26.29305231718578995, 31.19999999999999218, -19.10302069950538240 ) ) ;
#25741 = CARTESIAN_POINT ( 'NONE',  ( 6.277390505771533514E-15, 28.50000000000000000, 34.17252228774368916 ) ) ;
#25742 = CARTESIAN_POINT ( 'NONE',  ( 1.507698388325705758E-15, 15.12499999726880873, -24.62258325217400312 ) ) ;
#25743 = CARTESIAN_POINT ( 'NONE',  ( -33.58253175000000113, 69.22500000273117848, 10.91162601494193929 ) ) ;
#25744 = CARTESIAN_POINT ( 'NONE',  ( -9.358181289160242500, 66.99999999999998579, 31.32043657353317201 ) ) ;
#25745 = FACE_OUTER_BOUND ( 'NONE', #17761, .T. ) ;
#25746 = CARTESIAN_POINT ( 'NONE',  ( -10.37757302488624411, 60.97500000273120691, -31.93888565452638417 ) ) ;
#25747 = CARTESIAN_POINT ( 'NONE',  ( -12.13525491562420910, 72.45000000546237118, 8.816778784387098611 ) ) ;
#25748 = CARTESIAN_POINT ( 'NONE',  ( -32.50000000000000000, 40.40000000546239534, -10.55989012756945300 ) ) ;
#25749 = CARTESIAN_POINT ( 'NONE',  ( -27.16883889988624290, 16.92500000273117067, -19.73931689729374028 ) ) ;
#25750 = CARTESIAN_POINT ( 'NONE',  ( 15.14183272437242245, 10.04999999453761639, -20.84094480462497856 ) ) ;
#25751 = CARTESIAN_POINT ( 'NONE',  ( -19.06425588902591173, 20.31288166759063785, -19.11951029504763611 ) ) ;
#25752 = CARTESIAN_POINT ( 'NONE',  ( -15.00000000000000000, 74.15000000546240244, -4.873795443493594171 ) ) ;
#25753 = CARTESIAN_POINT ( 'NONE',  ( 33.58253175000000823, 40.02500000273119696, 10.91162601494192863 ) ) ;
#25754 = CARTESIAN_POINT ( 'NONE',  ( 5.779280353836490358E-15, 65.00000000546236834, 32.49999999999999289 ) ) ;
#25755 = CARTESIAN_POINT ( 'NONE',  ( 20.75514604977248467, 52.67500000273116711, -28.56700777964554305 ) ) ;
#25756 = CARTESIAN_POINT ( 'NONE',  ( -20.53372385742071771, 50.39100666759063785, 20.47846945139902530 ) ) ;
#25757 = CARTESIAN_POINT ( 'NONE',  ( -1.778240108872766143E-15, 65.50000000000000000, -32.49999999999999289 ) ) ;
#25758 = CARTESIAN_POINT ( 'NONE',  ( -20.53372385742107653, 41.49961833240934794, -20.47846945139867003 ) ) ;
#25759 = CARTESIAN_POINT ( 'NONE',  ( 10.04305231718578817, 63.90000000546238113, -30.90933677959249337 ) ) ;
#25760 = CARTESIAN_POINT ( 'NONE',  ( -8.601468415847515203, 77.67500000273122396, 11.83890561707634959 ) ) ;
#25761 = CARTESIAN_POINT ( 'NONE',  ( -3.880418787951138260, 3.198745712990784806, 24.50000000000000000 ) ) ;
#25762 = CARTESIAN_POINT ( 'NONE',  ( 14.01125832528330051, 67.42409749907601224, 24.18731323226221974 ) ) ;
#25763 = CARTESIAN_POINT ( 'NONE',  ( 5.147494310547380714, 63.05125428700923607, 32.50000000000002132 ) ) ;
#25764 = CARTESIAN_POINT ( 'NONE',  ( -10.04305231718578462, 74.90000000546237402, 30.90933677959249337 ) ) ;
#25765 = DIRECTION ( 'NONE',  ( 0.8660254037844387076, 0.000000000000000000, -0.4999999999999998890 ) ) ;
#25766 = CARTESIAN_POINT ( 'NONE',  ( -10.37757302488624411, 32.97500000273119269, -31.93888565452638417 ) ) ;
#25767 = CARTESIAN_POINT ( 'NONE',  ( -7.236395654485763274, 6.524999997268826846, 22.27133577429736633 ) ) ;
#25768 = ORIENTED_EDGE ( 'NONE', *, *, #1215, .T. ) ;
#25769 = CARTESIAN_POINT ( 'NONE',  ( 33.58253175000000113, 76.37500000273116996, -4.112674001490185761E-15 ) ) ;
#25770 = CARTESIAN_POINT ( 'NONE',  ( 20.08610463437157279, 25.80000000546239036, -27.64615127144129758 ) ) ;
#25771 = CARTESIAN_POINT ( 'NONE',  ( -7.505752307972844761, 45.22916666666665719, 28.01184896238304134 ) ) ;
#25772 = CARTESIAN_POINT ( 'NONE',  ( 30.02300923189239512, 57.97656249999997868, -2.619432448724977703E-13 ) ) ;
#25773 = CARTESIAN_POINT ( 'NONE',  ( 27.16883889988624290, 54.17500000273117422, 19.73931689729373673 ) ) ;
#25774 = CARTESIAN_POINT ( 'NONE',  ( -20.08610463437157989, 62.20000000546237828, -27.64615127144129758 ) ) ;
#25775 = EDGE_LOOP ( 'NONE', ( #1222, #17753, #26742, #22507 ) ) ;
#25776 = CARTESIAN_POINT ( 'NONE',  ( -10.04305231718579172, 10.10000000546237864, -30.90933677959248982 ) ) ;
#25777 = CARTESIAN_POINT ( 'NONE',  ( 33.58253175000000113, 44.12500000273117706, -4.112674001490185761E-15 ) ) ;
#25778 = CARTESIAN_POINT ( 'NONE',  ( 20.75514604977248467, 66.67500000273119554, -28.56700777964554305 ) ) ;
#25779 = CARTESIAN_POINT ( 'NONE',  ( 26.29305231718578995, 5.700000005462390718, -19.10302069950538240 ) ) ;
#25780 = CARTESIAN_POINT ( 'NONE',  ( -2.162160676586882350E-15, 58.62500000273118417, -35.31076352940722529 ) ) ;
#25781 = DIRECTION ( 'NONE',  ( 0.000000000000000000, 0.000000000000000000, -1.000000000000000000 ) ) ;
#25782 = CARTESIAN_POINT ( 'NONE',  ( -32.50000000000000000, 48.09999999999999432, 10.55989012756946366 ) ) ;
#25783 = CARTESIAN_POINT ( 'NONE',  ( 20.75514604977248467, 12.67500000273118488, -28.56700777964554305 ) ) ;
#25784 = LINE ( 'NONE', #33679, #6881 ) ;
#25785 = CARTESIAN_POINT ( 'NONE',  ( 26.06988505166722803, 28.89545166574268009, -7.025853678916862854 ) ) ;
#25786 = CARTESIAN_POINT ( 'NONE',  ( 11.25946833292375793, 80.57500000273121543, -8.180482586598735395 ) ) ;
#25787 = CARTESIAN_POINT ( 'NONE',  ( 33.58253175000000113, 78.47500000273116427, -10.91162601494193574 ) ) ;
#25788 = CARTESIAN_POINT ( 'NONE',  ( -10.04305231718578462, 22.40000000000000213, 30.90933677959249337 ) ) ;
#25789 = CARTESIAN_POINT ( 'NONE',  ( -10.37757302488624411, 74.97500000273120691, -31.93888565452638417 ) ) ;
#25790 = EDGE_LOOP ( 'NONE', ( #11412, #11451, #3487, #1257 ) ) ;
#25791 = CARTESIAN_POINT ( 'NONE',  ( 14.47279130897151589, 10.82499999726882756, 19.92008829642072953 ) ) ;
#25792 = CARTESIAN_POINT ( 'NONE',  ( -18.94512977948575738, 3.424999997268807217, -13.76444248337723231 ) ) ;
#25793 = CARTESIAN_POINT ( 'NONE',  ( 19.09188309203661049, 54.10937499999999289, -19.09188309203694445 ) ) ;
#25794 = CARTESIAN_POINT ( 'NONE',  ( -2.162160676586881955E-15, 62.62500000273116996, -35.31076352940723240 ) ) ;
#25795 = CARTESIAN_POINT ( 'NONE',  ( 33.58253175000000823, 18.27500000273118275, 10.91162601494192863 ) ) ;
#25796 = CARTESIAN_POINT ( 'NONE',  ( 27.16883889988623935, 8.575000002731188786, -19.73931689729374384 ) ) ;
#25797 = CARTESIAN_POINT ( 'NONE',  ( -19.09188309203660694, 31.76562499999999289, 19.09188309203694800 ) ) ;
#25798 = CARTESIAN_POINT ( 'NONE',  ( -30.02300923189239867, 23.32069416759064140, -0.04044903254991731589 ) ) ;
#25799 = CARTESIAN_POINT ( 'NONE',  ( -28.01184896238304134, 63.27604166666667140, -7.505752307972844761 ) ) ;
#25800 = CARTESIAN_POINT ( 'NONE',  ( 20.75514604977248467, 2.425000002731189763, -28.56700777964554305 ) ) ;
#25801 = CARTESIAN_POINT ( 'NONE',  ( -11.25946833292375793, 73.57500000273120122, 8.180482586598737171 ) ) ;
#25802 = CARTESIAN_POINT ( 'NONE',  ( 32.50000000000000000, 41.10000000000001563, -10.55989012756945833 ) ) ;
#25803 = CARTESIAN_POINT ( 'NONE',  ( 27.16883889988624290, 45.92500000273119554, 19.73931689729373673 ) ) ;
#25804 = CARTESIAN_POINT ( 'NONE',  ( 14.47279130897151589, 10.32499999726881335, 19.92008829642072953 ) ) ;
#25805 = FACE_OUTER_BOUND ( 'NONE', #893, .T. ) ;
#25806 = EDGE_LOOP ( 'NONE', ( #14837, #25768, #27746, #9246 ) ) ;
#25807 = EDGE_CURVE ( 'NONE', #30562, #17974, #5173, .T. ) ;
#25808 = CARTESIAN_POINT ( 'NONE',  ( 33.58253175000000113, 52.37500000273119838, -4.112674001490185761E-15 ) ) ;
#25809 = DIRECTION ( 'NONE',  ( -0.000000000000000000, 1.000000000000000000, -0.000000000000000000 ) ) ;
#25810 = CARTESIAN_POINT ( 'NONE',  ( -7.025853678916393008, 39.79204833425731636, 26.06988505166735592 ) ) ;
#25811 = CARTESIAN_POINT ( 'NONE',  ( -33.58253175000000113, 75.27500000273118985, -10.91162601494193218 ) ) ;
#25812 = ADVANCED_FACE ( 'NONE', ( #28527 ), #20664, .F. ) ;
#25813 = EDGE_LOOP ( 'NONE', ( #5732, #24005, #33685, #10792 ) ) ;
#25814 = CARTESIAN_POINT ( 'NONE',  ( -10.37757302488624411, 24.72500000273118559, -31.93888565452638417 ) ) ;
#25815 = CARTESIAN_POINT ( 'NONE',  ( 15.01150461594643204, 13.86197916666666430, 26.00068869287340334 ) ) ;
#25816 = VERTEX_POINT ( 'NONE', #371 ) ;
#25817 =( BOUNDED_CURVE ( )  B_SPLINE_CURVE ( 2, ( #15258, #32907, #30682, #25720, #2200, #32745, #10789, #10618, #18014, #13023, #28800, #26235, #20924 ),
 .UNSPECIFIED., .F., .T. ) 
 B_SPLINE_CURVE_WITH_KNOTS ( ( 3, 2, 2, 2, 2, 2, 3 ),
 ( 0.8782051282051281937, 0.8794871794871794712, 0.8820512820512820262, 0.8846153846153845812, 0.8871794871794871362, 0.8897435897435896912, 0.8910256410256410797 ),
 .UNSPECIFIED. ) 
 CURVE ( )  GEOMETRIC_REPRESENTATION_ITEM ( )  RATIONAL_B_SPLINE_CURVE ( ( 0.9755282581475768211, 0.9755282581475768211, 1.000000000000000000, 0.9510565162951535312, 1.000000000000000000, 0.9510565162951535312, 1.000000000000000000, 0.9510565162951535312, 1.000000000000000000, 0.9510565162951535312, 1.000000000000000000, 0.9755282581475757109, 0.9755282581475768211 ) ) 
 REPRESENTATION_ITEM ( '' )  );
#25818 = CARTESIAN_POINT ( 'NONE',  ( 33.58253175000000113, 62.22500000273119269, -10.91162601494193751 ) ) ;
#25819 = CARTESIAN_POINT ( 'NONE',  ( -15.01150461594595775, 35.05989583333332860, 26.00068869287368756 ) ) ;
#25820 = CARTESIAN_POINT ( 'NONE',  ( -19.82091636218621034, 16.80000000000000782, -14.40073868116559552 ) ) ;
#25821 = DIRECTION ( 'NONE',  ( -0.000000000000000000, -1.000000000000000000, -0.000000000000000000 ) ) ;
#25822 = VECTOR ( 'NONE', #1000, 1000.000000000000000 ) ;
#25823 = CARTESIAN_POINT ( 'NONE',  ( 33.58253175000000113, 8.125000002731198379, -4.112674001490185761E-15 ) ) ;
#25824 = CARTESIAN_POINT ( 'NONE',  ( -0.04044903255044120238, 55.67930583240935505, -30.02300923189239867 ) ) ;
#25825 = CARTESIAN_POINT ( 'NONE',  ( -15.00000000000000000, 76.10000000000002274, 4.873795443493597723 ) ) ;
#25826 = CARTESIAN_POINT ( 'NONE',  ( -15.01150461594642316, 63.70572916666667140, -26.00068869287341045 ) ) ;
#25827 = CARTESIAN_POINT ( 'NONE',  ( -4.223320258572819786E-15, 15.24999999453762278, 24.50000000000000000 ) ) ;
#25828 = CARTESIAN_POINT ( 'NONE',  ( 32.50000000000000000, 19.10000000000000497, -10.55989012756945833 ) ) ;
#25829 = CARTESIAN_POINT ( 'NONE',  ( -24.50000000000001066, 12.84999999453761532, 7.960532557706201828 ) ) ;
#25830 = CARTESIAN_POINT ( 'NONE',  ( 12.13525491562421088, 73.05000000546237970, 8.816778784387095058 ) ) ;
#25831 = CARTESIAN_POINT ( 'NONE',  ( 6.988114217768294445, 20.88020833333333215, 26.07999730980477437 ) ) ;
#25832 = CARTESIAN_POINT ( 'NONE',  ( 27.16883889988624290, 31.92500000273118488, 19.73931689729373673 ) ) ;
#25833 = CARTESIAN_POINT ( 'NONE',  ( -2.162160676586881955E-15, 76.62500000273118417, -35.31076352940723240 ) ) ;
#25834 = AXIS2_PLACEMENT_3D ( 'NONE', #23818, #26045, #33774 ) ;
#25835 = VECTOR ( 'NONE', #14889, 1000.000000000000114 ) ;
#25836 = CARTESIAN_POINT ( 'NONE',  ( -2.162160676586881955E-15, 44.87500000273119127, -35.31076352940723240 ) ) ;
#25837 = CARTESIAN_POINT ( 'NONE',  ( -33.58253175000000113, 21.27500000273117564, -10.91162601494193041 ) ) ;
#25838 = CARTESIAN_POINT ( 'NONE',  ( -20.08610463437157989, 67.70000000000000284, -27.64615127144129758 ) ) ;
#25839 = CARTESIAN_POINT ( 'NONE',  ( 6.486482029760648627E-15, 77.62500000273119838, 35.31076352940722529 ) ) ;
#25840 = CARTESIAN_POINT ( 'NONE',  ( 5.147494310547481966, 59.94874572391551482, -32.49999999999998579 ) ) ;
#25841 = CARTESIAN_POINT ( 'NONE',  ( 26.29305231718579350, 60.80000000000000426, 19.10302069950537529 ) ) ;
#25842 = CARTESIAN_POINT ( 'NONE',  ( -23.41746824999999887, 17.62499999726882649, -2.867812753649727150E-15 ) ) ;
#25843 = CARTESIAN_POINT ( 'NONE',  ( 33.58253175000000823, 62.02500000273116854, 10.91162601494192685 ) ) ;
#25844 = CARTESIAN_POINT ( 'NONE',  ( -7.236395654485763274, 10.52499999726880198, 22.27133577429736633 ) ) ;
#25845 = CARTESIAN_POINT ( 'NONE',  ( -20.75514604977248112, 71.67500000273116711, 28.56700777964554661 ) ) ;
#25846 = CARTESIAN_POINT ( 'NONE',  ( 10.37757302488624767, 5.725000002731183812, 31.93888565452638417 ) ) ;
#25847 = CARTESIAN_POINT ( 'NONE',  ( -23.41746824999999887, 18.12499999726882649, -2.867812753649727150E-15 ) ) ;
#25848 = CARTESIAN_POINT ( 'NONE',  ( 7.025853678916403666, 17.44829833425730925, -26.06988505166735237 ) ) ;
#25849 = ORIENTED_EDGE ( 'NONE', *, *, #609, .T. ) ;
#25850 = CARTESIAN_POINT ( 'NONE',  ( 10.37757302488624767, 41.72500000273119980, 31.93888565452638417 ) ) ;
#25851 = ORIENTED_EDGE ( 'NONE', *, *, #31876, .T. ) ;
#25852 = CARTESIAN_POINT ( 'NONE',  ( -15.01150461594642138, 39.64322916666667140, -26.00068869287340334 ) ) ;
#25853 = DIRECTION ( 'NONE',  ( -0.000000000000000000, -1.000000000000000000, -0.000000000000000000 ) ) ;
#25854 = CARTESIAN_POINT ( 'NONE',  ( 32.50000000000000000, 5.600000005462370645, -10.55989012756945833 ) ) ;
#25855 = TOROIDAL_SURFACE ( 'NONE', #23112, 11.45223628611452860, 4.000000000000014211 ) ;
#25856 = LINE ( 'NONE', #23804, #30428 ) ;
#25857 = CARTESIAN_POINT ( 'NONE',  ( -18.94512977948575738, 3.924999997268807661, -13.76444248337723231 ) ) ;
#25858 = CARTESIAN_POINT ( 'NONE',  ( 14.47279130897151767, 14.92499999726881299, -19.92008829642072598 ) ) ;
#25859 = CARTESIAN_POINT ( 'NONE',  ( -10.37757302488623701, 17.77500000273118985, 31.93888565452638417 ) ) ;
#25860 = CARTESIAN_POINT ( 'NONE',  ( -32.50000000000000000, 18.50000000546236834, 0.000000000000000000 ) ) ;
#25861 = CARTESIAN_POINT ( 'NONE',  ( -32.50000000000000000, 68.00000000000000000, 0.000000000000000000 ) ) ;
#25862 = CARTESIAN_POINT ( 'NONE',  ( -15.14183272437242067, 4.699999999999996625, -20.84094480462497856 ) ) ;
#25863 = DIRECTION ( 'NONE',  ( -0.000000000000000000, 1.000000000000000000, -0.000000000000000000 ) ) ;
#25864 = CARTESIAN_POINT ( 'NONE',  ( -7.468012846824771955, 61.84934000092397355, -28.02196122052045624 ) ) ;
#25865 = DIRECTION ( 'NONE',  ( 0.000000000000000000, 0.000000000000000000, -1.000000000000000000 ) ) ;
#25866 = CARTESIAN_POINT ( 'NONE',  ( -30.02300923189239867, 39.07031249999998579, 2.654126918244514854E-13 ) ) ;
#25867 = SHAPE_DEFINITION_REPRESENTATION ( #15378, #3268 ) ;
#25868 = DIRECTION ( 'NONE',  ( -0.000000000000000000, -1.000000000000000000, -0.000000000000000000 ) ) ;
#25869 = CARTESIAN_POINT ( 'NONE',  ( 18.94512977948576093, 17.32499999726880446, -13.76444248337722875 ) ) ;
#25870 = CARTESIAN_POINT ( 'NONE',  ( 32.50000000000000711, 10.90000000000000568, 10.55989012756945122 ) ) ;
#25871 = CARTESIAN_POINT ( 'NONE',  ( 13.94119854578893580, 49.09076416574269786, -24.22776226481265383 ) ) ;
#25872 = CARTESIAN_POINT ( 'NONE',  ( -33.58253175000000113, 53.22500000273118559, 10.91162601494193929 ) ) ;
#25873 = CARTESIAN_POINT ( 'NONE',  ( 10.37757302488624767, 61.97500000273119269, 31.93888565452638417 ) ) ;
#25874 = CARTESIAN_POINT ( 'NONE',  ( -10.37757302488624411, 38.97500000273118559, -31.93888565452638417 ) ) ;
#25875 = CARTESIAN_POINT ( 'NONE',  ( -1.778240108872766143E-15, 25.50000000000000711, -32.49999999999999289 ) ) ;
#25876 = CARTESIAN_POINT ( 'NONE',  ( 19.09188309203694800, 17.15624999999999645, 19.09188309203660694 ) ) ;
#25877 = CARTESIAN_POINT ( 'NONE',  ( 20.08610463437158344, 51.20000000546237118, 27.64615127144129403 ) ) ;
#25878 = CARTESIAN_POINT ( 'NONE',  ( -40.00000000000000711, 66.99999999999998579, -23.09401076758504345 ) ) ;
#25879 = CARTESIAN_POINT ( 'NONE',  ( 10.37757302488624056, 12.52500000273119873, -31.93888565452638417 ) ) ;
#25880 = PLANE ( 'NONE',  #10591 ) ;
#25881 = CARTESIAN_POINT ( 'NONE',  ( 0.000000000000000000, 82.00000000000001421, -15.00000000000000000 ) ) ;
#25882 = CARTESIAN_POINT ( 'NONE',  ( 7.313012447739250820E-14, 11.49999999999999112, 24.50000000000000000 ) ) ;
#25883 = CARTESIAN_POINT ( 'NONE',  ( -27.95245687107223986, 17.00743083240935860, 0.04044903255043252877 ) ) ;
#25884 = CARTESIAN_POINT ( 'NONE',  ( 26.29305231718578995, 37.70000000546237828, -19.10302069950538240 ) ) ;
#25885 = CARTESIAN_POINT ( 'NONE',  ( 0.000000000000000000, 80.00000000000001421, 0.000000000000000000 ) ) ;
#25886 = CARTESIAN_POINT ( 'NONE',  ( 10.37757302488624767, 27.72500000273120335, 31.93888565452638417 ) ) ;
#25887 = CARTESIAN_POINT ( 'NONE',  ( 13.97622843553633665, 48.23697916666665719, 24.20753774853730889 ) ) ;
#25888 = VERTEX_POINT ( 'NONE', #31607 ) ;
#25889 = CARTESIAN_POINT ( 'NONE',  ( -27.16883889988623935, 65.32500000273118701, 19.73931689729374739 ) ) ;
#25890 = CARTESIAN_POINT ( 'NONE',  ( 15.01150461594643204, 48.23697916666665719, 26.00068869287340334 ) ) ;
#25891 = VERTEX_POINT ( 'NONE', #8105 ) ;
#25892 = CARTESIAN_POINT ( 'NONE',  ( 25.98046417659858420, 63.13840250092397355, 15.04653450569292872 ) ) ;
#25893 = CARTESIAN_POINT ( 'NONE',  ( 13.94119854578937812, 59.98736083425730925, 24.22776226481240514 ) ) ;
#25894 = AXIS2_PLACEMENT_3D ( 'NONE', #22128, #9071, #22798 ) ;
#25895 = VECTOR ( 'NONE', #27398, 1000.000000000000000 ) ;
#25896 = ORIENTED_EDGE ( 'NONE', *, *, #15609, .F. ) ;
#25897 = CARTESIAN_POINT ( 'NONE',  ( -33.58253175000000113, 9.025000002731184523, -10.91162601494193218 ) ) ;
#25898 = AXIS2_PLACEMENT_3D ( 'NONE', #13762, #11189, #3459 ) ;
#25899 = CARTESIAN_POINT ( 'NONE',  ( 26.02091320914876960, 19.01263916574269075, 14.97647472619900455 ) ) ;
#25900 = DIRECTION ( 'NONE',  ( -0.000000000000000000, -1.000000000000000000, -0.000000000000000000 ) ) ;
#25901 = CARTESIAN_POINT ( 'NONE',  ( 27.16883889988623935, 34.57500000273120122, -19.73931689729374384 ) ) ;
#25902 = CARTESIAN_POINT ( 'NONE',  ( 10.04305231718578817, 37.90000000546236691, -30.90933677959249337 ) ) ;
#25903 = CARTESIAN_POINT ( 'NONE',  ( -15.00000000000000000, 75.89999999999996305, -4.873795443493594171 ) ) ;
#25904 = CARTESIAN_POINT ( 'NONE',  ( -15.01150461594595775, 65.99739583333334281, 26.00068869287368756 ) ) ;
#25905 = CARTESIAN_POINT ( 'NONE',  ( -33.58253175000000113, 21.22500000273117848, 10.91162601494193929 ) ) ;
#25906 = CARTESIAN_POINT ( 'NONE',  ( -4.405589869732278832E-13, 31.00000000546236834, 32.50000000000000000 ) ) ;
#25907 = CARTESIAN_POINT ( 'NONE',  ( 33.58253175000000113, 48.47500000273118559, -10.91162601494193751 ) ) ;
#25908 =( NAMED_UNIT ( * ) SI_UNIT ( $, .STERADIAN. ) SOLID_ANGLE_UNIT ( ) );
#25909 = CARTESIAN_POINT ( 'NONE',  ( 32.50000000000000000, 29.00000000000001066, -3.980102097228898626E-15 ) ) ;
#25910 = CARTESIAN_POINT ( 'NONE',  ( 20.08610463437157279, 27.29999999999997939, -27.64615127144129758 ) ) ;
#25911 = CARTESIAN_POINT ( 'NONE',  ( -7.570916362186210335, 4.599999999999992539, -23.30088464923126779 ) ) ;
#25912 =( BOUNDED_CURVE ( )  B_SPLINE_CURVE ( 2, ( #5784, #19332, #620, #3874, #24476, #3217, #21748, #29776, #950, #21578, #789, #456, #14013 ),
 .UNSPECIFIED., .F., .F. ) 
 B_SPLINE_CURVE_WITH_KNOTS ( ( 3, 2, 2, 2, 2, 2, 3 ),
 ( 0.3012820512820512664, 0.3025641025641025439, 0.3051282051282051544, 0.3076923076923077094, 0.3102564102564102644, 0.3128205128205128194, 0.3141025641025640969 ),
 .UNSPECIFIED. ) 
 CURVE ( )  GEOMETRIC_REPRESENTATION_ITEM ( )  RATIONAL_B_SPLINE_CURVE ( ( 0.9755282581475768211, 0.9755282581475768211, 1.000000000000000000, 0.9510565162951535312, 1.000000000000000000, 0.9510565162951535312, 1.000000000000000000, 0.9510565162951535312, 1.000000000000000000, 0.9510565162951535312, 1.000000000000000000, 0.9755282581475768211, 0.9755282581475768211 ) ) 
 REPRESENTATION_ITEM ( '' )  );
#25913 = CARTESIAN_POINT ( 'NONE',  ( -20.75514604977248823, 68.82500000273118701, -28.56700777964554305 ) ) ;
#25914 = CARTESIAN_POINT ( 'NONE',  ( -26.29305231718579350, 77.80000000000001137, -19.10302069950537884 ) ) ;
#25915 = CARTESIAN_POINT ( 'NONE',  ( -20.08610463437157989, 20.20000000546238539, -27.64615127144129758 ) ) ;
#25916 = CARTESIAN_POINT ( 'NONE',  ( 10.37757302488624767, 57.97500000273119980, 31.93888565452638417 ) ) ;
#25917 = CYLINDRICAL_SURFACE ( 'NONE', #25432, 24.50000000000000000 ) ;
#25918 = CARTESIAN_POINT ( 'NONE',  ( 27.16883889988623935, 10.32500000273117635, -19.73931689729374384 ) ) ;
#25919 = CARTESIAN_POINT ( 'NONE',  ( -24.18731323226248264, 30.48215250092397710, -14.01125832528284931 ) ) ;
#25920 = CARTESIAN_POINT ( 'NONE',  ( 29.41736854754607222, 66.99999999999997158, -14.41477566699509083 ) ) ;
#25921 = VECTOR ( 'NONE', #333, 1000.000000000000000 ) ;
#25922 = CARTESIAN_POINT ( 'NONE',  ( -33.58253175000000113, 35.02500000273118275, -10.91162601494193218 ) ) ;
#25923 = CARTESIAN_POINT ( 'NONE',  ( 0.000000000000000000, 80.00000000000001421, -32.50000000000000000 ) ) ;
#25924 = AXIS2_PLACEMENT_3D ( 'NONE', #31429, #20814, #25944 ) ;
#25925 = CARTESIAN_POINT ( 'NONE',  ( -13.91746824999999532, 74.77500000273120406, -4.522059556121115875 ) ) ;
#25926 = CARTESIAN_POINT ( 'NONE',  ( 20.47846945139867003, 45.79649333240935505, -20.53372385742107653 ) ) ;
#25927 = CARTESIAN_POINT ( 'NONE',  ( -26.29305231718578995, 52.70000000546236407, 19.10302069950538595 ) ) ;
#25928 = CARTESIAN_POINT ( 'NONE',  ( 4.300734207923761154, 77.97500000273122112, 13.23629886949340495 ) ) ;
#25929 = CARTESIAN_POINT ( 'NONE',  ( 1.836970198721029589E-15, 82.00000000000001421, 15.00000000000000000 ) ) ;
#25930 = CARTESIAN_POINT ( 'NONE',  ( -27.95245687107222921, 15.00781249999999467, 2.498001805406602216E-13 ) ) ;
#25931 = CARTESIAN_POINT ( 'NONE',  ( -20.08610463437157989, 53.69999999999998863, -27.64615127144129758 ) ) ;
#25932 = CARTESIAN_POINT ( 'NONE',  ( -32.50000000000000000, 78.40000000546233139, -10.55989012756945478 ) ) ;
#25933 = CARTESIAN_POINT ( 'NONE',  ( 7.505752307973351023, 17.44270833333333215, 28.01184896238290278 ) ) ;
#25934 = EDGE_CURVE ( 'NONE', #7233, #5684, #30338, .T. ) ;
#25935 = CARTESIAN_POINT ( 'NONE',  ( -27.16883889988623935, 35.57500000273118701, 19.73931689729374739 ) ) ;
#25936 = CARTESIAN_POINT ( 'NONE',  ( 7.236395654485755280, 6.724999997268804819, 22.27133577429736988 ) ) ;
#25937 = ORIENTED_EDGE ( 'NONE', *, *, #31468, .T. ) ;
#25938 = CARTESIAN_POINT ( 'NONE',  ( -27.16883889988624290, 75.17500000273119554, -19.73931689729374028 ) ) ;
#25939 = CARTESIAN_POINT ( 'NONE',  ( -2.092463501923844636E-15, 22.00000000546238965, -34.17252228774368916 ) ) ;
#25940 = CARTESIAN_POINT ( 'NONE',  ( 26.00068869287340334, 43.94010416666665719, -15.01150461594642316 ) ) ;
#25941 = CARTESIAN_POINT ( 'NONE',  ( 30.02300923189239512, 61.41406250000000711, -2.619432448724977703E-13 ) ) ;
#25942 = CARTESIAN_POINT ( 'NONE',  ( -10.37757302488623701, 55.77500000273119696, 31.93888565452638417 ) ) ;
#25943 = CARTESIAN_POINT ( 'NONE',  ( -26.29305231718578995, 56.70000000546237828, 19.10302069950538595 ) ) ;
#25944 = DIRECTION ( 'NONE',  ( 0.000000000000000000, 0.000000000000000000, 1.000000000000000000 ) ) ;
#25945 = CARTESIAN_POINT ( 'NONE',  ( 10.37757302488624056, 40.52500000273118275, -31.93888565452638417 ) ) ;
#25946 = FACE_OUTER_BOUND ( 'NONE', #31874, .T. ) ;
#25947 = CARTESIAN_POINT ( 'NONE',  ( 27.16883889988623935, 68.57500000273120122, -19.73931689729374384 ) ) ;
#25948 = CARTESIAN_POINT ( 'NONE',  ( 32.50000000000000000, 3.500000005462383434, -3.980102097228898626E-15 ) ) ;
#25949 = AXIS2_PLACEMENT_3D ( 'NONE', #22930, #7651, #2508 ) ;
#25950 = CARTESIAN_POINT ( 'NONE',  ( -20.75514604977248112, 59.42500000273118843, 28.56700777964554661 ) ) ;
#25951 = ADVANCED_FACE ( 'NONE', ( #31773, #28700 ), #28868, .T. ) ;
#25952 = CARTESIAN_POINT ( 'NONE',  ( 0.000000000000000000, 80.00000000000001421, 0.000000000000000000 ) ) ;
#25953 = CARTESIAN_POINT ( 'NONE',  ( -32.50000000000000000, 47.89999999999999858, -10.55989012756945478 ) ) ;
#25954 = DIRECTION ( 'NONE',  ( -1.224646799147353207E-16, -1.499759782661857882E-32, 1.000000000000000000 ) ) ;
#25955 = CARTESIAN_POINT ( 'NONE',  ( -33.58253175000000113, 13.47500000273118914, 10.91162601494193929 ) ) ;
#25956 = CARTESIAN_POINT ( 'NONE',  ( 0.04044903255044120238, 29.89805583240935860, 27.95245687107223276 ) ) ;
#25957 = CARTESIAN_POINT ( 'NONE',  ( -8.601468415847515203, 77.67500000273119554, 11.83890561707634959 ) ) ;
#25958 = CARTESIAN_POINT ( 'NONE',  ( 33.58253175000000113, 76.47500000273117848, -10.91162601494193574 ) ) ;
#25959 = LINE ( 'NONE', #10683, #33080 ) ;
#25960 = CARTESIAN_POINT ( 'NONE',  ( 27.16883889988624290, 76.17500000273118133, 19.73931689729373673 ) ) ;
#25961 = VERTEX_POINT ( 'NONE', #20995 ) ;
#25962 = CARTESIAN_POINT ( 'NONE',  ( 7.236395654485760609, 15.52499999726880731, -22.27133577429736633 ) ) ;
#25963 = CARTESIAN_POINT ( 'NONE',  ( 14.47279130897151944, 4.924999997268811214, -19.92008829642072598 ) ) ;
#25964 = CARTESIAN_POINT ( 'NONE',  ( -19.09188309203694445, 56.68749999999998579, -19.09188309203661049 ) ) ;
#25965 = CARTESIAN_POINT ( 'NONE',  ( 33.58253175000000113, 54.22500000273117848, -10.91162601494193751 ) ) ;
#25966 = CARTESIAN_POINT ( 'NONE',  ( -10.37757302488624411, 18.97500000273118204, -31.93888565452638417 ) ) ;
#25967 = CARTESIAN_POINT ( 'NONE',  ( 10.37757302488624056, 6.775000002731193405, -31.93888565452638417 ) ) ;
#25968 = CARTESIAN_POINT ( 'NONE',  ( 13.97622843553633842, 44.79947916666667140, 24.20753774853730889 ) ) ;
#25969 = UNCERTAINTY_MEASURE_WITH_UNIT (LENGTH_MEASURE( 1.000000000000000082E-05 ), #31394, 'distance_accuracy_value', 'NONE');
#25970 = CARTESIAN_POINT ( 'NONE',  ( 15.04653450569292872, 17.59152750092397355, -25.98046417659857710 ) ) ;
#25971 = CARTESIAN_POINT ( 'NONE',  ( -20.47846945139866648, 16.57774333240934794, 20.53372385742108008 ) ) ;
#25972 = CARTESIAN_POINT ( 'NONE',  ( -10.04305231718579172, 78.10000000546239107, -30.90933677959248982 ) ) ;
#25973 = CARTESIAN_POINT ( 'NONE',  ( 29.99227890624914039, 52.00000000000002132, -14.07346378240328910 ) ) ;
#25974 = AXIS2_PLACEMENT_3D ( 'NONE', #9393, #2714, #10272 ) ;
#25975 = CARTESIAN_POINT ( 'NONE',  ( 27.16883889988624290, 43.92500000273119554, 19.73931689729373673 ) ) ;
#25976 = CIRCLE ( 'NONE', #24336, 1.500000000000008216 ) ;
#25977 = CARTESIAN_POINT ( 'NONE',  ( 18.94512977948575738, 6.424999997268809437, 13.76444248337723408 ) ) ;
#25978 = DIRECTION ( 'NONE',  ( 1.000000000000000000, 1.416100796715761110E-16, 0.000000000000000000 ) ) ;
#25979 = EDGE_LOOP ( 'NONE', ( #9204, #21680, #10211, #9660, #25684, #29012, #29135, #18317, #15617, #31130, #2472, #21641, #14287, #17897 ) ) ;
#25980 = CARTESIAN_POINT ( 'NONE',  ( 33.58253175000000823, 54.27500000273118275, 10.91162601494192863 ) ) ;
#25981 = CARTESIAN_POINT ( 'NONE',  ( -3.712076227271900841E-14, 10.24999999453763344, -24.50000000000000000 ) ) ;
#25982 = CARTESIAN_POINT ( 'NONE',  ( 27.95245687107223986, 38.78944416759064495, 0.04044903254993640479 ) ) ;
#25983 = CARTESIAN_POINT ( 'NONE',  ( -10.37757302488623701, 73.77500000273118985, 31.93888565452638417 ) ) ;
#25984 = EDGE_LOOP ( 'NONE', ( #19062, #27114, #31775, #10543 ) ) ;
#25985 = CARTESIAN_POINT ( 'NONE',  ( 27.16883889988623935, 24.32500000273117635, -19.73931689729374384 ) ) ;
#25986 = CARTESIAN_POINT ( 'NONE',  ( -15.01150461594595775, 17.87239583333332149, 26.00068869287368756 ) ) ;
#25987 = VERTEX_POINT ( 'NONE', #23564 ) ;
#25988 = CARTESIAN_POINT ( 'NONE',  ( -32.50000000000000000, 14.50000000546236478, 0.000000000000000000 ) ) ;
#25989 = CARTESIAN_POINT ( 'NONE',  ( -33.58253175000000113, 59.02500000273120406, -10.91162601494193218 ) ) ;
#25990 = CARTESIAN_POINT ( 'NONE',  ( -20.50609665441004736, 39.49999999999999289, -20.50609665440969565 ) ) ;
#25991 = CARTESIAN_POINT ( 'NONE',  ( -15.14183272437242067, 6.449999994537612302, -20.84094480462497856 ) ) ;
#25992 = CARTESIAN_POINT ( 'NONE',  ( -18.94512977948576093, 2.324999997268817342, 13.76444248337722698 ) ) ;
#25993 = CARTESIAN_POINT ( 'NONE',  ( -10.37757302488624411, 6.725000002731185589, -31.93888565452638417 ) ) ;
#25994 = FACE_OUTER_BOUND ( 'NONE', #21510, .T. ) ;
#25995 = CARTESIAN_POINT ( 'NONE',  ( -25.98046417659831420, 61.40847249907603356, 15.04653450569339945 ) ) ;
#25996 = CARTESIAN_POINT ( 'NONE',  ( -7.570916362186210335, 14.60000000000000142, -23.30088464923126779 ) ) ;
#25997 = CYLINDRICAL_SURFACE ( 'NONE', #19894, 32.50000000000000000 ) ;
#25998 = CARTESIAN_POINT ( 'NONE',  ( 2.445080149700053643E-15, 74.50000000000000000, 15.00000000000000000 ) ) ;
#25999 = CARTESIAN_POINT ( 'NONE',  ( -10.04305231718578462, 18.40000000000001279, 30.90933677959249337 ) ) ;
#26000 = CARTESIAN_POINT ( 'NONE',  ( 19.09188309203661049, 60.98437499999999289, -19.09188309203694445 ) ) ;
#26001 = CARTESIAN_POINT ( 'NONE',  ( -19.82091636218621034, 10.54999999453762349, -14.40073868116559552 ) ) ;
#26002 = CARTESIAN_POINT ( 'NONE',  ( -4.635254915624208216, 72.65000000546240244, 14.26584774442730463 ) ) ;
#26003 = CARTESIAN_POINT ( 'NONE',  ( -6.988114217768288228, 26.03645833333333215, -26.07999730980477437 ) ) ;
#26004 = ADVANCED_FACE ( 'NONE', ( #33856 ), #7767, .T. ) ;
#26005 = CARTESIAN_POINT ( 'NONE',  ( -27.16883889988623935, 33.32500000273120122, 19.73931689729374739 ) ) ;
#26006 = CARTESIAN_POINT ( 'NONE',  ( -20.75514604977248823, 76.82500000273120122, -28.56700777964554305 ) ) ;
#26007 = CARTESIAN_POINT ( 'NONE',  ( -33.58253175000000113, 39.47500000273117848, 10.91162601494193929 ) ) ;
#26008 = CARTESIAN_POINT ( 'NONE',  ( 33.58253175000000823, 20.27500000273117564, 10.91162601494192685 ) ) ;
#26009 = CARTESIAN_POINT ( 'NONE',  ( 3.445340210940985210E-14, 7.249999994537622783, 24.50000000000000000 ) ) ;
#26010 = ADVANCED_FACE ( 'NONE', ( #15505 ), #5365, .T. ) ;
#26011 = CARTESIAN_POINT ( 'NONE',  ( -19.06425588902591173, 47.81288166759064495, -19.11951029504763611 ) ) ;
#26012 = CARTESIAN_POINT ( 'NONE',  ( 33.58253175000000823, 76.02500000273118985, 10.91162601494192685 ) ) ;
#26013 = CYLINDRICAL_SURFACE ( 'NONE', #8606, 9.000000000000001776 ) ;
#26014 = CARTESIAN_POINT ( 'NONE',  ( -32.50000000000000000, 60.09999999999999432, 10.55989012756946366 ) ) ;
#26015 = CARTESIAN_POINT ( 'NONE',  ( -4.523095164977117273E-15, 18.12499999726880162, 24.62258325217400312 ) ) ;
#26016 = CARTESIAN_POINT ( 'NONE',  ( 33.58253175000000113, 66.22500000273120691, -10.91162601494193574 ) ) ;
#26017 =( BOUNDED_CURVE ( )  B_SPLINE_CURVE ( 2, ( #3357, #929, #24296, #29090, #11249, #8664, #3520, #18983, #26698, #24128, #5594, #3195, #23962 ),
 .UNSPECIFIED., .F., .F. ) 
 B_SPLINE_CURVE_WITH_KNOTS ( ( 3, 2, 2, 2, 2, 2, 3 ),
 ( 0.8141025641025640969, 0.8153846153846153744, 0.8179487179487179294, 0.8205128205128204844, 0.8230769230769230393, 0.8256410256410255943, 0.8269230769230769829 ),
 .UNSPECIFIED. ) 
 CURVE ( )  GEOMETRIC_REPRESENTATION_ITEM ( )  RATIONAL_B_SPLINE_CURVE ( ( 0.9755282581475768211, 0.9755282581475768211, 1.000000000000000000, 0.9510565162951535312, 1.000000000000000000, 0.9510565162951535312, 1.000000000000000000, 0.9510565162951535312, 1.000000000000000000, 0.9510565162951535312, 1.000000000000000000, 0.9755282581475757109, 0.9755282581475768211 ) ) 
 REPRESENTATION_ITEM ( '' )  );
#26018 = CARTESIAN_POINT ( 'NONE',  ( 18.94512977948575738, 10.92499999726881299, 13.76444248337723408 ) ) ;
#26019 = AXIS2_PLACEMENT_3D ( 'NONE', #9912, #4590, #22440 ) ;
#26020 = CARTESIAN_POINT ( 'NONE',  ( -33.58253175000000113, 73.27500000273118985, -10.91162601494193218 ) ) ;
#26021 =( BOUNDED_CURVE ( )  B_SPLINE_CURVE ( 2, ( #20820, #2096, #5014, #4330, #20130, #23215, #1919, #14803, #33675, #30574, #25268, #12569, #22694, #10173, #33849, #20299, #23040, #20656, #14975, #10001, #31264, #10344, #7759, #27846, #1741, #25444, #12221, #12396, #22867, #33324, #30749, #17727, #28184, #33498, #25615, #28860, #3125, #21486, #24063, #31599, #31933, #15837, #8426, #16007, #26122, #21156, #32559, #18245, #23892, #23722, #18584, #13082, #28692, #6320, #15673, #13597, #18915, #20986, #8258, #29024, #18750, #31765, #529, #29192, #26462, #2954, #10676, #29817, #2619, #5527, #5190, #23556, #5357, #26294, #13424, #22115, #363, #8097, #16175, #10849, #20, #11016, #5698, #21324, #26631, #16796, #27254, #10508, #11631, #31436, #7928, #18414, #3746, #2783, #13249, #14219, #24676, #1149, #189, #22607, #14722, #11968, #22956, #15066, #25182, #1660, #7158, #19867, #33061, #12312, #12135, #11802, #25534, #22439, #17641, #9219, #22784, #6990, #24841, #28102, #9735, #22280, #19703, #9565, #12487, #27760, #30321, #27933, #32886, #20044, #3913, #4417, #25012, #14894, #14382, #30149, #9385, #1319, #1494, #29986, #6491, #25355, #6818, #30489, #32723, #1834, #17299, #33236, #6652, #17133, #4248, #27589, #17473, #16964, #27422, #9058, #4589, #20221, #30661, #2011, #19538, #4078, #14553, #31351, #7509, #9911, #10425, #25699, #20388, #18161, #28273, #20903, #28946, #15411, #28603, #4759, #18502, #10260, #106, #28439, #31012, #2705, #30839, #33769, #10088, #13165, #4930, #15236, #2180, #25866, #12653, #26039, #2533, #10597, #23642, #23123, #7844, #2355, #17993, #5444, #13001, #21074, #12830, #17815, #23472, #33587, #23302, #18333, #20567, #5102, #15925, #20742, #8017, #7331, #15588, #5275, #31184, #31523, #15757, #7675, #28778, #33934, #26211, #26381, #2872, #13341, #33414, #948, #24147, #18671, #21903, #21745, #29110, #617, #5950, #3377, #32021, #32355, #16429, #32191, #26719, #10767, #8346, #11106, #11269, #18835, #3215, #31854, #8517, #26549, #14011, #5614, #23980, #19003, #8849, #19169, #29447, #16262, #26881, #451, #787, #10933, #13847, #27215, #24313, #21575, #16098, #8685, #19330, #5782, #29607, #3045, #29773, #6109, #24473, #29281, #21408, #27045, #16589, #31687, #13683, #3539, #11428, #13517, #6280, #16756, #3706, #23814, #279, #21244, #8181, #3871, #22565, #9179, #22239, #20176, #27720, #33016, #4208, #11931, #22401, #27382, #4036, #1617, #16922, #9341, #9696, #14344, #22742, #22072, #19826, #20003, #29946, #12267, #30450, #6450, #9522, #14680, #32849, #12095, #30278, #19498, #11758, #25316, #14511, #9016, #33193, #6948, #24801, #24970, #6779, #25141, #17258, #30620, #17431, #27892, #17090, #28060, #7116, #4376, #14850, #19663, #27549, #32684, #1789, #1278, #17598, #30106, #6612, #14178, #24635, #1108, #11593, #1452, #32516, #4717, #15545, #13125, #7635, #18117, #21033, #25826, #23433, #28401, #20702, #33372, #33893, #20527, #10385, #9868, #25661, #4890, #20345, #30970, #25492, #1971, #4547, #23600, #10223, #26172, #15717, #7803, #15023, #30795, #2490 ),
 .UNSPECIFIED., .F., .T. ) 
 B_SPLINE_CURVE_WITH_KNOTS ( ( 3, 2, 2, 2, 2, 2, 2, 2, 2, 2, 2, 2, 2, 2, 2, 2, 2, 2, 2, 2, 2, 2, 2, 2, 2, 2, 2, 2, 2, 2, 2, 2, 2, 2, 2, 2, 2, 2, 2, 2, 2, 2, 2, 2, 2, 2, 2, 2, 2, 2, 2, 2, 2, 2, 2, 2, 2, 2, 2, 2, 2, 2, 2, 2, 2, 2, 2, 2, 2, 2, 2, 2, 2, 2, 2, 2, 2, 2, 2, 2, 2, 2, 2, 2, 2, 2, 2, 2, 2, 2, 2, 2, 2, 2, 2, 2, 2, 2, 2, 2, 2, 2, 2, 2, 2, 2, 2, 2, 2, 2, 2, 2, 2, 2, 2, 2, 2, 2, 2, 2, 2, 2, 2, 2, 2, 2, 2, 2, 2, 2, 2, 2, 2, 2, 2, 2, 2, 2, 2, 2, 2, 2, 2, 2, 2, 2, 2, 2, 2, 2, 2, 2, 2, 2, 2, 2, 2, 2, 2, 2, 2, 2, 2, 2, 2, 2, 2, 2, 2, 2, 2, 2, 2, 2, 2, 2, 2, 2, 2, 2, 2, 2, 2, 2, 2, 2, 2, 2, 2, 2, 2, 2, 3 ),
 ( 0.000000000000000000, 0.005208333333333333044, 0.01041666666666666609, 0.01562500000000000000, 0.02083333333333333218, 0.02604166666666666782, 0.03125000000000000000, 0.03645833333333333565, 0.04166666666666666435, 0.04687500000000000000, 0.05208333333333333565, 0.05729166666666666435, 0.06250000000000000000, 0.06770833333333332871, 0.07291666666666667129, 0.07812500000000000000, 0.08333333333333332871, 0.08854166666666667129, 0.09375000000000000000, 0.09895833333333332871, 0.1041666666666666713, 0.1093750000000000000, 0.1145833333333333287, 0.1197916666666666713, 0.1250000000000000000, 0.1302083333333333426, 0.1354166666666666574, 0.1406250000000000000, 0.1458333333333333426, 0.1510416666666666574, 0.1562500000000000000, 0.1614583333333333426, 0.1666666666666666574, 0.1718750000000000000, 0.1770833333333333426, 0.1822916666666666574, 0.1875000000000000000, 0.1927083333333333426, 0.1979166666666666574, 0.2031250000000000000, 0.2083333333333333426, 0.2135416666666666574, 0.2187500000000000000, 0.2239583333333333426, 0.2291666666666666574, 0.2343750000000000000, 0.2395833333333333426, 0.2447916666666666574, 0.2500000000000000000, 0.2552083333333333148, 0.2604166666666666852, 0.2656250000000000000, 0.2708333333333333148, 0.2760416666666666852, 0.2812500000000000000, 0.2864583333333333148, 0.2916666666666666852, 0.2968750000000000000, 0.3020833333333333148, 0.3072916666666666852, 0.3125000000000000000, 0.3177083333333333148, 0.3229166666666666852, 0.3281250000000000000, 0.3333333333333333148, 0.3385416666666666852, 0.3437500000000000000, 0.3489583333333333148, 0.3541666666666666852, 0.3593750000000000000, 0.3645833333333333148, 0.3697916666666666852, 0.3750000000000000000, 0.3802083333333333148, 0.3854166666666666852, 0.3906250000000000000, 0.3958333333333333148, 0.4010416666666666852, 0.4062500000000000000, 0.4114583333333333148, 0.4166666666666666852, 0.4218750000000000000, 0.4270833333333333148, 0.4322916666666666852, 0.4375000000000000000, 0.4427083333333333148, 0.4479166666666666852, 0.4531250000000000000, 0.4583333333333333148, 0.4635416666666666852, 0.4687500000000000000, 0.4739583333333333148, 0.4791666666666666852, 0.4843750000000000000, 0.4895833333333333148, 0.4947916666666666852, 0.5000000000000000000, 0.5052083333333333703, 0.5104166666666666297, 0.5156250000000000000, 0.5208333333333333703, 0.5260416666666666297, 0.5312500000000000000, 0.5364583333333333703, 0.5416666666666666297, 0.5468750000000000000, 0.5520833333333333703, 0.5572916666666666297, 0.5625000000000000000, 0.5677083333333333703, 0.5729166666666666297, 0.5781250000000000000, 0.5833333333333333703, 0.5885416666666666297, 0.5937500000000000000, 0.5989583333333333703, 0.6041666666666666297, 0.6093750000000000000, 0.6145833333333333703, 0.6197916666666666297, 0.6250000000000000000, 0.6302083333333333703, 0.6354166666666666297, 0.6406250000000000000, 0.6458333333333333703, 0.6510416666666666297, 0.6562500000000000000, 0.6614583333333333703, 0.6666666666666666297, 0.6718750000000000000, 0.6770833333333333703, 0.6822916666666666297, 0.6875000000000000000, 0.6927083333333333703, 0.6979166666666666297, 0.7031250000000000000, 0.7083333333333333703, 0.7135416666666666297, 0.7187500000000000000, 0.7239583333333333703, 0.7291666666666666297, 0.7343750000000000000, 0.7395833333333333703, 0.7447916666666666297, 0.7500000000000000000, 0.7552083333333333703, 0.7604166666666666297, 0.7656250000000000000, 0.7708333333333333703, 0.7760416666666666297, 0.7812500000000000000, 0.7864583333333333703, 0.7916666666666666297, 0.7968750000000000000, 0.8020833333333333703, 0.8072916666666666297, 0.8125000000000000000, 0.8177083333333333703, 0.8229166666666666297, 0.8281250000000000000, 0.8333333333333333703, 0.8385416666666666297, 0.8437500000000000000, 0.8489583333333333703, 0.8541666666666666297, 0.8593750000000000000, 0.8645833333333333703, 0.8697916666666666297, 0.8750000000000000000, 0.8802083333333333703, 0.8854166666666666297, 0.8906250000000000000, 0.8958333333333333703, 0.9010416666666666297, 0.9062500000000000000, 0.9114583333333333703, 0.9166666666666666297, 0.9218750000000000000, 0.9270833333333333703, 0.9322916666666666297, 0.9375000000000000000, 0.9427083333333333703, 0.9479166666666666297, 0.9531250000000000000, 0.9583333333333333703, 0.9635416666666666297, 0.9687500000000000000, 0.9739583333333333703, 0.9791666666666666297, 0.9843750000000000000, 0.9895833333333333703, 0.9947916666666666297, 1.000000000000000000 ),
 .UNSPECIFIED. ) 
 CURVE ( )  GEOMETRIC_REPRESENTATION_ITEM ( )  RATIONAL_B_SPLINE_CURVE ( ( 1.000000000000000000, 0.9659258262890683122, 1.000000000000000000, 0.9659258262890683122, 1.000000000000000000, 0.9659258262890683122, 1.000000000000000000, 0.9659258262890683122, 1.000000000000000000, 0.9659258262890683122, 1.000000000000000000, 0.9659258262890683122, 1.000000000000000000, 0.9659258262890683122, 1.000000000000000000, 0.9659258262890683122, 1.000000000000000000, 0.9659258262890683122, 1.000000000000000000, 0.9659258262890683122, 1.000000000000000000, 0.9659258262890683122, 1.000000000000000000, 0.9659258262890683122, 1.000000000000000000, 0.9659258262890683122, 1.000000000000000000, 0.9659258262890683122, 1.000000000000000000, 0.9659258262890683122, 1.000000000000000000, 0.9659258262890683122, 1.000000000000000000, 0.9659258262890683122, 1.000000000000000000, 0.9659258262890683122, 1.000000000000000000, 0.9659258262890683122, 1.000000000000000000, 0.9659258262890683122, 1.000000000000000000, 0.9659258262890683122, 1.000000000000000000, 0.9659258262890683122, 1.000000000000000000, 0.9659258262890683122, 1.000000000000000000, 0.9659258262890683122, 1.000000000000000000, 0.9659258262890683122, 1.000000000000000000, 0.9659258262890683122, 1.000000000000000000, 0.9659258262890683122, 1.000000000000000000, 0.9659258262890683122, 1.000000000000000000, 0.9659258262890683122, 1.000000000000000000, 0.9659258262890683122, 1.000000000000000000, 0.9659258262890683122, 1.000000000000000000, 0.9659258262890683122, 1.000000000000000000, 0.9659258262890683122, 1.000000000000000000, 0.9659258262890683122, 1.000000000000000000, 0.9659258262890683122, 1.000000000000000000, 0.9659258262890683122, 1.000000000000000000, 0.9659258262890683122, 1.000000000000000000, 0.9659258262890683122, 1.000000000000000000, 0.9659258262890683122, 1.000000000000000000, 0.9659258262890683122, 1.000000000000000000, 0.9659258262890683122, 1.000000000000000000, 0.9659258262890683122, 1.000000000000000000, 0.9659258262890683122, 1.000000000000000000, 0.9659258262890683122, 1.000000000000000000, 0.9659258262890683122, 1.000000000000000000, 0.9659258262890683122, 1.000000000000000000, 0.9659258262890683122, 1.000000000000000000, 0.9659258262890683122, 1.000000000000000000, 0.9659258262890683122, 1.000000000000000000, 0.9659258262890683122, 1.000000000000000000, 0.9659258262890683122, 1.000000000000000000, 0.9659258262890683122, 1.000000000000000000, 0.9659258262890683122, 1.000000000000000000, 0.9659258262890683122, 1.000000000000000000, 0.9659258262890683122, 1.000000000000000000, 0.9659258262890683122, 1.000000000000000000, 0.9659258262890683122, 1.000000000000000000, 0.9659258262890683122, 1.000000000000000000, 0.9659258262890683122, 1.000000000000000000, 0.9659258262890683122, 1.000000000000000000, 0.9659258262890683122, 1.000000000000000000, 0.9659258262890683122, 1.000000000000000000, 0.9659258262890683122, 1.000000000000000000, 0.9659258262890683122, 1.000000000000000000, 0.9659258262890683122, 1.000000000000000000, 0.9659258262890683122, 1.000000000000000000, 0.9659258262890683122, 1.000000000000000000, 0.9659258262890683122, 1.000000000000000000, 0.9659258262890683122, 1.000000000000000000, 0.9659258262890683122, 1.000000000000000000, 0.9659258262890683122, 1.000000000000000000, 0.9659258262890683122, 1.000000000000000000, 0.9659258262890683122, 1.000000000000000000, 0.9659258262890683122, 1.000000000000000000, 0.9659258262890683122, 1.000000000000000000, 0.9659258262890683122, 1.000000000000000000, 0.9659258262890683122, 1.000000000000000000, 0.9659258262890683122, 1.000000000000000000, 0.9659258262890683122, 1.000000000000000000, 0.9659258262890683122, 1.000000000000000000, 0.9659258262890683122, 1.000000000000000000, 0.9659258262890683122, 1.000000000000000000, 0.9659258262890683122, 1.000000000000000000, 0.9659258262890683122, 1.000000000000000000, 0.9659258262890683122, 1.000000000000000000, 0.9659258262890683122, 1.000000000000000000, 0.9659258262890683122, 1.000000000000000000, 0.9659258262890683122, 1.000000000000000000, 0.9659258262890683122, 1.000000000000000000, 0.9659258262890683122, 1.000000000000000000, 0.9659258262890683122, 1.000000000000000000, 0.9659258262890683122, 1.000000000000000000, 0.9659258262890683122, 1.000000000000000000, 0.9659258262890683122, 1.000000000000000000, 0.9659258262890683122, 1.000000000000000000, 0.9659258262890683122, 1.000000000000000000, 0.9659258262890683122, 1.000000000000000000, 0.9659258262890683122, 1.000000000000000000, 0.9659258262890683122, 1.000000000000000000, 0.9659258262890683122, 1.000000000000000000, 0.9659258262890683122, 1.000000000000000000, 0.9659258262890683122, 1.000000000000000000, 0.9659258262890683122, 1.000000000000000000, 0.9659258262890683122, 1.000000000000000000, 0.9659258262890683122, 1.000000000000000000, 0.9659258262890683122, 1.000000000000000000, 0.9659258262890683122, 1.000000000000000000, 0.9659258262890683122, 1.000000000000000000, 0.9659258262890683122, 1.000000000000000000, 0.9659258262890683122, 1.000000000000000000, 0.9659258262890683122, 1.000000000000000000, 0.9659258262890683122, 1.000000000000000000, 0.9659258262890683122, 1.000000000000000000, 0.9659258262890683122, 1.000000000000000000, 0.9659258262890683122, 1.000000000000000000, 0.9659258262890683122, 1.000000000000000000, 0.9659258262890683122, 1.000000000000000000, 0.9659258262890683122, 1.000000000000000000, 0.9659258262890683122, 1.000000000000000000, 0.9659258262890683122, 1.000000000000000000, 0.9659258262890683122, 1.000000000000000000, 0.9659258262890683122, 1.000000000000000000, 0.9659258262890683122, 1.000000000000000000, 0.9659258262890683122, 1.000000000000000000, 0.9659258262890683122, 1.000000000000000000, 0.9659258262890683122, 1.000000000000000000, 0.9659258262890683122, 1.000000000000000000, 0.9659258262890683122, 1.000000000000000000, 0.9659258262890683122, 1.000000000000000000, 0.9659258262890683122, 1.000000000000000000, 0.9659258262890683122, 1.000000000000000000, 0.9659258262890683122, 1.000000000000000000, 0.9659258262890683122, 1.000000000000000000, 0.9659258262890683122, 1.000000000000000000, 0.9659258262890683122, 1.000000000000000000, 0.9659258262890683122, 1.000000000000000000, 0.9659258262890683122, 1.000000000000000000, 0.9659258262890683122, 1.000000000000000000, 0.9659258262890683122, 1.000000000000000000, 0.9659258262890683122, 1.000000000000000000, 0.9659258262890683122, 1.000000000000000000, 0.9659258262890683122, 1.000000000000000000, 0.9659258262890683122, 1.000000000000000000, 0.9659258262890683122, 1.000000000000000000, 0.9659258262890683122, 1.000000000000000000, 0.9659258262890683122, 1.000000000000000000, 0.9659258262890683122, 1.000000000000000000, 0.9659258262890683122, 1.000000000000000000, 0.9659258262890683122, 1.000000000000000000, 0.9659258262890683122, 1.000000000000000000, 0.9659258262890683122, 1.000000000000000000, 0.9659258262890683122, 1.000000000000000000, 0.9659258262890683122, 1.000000000000000000, 0.9659258262890683122, 1.000000000000000000, 0.9659258262890683122, 1.000000000000000000, 0.9659258262890683122, 1.000000000000000000, 0.9659258262890683122, 1.000000000000000000, 0.9659258262890683122, 1.000000000000000000, 0.9659258262890683122, 1.000000000000000000, 0.9659258262890683122, 1.000000000000000000, 0.9659258262890683122, 1.000000000000000000, 0.9659258262890683122, 1.000000000000000000, 0.9659258262890683122, 1.000000000000000000, 0.9659258262890683122, 1.000000000000000000, 0.9659258262890683122, 1.000000000000000000, 0.9659258262890683122, 1.000000000000000000, 0.9659258262890683122, 1.000000000000000000, 0.9659258262890683122, 1.000000000000000000, 0.9659258262890683122, 1.000000000000000000, 0.9659258262890683122, 1.000000000000000000, 0.9659258262890683122, 1.000000000000000000, 0.9659258262890683122, 1.000000000000000000, 0.9659258262890683122, 1.000000000000000000, 0.9659258262890683122, 1.000000000000000000, 0.9659258262890683122, 1.000000000000000000, 0.9659258262890683122, 1.000000000000000000, 0.9659258262890683122, 1.000000000000000000, 0.9659258262890683122, 1.000000000000000000, 0.9659258262890683122, 1.000000000000000000, 0.9659258262890683122, 1.000000000000000000, 0.9659258262890683122, 1.000000000000000000, 0.9659258262890683122, 1.000000000000000000, 0.9659258262890683122, 1.000000000000000000, 0.9659258262890683122, 1.000000000000000000, 0.9659258262890683122, 1.000000000000000000, 0.9659258262890683122, 1.000000000000000000, 0.9659258262890683122, 1.000000000000000000, 0.9659258262890683122, 1.000000000000000000, 0.9659258262890683122, 1.000000000000000000, 0.9659258262890683122, 1.000000000000000000, 0.9659258262890683122, 1.000000000000000000, 0.9659258262890683122, 1.000000000000000000 ) ) 
 REPRESENTATION_ITEM ( '' )  );
#26022 = CARTESIAN_POINT ( 'NONE',  ( 10.37757302488624056, 8.525000002731180970, -31.93888565452638417 ) ) ;
#26023 = CARTESIAN_POINT ( 'NONE',  ( 7.236395654485760609, 3.024999997268823293, -22.27133577429736633 ) ) ;
#26024 = CARTESIAN_POINT ( 'NONE',  ( 13.94119854578937812, 11.86236083425730925, 24.22776226481240514 ) ) ;
#26025 = ORIENTED_EDGE ( 'NONE', *, *, #13776, .T. ) ;
#26026 = CARTESIAN_POINT ( 'NONE',  ( -33.58253175000000113, 45.22500000273117848, 10.91162601494193929 ) ) ;
#26027 = ORIENTED_EDGE ( 'NONE', *, *, #33913, .F. ) ;
#26028 = CARTESIAN_POINT ( 'NONE',  ( -26.00068869287368756, 42.79427083333331439, -15.01150461594595775 ) ) ;
#26029 = CYLINDRICAL_SURFACE ( 'NONE', #24831, 32.50000000000000000 ) ;
#26030 = CARTESIAN_POINT ( 'NONE',  ( -10.04305231718579172, 6.100000005462375086, -30.90933677959248982 ) ) ;
#26031 = CARTESIAN_POINT ( 'NONE',  ( -14.47279130897151589, 5.824999997268811569, -19.92008829642072598 ) ) ;
#26032 = CARTESIAN_POINT ( 'NONE',  ( 1.577395562988744260E-15, 0.5000000000000133227, -25.76082449383753925 ) ) ;
#26033 = CARTESIAN_POINT ( 'NONE',  ( -33.58253175000000113, 17.37500000273117706, 0.000000000000000000 ) ) ;
#26034 = CARTESIAN_POINT ( 'NONE',  ( -10.04305231718579172, 63.59999999999998721, -30.90933677959248982 ) ) ;
#26035 = CARTESIAN_POINT ( 'NONE',  ( -24.50000000000000711, 5.100000000000012967, 7.960532557706201828 ) ) ;
#26036 = CARTESIAN_POINT ( 'NONE',  ( -20.08610463437157989, 29.69999999999999218, -27.64615127144129758 ) ) ;
#26037 = CARTESIAN_POINT ( 'NONE',  ( 20.50609665440969565, 12.85937500000000000, -20.50609665441004736 ) ) ;
#26038 = CARTESIAN_POINT ( 'NONE',  ( 11.25946833292375793, 74.17500000273119554, 8.180482586598731842 ) ) ;
#26039 = CARTESIAN_POINT ( 'NONE',  ( -26.00068869287368756, 39.35677083333333570, -15.01150461594595775 ) ) ;
#26040 = APPLICATION_PROTOCOL_DEFINITION ( 'draft international standard', 'automotive_design', 1998, #9647 ) ;
#26041 = CARTESIAN_POINT ( 'NONE',  ( 8.891200544363830713E-16, 81.50000000000001421, -15.00000000000000000 ) ) ;
#26042 = CARTESIAN_POINT ( 'NONE',  ( 23.41746824999999887, 19.12499999726882649, 0.000000000000000000 ) ) ;
#26043 = CARTESIAN_POINT ( 'NONE',  ( 26.29305231718579350, 8.800000000000002487, 19.10302069950537529 ) ) ;
#26044 = STYLED_ITEM ( 'NONE', ( #7908 ), #32186 ) ;
#26045 = DIRECTION ( 'NONE',  ( -1.224646799147353454E-16, 1.000000000000000000, -0.000000000000000000 ) ) ;
#26046 = EDGE_CURVE ( 'NONE', #19445, #9464, #25959, .T. ) ;
#26047 = CARTESIAN_POINT ( 'NONE',  ( -19.06425588902558133, 54.39024333240934794, 19.11951029504797006 ) ) ;
#26048 = CARTESIAN_POINT ( 'NONE',  ( 10.37757302488624767, 49.72500000273119269, 31.93888565452638417 ) ) ;
#26049 = CARTESIAN_POINT ( 'NONE',  ( 27.16883889988623935, 58.57500000273117990, -19.73931689729374384 ) ) ;
#26050 = CARTESIAN_POINT ( 'NONE',  ( 20.75514604977248467, 42.67500000273119554, -28.56700777964554305 ) ) ;
#26051 = CARTESIAN_POINT ( 'NONE',  ( 0.000000000000000000, -21.99999999999999645, 0.000000000000000000 ) ) ;
#26052 = EDGE_CURVE ( 'NONE', #15393, #31882, #7936, .T. ) ;
#26053 = DIRECTION ( 'NONE',  ( 0.000000000000000000, 0.000000000000000000, -1.000000000000000000 ) ) ;
#26054 = DIRECTION ( 'NONE',  ( 0.000000000000000000, 1.000000000000000000, 0.000000000000000000 ) ) ;
#26055 = FACE_OUTER_BOUND ( 'NONE', #16862, .T. ) ;
#26056 = CARTESIAN_POINT ( 'NONE',  ( 5.779280353836490358E-15, 28.50000000000000355, 32.49999999999999289 ) ) ;
#26057 = CARTESIAN_POINT ( 'NONE',  ( 20.75514604977248467, 12.42500000273117777, -28.56700777964554305 ) ) ;
#26058 = LINE ( 'NONE', #23138, #13875 ) ;
#26059 = DIRECTION ( 'NONE',  ( -0.000000000000000000, -1.000000000000000000, -0.000000000000000000 ) ) ;
#26060 = DIRECTION ( 'NONE',  ( 0.000000000000000000, 0.000000000000000000, -1.000000000000000000 ) ) ;
#26061 = CARTESIAN_POINT ( 'NONE',  ( 27.95245687107223276, 18.72618083240936215, -0.04044903255042905932 ) ) ;
#26062 = CARTESIAN_POINT ( 'NONE',  ( 26.29305231718578995, 35.70000000546237828, -19.10302069950538240 ) ) ;
#26063 = CARTESIAN_POINT ( 'NONE',  ( 15.14183272437242422, 18.04999999453762172, -20.84094480462497856 ) ) ;
#26064 = CARTESIAN_POINT ( 'NONE',  ( 27.16883889988623935, 26.32500000273119056, -19.73931689729374384 ) ) ;
#26065 = CARTESIAN_POINT ( 'NONE',  ( -26.07999730980490583, 46.08854166666666430, -6.988114217767815717 ) ) ;
#26066 = ORIENTED_EDGE ( 'NONE', *, *, #3297, .T. ) ;
#26067 = CARTESIAN_POINT ( 'NONE',  ( -27.16883889988624290, 62.92500000273119554, -19.73931689729374028 ) ) ;
#26068 = CARTESIAN_POINT ( 'NONE',  ( -20.50609665441004736, 46.37500000000000000, -20.50609665440969565 ) ) ;
#26069 = ORIENTED_EDGE ( 'NONE', *, *, #32784, .F. ) ;
#26070 = CARTESIAN_POINT ( 'NONE',  ( 15.01150461594596308, 16.15364583333333215, -26.00068869287367335 ) ) ;
#26071 = CARTESIAN_POINT ( 'NONE',  ( 26.02091320914851025, 17.87798583425730570, -14.97647472619946463 ) ) ;
#26072 = CARTESIAN_POINT ( 'NONE',  ( -33.58253175000000113, 5.025000002731194293, -10.91162601494193218 ) ) ;
#26073 = CARTESIAN_POINT ( 'NONE',  ( -11.54700538379251817, 96.00000000000002842, 19.99999999999999645 ) ) ;
#26074 = CARTESIAN_POINT ( 'NONE',  ( -27.16883889988624290, 37.17500000273118843, -19.73931689729374028 ) ) ;
#26075 = CARTESIAN_POINT ( 'NONE',  ( -20.08610463437156923, 36.80000000546239391, 27.64615127144130113 ) ) ;
#26076 = PRESENTATION_LAYER_ASSIGNMENT (  '', '', ( #29900 ) ) ;
#26077 = CARTESIAN_POINT ( 'NONE',  ( 12.13525491562420910, 79.19999999999998863, -8.816778784387098611 ) ) ;
#26078 = CARTESIAN_POINT ( 'NONE',  ( 20.50609665441005092, 65.28125000000000000, 20.50609665440969209 ) ) ;
#26079 = CARTESIAN_POINT ( 'NONE',  ( -20.75514604977248112, 25.42500000273119198, 28.56700777964554661 ) ) ;
#26080 = CARTESIAN_POINT ( 'NONE',  ( 24.50000000000000000, 5.649999994537638237, 7.960532557706212486 ) ) ;
#26081 = CARTESIAN_POINT ( 'NONE',  ( 33.58253175000000113, 52.37500000273121259, -4.112674001490185761E-15 ) ) ;
#26082 = SHAPE_REPRESENTATION_RELATIONSHIP ( 'NONE' , 'NONE' ,  #33740, #13626 ) ;
#26083 = CARTESIAN_POINT ( 'NONE',  ( -10.04305231718579172, 29.60000000000000142, -30.90933677959248982 ) ) ;
#26084 = CARTESIAN_POINT ( 'NONE',  ( 20.08610463437157279, 25.29999999999998650, -27.64615127144129758 ) ) ;
#26085 = CARTESIAN_POINT ( 'NONE',  ( -19.82091636218621034, 2.799999999999997158, -14.40073868116559552 ) ) ;
#26086 = CARTESIAN_POINT ( 'NONE',  ( -10.37757302488624411, 68.72500000273117848, -31.93888565452638417 ) ) ;
#26087 = CARTESIAN_POINT ( 'NONE',  ( -30.82792611048012787, 66.99999999999995737, 12.22707559850328174 ) ) ;
#26088 = CARTESIAN_POINT ( 'NONE',  ( -20.75514604977248823, 63.07500000273119412, -28.56700777964554305 ) ) ;
#26089 = DIRECTION ( 'NONE',  ( 0.000000000000000000, 0.000000000000000000, -1.000000000000000000 ) ) ;
#26090 = CARTESIAN_POINT ( 'NONE',  ( 20.75514604977248467, 14.42500000273119021, -28.56700777964554305 ) ) ;
#26091 = CARTESIAN_POINT ( 'NONE',  ( 19.06425588902592239, 32.34413166759064495, 19.11951029504763611 ) ) ;
#26092 = CARTESIAN_POINT ( 'NONE',  ( 15.83883214465800826, 67.00000000000004263, -29.08710441171870542 ) ) ;
#26093 = CARTESIAN_POINT ( 'NONE',  ( -27.16883889988623935, 1.575000002731197224, 19.73931689729374739 ) ) ;
#26094 = CARTESIAN_POINT ( 'NONE',  ( 33.58253175000000823, 36.02500000273117564, 10.91162601494192863 ) ) ;
#26095 = DIRECTION ( 'NONE',  ( 0.8660254037844387076, 0.000000000000000000, -0.4999999999999998890 ) ) ;
#26096 = CARTESIAN_POINT ( 'NONE',  ( 0.000000000000000000, 80.00000000000001421, 0.000000000000000000 ) ) ;
#26097 = CARTESIAN_POINT ( 'NONE',  ( 11.25946833292375793, 74.07500000273120122, -8.180482586598735395 ) ) ;
#26098 = CARTESIAN_POINT ( 'NONE',  ( -25.98046417659831420, 51.09597249907602645, 15.04653450569339945 ) ) ;
#26099 = CARTESIAN_POINT ( 'NONE',  ( 10.04305231718578817, 51.90000000546239534, -30.90933677959249337 ) ) ;
#26100 = CARTESIAN_POINT ( 'NONE',  ( -8.960552108402742093E-16, 78.87500000273118417, -14.63369212191046387 ) ) ;
#26101 =( NAMED_UNIT ( * ) PLANE_ANGLE_UNIT ( ) SI_UNIT ( $, .RADIAN. ) );
#26102 = CARTESIAN_POINT ( 'NONE',  ( 26.07999730980490227, 20.30729166666666430, 6.988114217767821046 ) ) ;
#26103 = CARTESIAN_POINT ( 'NONE',  ( -10.04305231718579172, 53.60000000000000853, -30.90933677959248982 ) ) ;
#26104 = CARTESIAN_POINT ( 'NONE',  ( -32.50000000000000000, 70.60000000546234844, 10.55989012756946366 ) ) ;
#26105 = CARTESIAN_POINT ( 'NONE',  ( 7.505752307972854531, 22.88541666666666430, -28.01184896238303423 ) ) ;
#26106 = CARTESIAN_POINT ( 'NONE',  ( 33.58253175000000113, 32.37500000273117706, -4.112674001490185761E-15 ) ) ;
#26107 = CARTESIAN_POINT ( 'NONE',  ( 18.94512977948576093, 11.32499999726882578, -13.76444248337722875 ) ) ;
#26108 = EDGE_LOOP ( 'NONE', ( #11330, #33157, #15187, #25454 ) ) ;
#26109 = CARTESIAN_POINT ( 'NONE',  ( 28.00173670424549499, 42.37017333425730925, 7.543491769121417612 ) ) ;
#26110 = CARTESIAN_POINT ( 'NONE',  ( -20.08610463437157989, 24.20000000546238184, -27.64615127144129758 ) ) ;
#26111 = CARTESIAN_POINT ( 'NONE',  ( -7.505752307972844761, 41.79166666666666430, 28.01184896238304134 ) ) ;
#26112 = CARTESIAN_POINT ( 'NONE',  ( -7.505752307973343918, 63.84895833333332860, -28.01184896238290989 ) ) ;
#26113 = CARTESIAN_POINT ( 'NONE',  ( -27.16883889988624290, 55.17500000273118133, -19.73931689729374028 ) ) ;
#26114 = CARTESIAN_POINT ( 'NONE',  ( 10.04305231718579705, 57.10000000546239107, 30.90933677959248982 ) ) ;
#26115 =( BOUNDED_CURVE ( )  B_SPLINE_CURVE ( 2, ( #28443, #2709, #4934, #31015, #18166, #17998, #26217, #13170, #15416, #33939, #21249, #2361, #20906 ),
 .UNSPECIFIED., .F., .F. ) 
 B_SPLINE_CURVE_WITH_KNOTS ( ( 3, 2, 2, 2, 2, 2, 3 ),
 ( 0.7500000000000000000, 0.7600000000000000089, 0.7800000000000000266, 0.8000000000000000444, 0.8199999999999999512, 0.8399999999999999689, 0.8499999999999999778 ),
 .UNSPECIFIED. ) 
 CURVE ( )  GEOMETRIC_REPRESENTATION_ITEM ( )  RATIONAL_B_SPLINE_CURVE ( ( 0.9755282581475768211, 0.9755282581475768211, 1.000000000000000000, 0.9510565162951535312, 1.000000000000000000, 0.9510565162951535312, 1.000000000000000000, 0.9510565162951535312, 1.000000000000000000, 0.9510565162951535312, 1.000000000000000000, 0.9755282581475768211, 0.9755282581475768211 ) ) 
 REPRESENTATION_ITEM ( '' )  );
#26116 = CARTESIAN_POINT ( 'NONE',  ( -7.347880794884122694E-16, -16.99999999999999645, 0.000000000000000000 ) ) ;
#26117 = CARTESIAN_POINT ( 'NONE',  ( -20.75514604977248823, 40.82500000273120122, -28.56700777964554305 ) ) ;
#26118 = FACE_OUTER_BOUND ( 'NONE', #6597, .T. ) ;
#26119 = CARTESIAN_POINT ( 'NONE',  ( 33.58253175000000823, 68.27500000273120406, 10.91162601494192863 ) ) ;
#26120 = CARTESIAN_POINT ( 'NONE',  ( 26.29305231718579350, 1.300000005462376151, 19.10302069950537529 ) ) ;
#26121 = CARTESIAN_POINT ( 'NONE',  ( -27.16883889988624290, 62.92500000273119554, -19.73931689729374028 ) ) ;
#26122 = CARTESIAN_POINT ( 'NONE',  ( -28.01184896238290278, 18.30208333333332860, 7.505752307973363457 ) ) ;
#26123 = CARTESIAN_POINT ( 'NONE',  ( -26.29305231718579350, 49.80000000000001137, -19.10302069950537884 ) ) ;
#26124 = CARTESIAN_POINT ( 'NONE',  ( -7.236395654485763274, 4.024999997268824181, 22.27133577429736633 ) ) ;
#26125 = CARTESIAN_POINT ( 'NONE',  ( -10.37757302488623701, 9.775000002731182747, 31.93888565452638417 ) ) ;
#26126 = DIRECTION ( 'NONE',  ( 0.000000000000000000, 0.000000000000000000, 1.000000000000000000 ) ) ;
#26127 = CARTESIAN_POINT ( 'NONE',  ( -19.06425588902558133, 33.76524333240934084, 19.11951029504797006 ) ) ;
#26128 = CARTESIAN_POINT ( 'NONE',  ( -8.960552108402742093E-16, 78.87500000273118417, -14.63369212191046387 ) ) ;
#26129 = CARTESIAN_POINT ( 'NONE',  ( -33.58253175000000113, 79.27500000273120406, -10.91162601494193041 ) ) ;
#26130 = CARTESIAN_POINT ( 'NONE',  ( -5.147494310547430452, 21.55125428154684286, -32.49999999999999289 ) ) ;
#26131 = CARTESIAN_POINT ( 'NONE',  ( 27.16883889988623935, 74.57500000273118701, -19.73931689729374384 ) ) ;
#26132 = ORIENTED_EDGE ( 'NONE', *, *, #32426, .F. ) ;
#26133 = AXIS2_PLACEMENT_3D ( 'NONE', #14437, #27475, #21665 ) ;
#26134 = CARTESIAN_POINT ( 'NONE',  ( 18.94512977948575738, 18.92499999726882010, 13.76444248337723408 ) ) ;
#26135 = CARTESIAN_POINT ( 'NONE',  ( 6.988114217767829928, 57.26041666666666430, -26.07999730980489872 ) ) ;
#26136 = CARTESIAN_POINT ( 'NONE',  ( 27.16883889988624290, 53.92500000273118843, 19.73931689729373673 ) ) ;
#26137 = CARTESIAN_POINT ( 'NONE',  ( 20.75514604977248467, 14.67500000273117955, -28.56700777964554305 ) ) ;
#26138 = CARTESIAN_POINT ( 'NONE',  ( -33.58253175000000113, 5.375000002731181503, 0.000000000000000000 ) ) ;
#26139 = CARTESIAN_POINT ( 'NONE',  ( 26.07999730980477437, 44.08333333333332860, -6.988114217768290004 ) ) ;
#26140 = CARTESIAN_POINT ( 'NONE',  ( 14.97647472619947351, 25.61236083425731636, 26.02091320914850314 ) ) ;
#26141 = EDGE_CURVE ( 'NONE', #13792, #24744, #12919, .T. ) ;
#26142 = CARTESIAN_POINT ( 'NONE',  ( -26.02091320914878025, 17.29388916574268720, -14.97647472619899389 ) ) ;
#26143 = CARTESIAN_POINT ( 'NONE',  ( 10.04305231718579705, 75.10000000546239107, 30.90933677959248982 ) ) ;
#26144 = CARTESIAN_POINT ( 'NONE',  ( 19.64450058003839672, 52.00000000000002132, -26.34187928026370429 ) ) ;
#26145 = CARTESIAN_POINT ( 'NONE',  ( -33.58253175000000113, 41.22500000273118559, 10.91162601494193929 ) ) ;
#26146 = CARTESIAN_POINT ( 'NONE',  ( -0.04044903255042732459, 45.36680583240934794, -27.95245687107223986 ) ) ;
#26147 = CARTESIAN_POINT ( 'NONE',  ( 7.236395654485760609, 11.02499999726880375, -22.27133577429736633 ) ) ;
#26148 = ADVANCED_FACE ( 'NONE', ( #20829 ), #15681, .T. ) ;
#26149 = EDGE_CURVE ( 'NONE', #23750, #1559, #23731, .T. ) ;
#26150 = CARTESIAN_POINT ( 'NONE',  ( -23.09401076758502924, 96.00000000000002842, 5.354274672883389237E-15 ) ) ;
#26151 = EDGE_LOOP ( 'NONE', ( #21562, #3274, #8643, #13280 ) ) ;
#26152 = CARTESIAN_POINT ( 'NONE',  ( 27.16883889988624290, 54.17500000273118843, 19.73931689729373673 ) ) ;
#26153 = CARTESIAN_POINT ( 'NONE',  ( -32.50000000000000000, 4.500000005462356789, 0.000000000000000000 ) ) ;
#26154 = CARTESIAN_POINT ( 'NONE',  ( 13.94119854578937812, 42.79986083425731636, 24.22776226481240514 ) ) ;
#26155 = CARTESIAN_POINT ( 'NONE',  ( -33.58253175000000113, 75.47500000273116427, 10.91162601494193929 ) ) ;
#26156 = EDGE_LOOP ( 'NONE', ( #22984, #33182, #27512, #8627 ) ) ;
#26157 = CARTESIAN_POINT ( 'NONE',  ( 27.16883889988624290, 21.92500000273119198, 19.73931689729373673 ) ) ;
#26158 = ADVANCED_FACE ( 'NONE', ( #33683 ), #29032, .F. ) ;
#26159 = CARTESIAN_POINT ( 'NONE',  ( -2.584737979205441561E-13, 12.42968749999999289, -30.02300923189239512 ) ) ;
#26160 =( BOUNDED_CURVE ( )  B_SPLINE_CURVE ( 2, ( #26428, #13212, #23689, #15288, #13390, #15464, #24360, #21455, #5992, #16637, #3095, #21951, #6153 ),
 .UNSPECIFIED., .F., .T. ) 
 B_SPLINE_CURVE_WITH_KNOTS ( ( 3, 2, 2, 2, 2, 2, 3 ),
 ( 0.4935897435897436125, 0.4948717948717948900, 0.4974358974358974450, 0.5000000000000000000, 0.5025641025641025550, 0.5051282051282051100, 0.5064102564102563875 ),
 .UNSPECIFIED. ) 
 CURVE ( )  GEOMETRIC_REPRESENTATION_ITEM ( )  RATIONAL_B_SPLINE_CURVE ( ( 0.9755282581475768211, 0.9755282581475768211, 1.000000000000000000, 0.9510565162951535312, 1.000000000000000000, 0.9510565162951535312, 1.000000000000000000, 0.9510565162951535312, 1.000000000000000000, 0.9510565162951535312, 1.000000000000000000, 0.9755282581475768211, 0.9755282581475768211 ) ) 
 REPRESENTATION_ITEM ( '' )  );
#26161 = ORIENTED_EDGE ( 'NONE', *, *, #23095, .F. ) ;
#26162 = DIRECTION ( 'NONE',  ( 0.000000000000000000, -0.000000000000000000, 1.000000000000000000 ) ) ;
#26163 = CARTESIAN_POINT ( 'NONE',  ( 20.75514604977248467, 58.42500000273119554, -28.56700777964554305 ) ) ;
#26164 = CARTESIAN_POINT ( 'NONE',  ( -26.00068869287368756, 53.10677083333331439, -15.01150461594595775 ) ) ;
#26165 = VECTOR ( 'NONE', #2393, 1000.000000000000000 ) ;
#26166 = DIRECTION ( 'NONE',  ( 0.7071067811865526798, 0.000000000000000000, 0.7071067811865423547 ) ) ;
#26167 = CARTESIAN_POINT ( 'NONE',  ( -14.47279130897151767, 3.824999997268816454, -19.92008829642072598 ) ) ;
#26168 = CARTESIAN_POINT ( 'NONE',  ( -20.75514604977248823, 2.825000002731177240, -28.56700777964554305 ) ) ;
#26169 = CARTESIAN_POINT ( 'NONE',  ( -15.00000000000000000, 78.35000000546237686, 4.873795443493597723 ) ) ;
#26170 = CARTESIAN_POINT ( 'NONE',  ( 0.04044903255045854962, 60.83555583240935505, 30.02300923189239867 ) ) ;
#26171 = CARTESIAN_POINT ( 'NONE',  ( 27.16883889988624290, 78.17500000273119554, 19.73931689729373673 ) ) ;
#26172 = CARTESIAN_POINT ( 'NONE',  ( -26.00068869287340334, 66.28385416666664298, 15.01150461594643559 ) ) ;
#26173 = CARTESIAN_POINT ( 'NONE',  ( -5.147494310547430452, 69.55125428154683220, -32.49999999999999289 ) ) ;
#26174 = CARTESIAN_POINT ( 'NONE',  ( -10.04305231718579172, 17.59999999999999076, -30.90933677959248982 ) ) ;
#26175 = CARTESIAN_POINT ( 'NONE',  ( 24.20753774853756113, 58.26302083333332860, 13.97622843553589789 ) ) ;
#26176 = CARTESIAN_POINT ( 'NONE',  ( 15.14183272437242245, 12.04999999453761106, -20.84094480462497856 ) ) ;
#26177 = CARTESIAN_POINT ( 'NONE',  ( -11.25946833292375793, 80.67500000273119554, -8.180482586598733619 ) ) ;
#26178 = CARTESIAN_POINT ( 'NONE',  ( -13.97622843553632421, 36.20572916666666430, -24.20753774853731599 ) ) ;
#26179 = CARTESIAN_POINT ( 'NONE',  ( 33.58253175000000113, 30.22500000273118559, -10.91162601494193751 ) ) ;
#26180 = CARTESIAN_POINT ( 'NONE',  ( 6.486482029760649416E-15, 71.62500000273119838, 35.31076352940723240 ) ) ;
#26181 = CARTESIAN_POINT ( 'NONE',  ( -33.58253175000000113, 35.27500000273120406, -10.91162601494193218 ) ) ;
#26182 = CARTESIAN_POINT ( 'NONE',  ( -33.58253175000000113, 13.27500000273119340, -10.91162601494193041 ) ) ;
#26183 = CARTESIAN_POINT ( 'NONE',  ( -26.09010956794232428, 57.55246500092398065, 6.950374756619732253 ) ) ;
#26184 = CARTESIAN_POINT ( 'NONE',  ( -2.162160676586882350E-15, 76.62500000273116996, -35.31076352940722529 ) ) ;
#26185 = DIRECTION ( 'NONE',  ( 0.000000000000000000, 0.000000000000000000, -1.000000000000000000 ) ) ;
#26186 = CARTESIAN_POINT ( 'NONE',  ( 32.50000000000000711, 54.90000000000001279, 10.55989012756945122 ) ) ;
#26187 = CARTESIAN_POINT ( 'NONE',  ( 23.41746824999999887, 14.52499999726879842, 7.608796670333735079 ) ) ;
#26188 = CARTESIAN_POINT ( 'NONE',  ( 27.16883889988623935, 62.32500000273119412, -19.73931689729374384 ) ) ;
#26189 = AXIS2_PLACEMENT_3D ( 'NONE', #4884, #5566, #20857 ) ;
#26190 = CARTESIAN_POINT ( 'NONE',  ( -7.236395654485757944, 7.724999997268805707, -22.27133577429736988 ) ) ;
#26191 = CARTESIAN_POINT ( 'NONE',  ( -33.58253175000000113, 73.37500000273118417, 0.000000000000000000 ) ) ;
#26192 = CARTESIAN_POINT ( 'NONE',  ( 27.16883889988624290, 9.925000002731193760, 19.73931689729373673 ) ) ;
#26193 = CARTESIAN_POINT ( 'NONE',  ( 23.41746824999999887, 17.12499999726882649, 0.000000000000000000 ) ) ;
#26194 = CARTESIAN_POINT ( 'NONE',  ( 19.06425588902592239, 18.59413166759064140, 19.11951029504763611 ) ) ;
#26195 = ORIENTED_EDGE ( 'NONE', *, *, #4418, .T. ) ;
#26196 = CARTESIAN_POINT ( 'NONE',  ( -33.58253175000000113, 43.02500000273118275, -10.91162601494193218 ) ) ;
#26197 = EDGE_CURVE ( 'NONE', #4016, #2966, #16016, .T. ) ;
#26198 = EDGE_LOOP ( 'NONE', ( #17416, #31840, #8462, #2630 ) ) ;
#26199 = CARTESIAN_POINT ( 'NONE',  ( 15.01150461594643204, 41.36197916666666430, 26.00068869287340334 ) ) ;
#26200 = CARTESIAN_POINT ( 'NONE',  ( 20.75514604977249178, 66.07500000273118701, 28.56700777964553950 ) ) ;
#26201 = CARTESIAN_POINT ( 'NONE',  ( 26.29305231718579350, 7.300000005462367270, 19.10302069950537529 ) ) ;
#26202 = CARTESIAN_POINT ( 'NONE',  ( -32.50000000000000000, 71.89999999999999147, -10.55989012756945300 ) ) ;
#26203 = CARTESIAN_POINT ( 'NONE',  ( 2.740863092043355209E-13, 17.58593749999999645, 30.02300923189239512 ) ) ;
#26204 = CARTESIAN_POINT ( 'NONE',  ( 7.570916362186213000, 2.400000000000013234, -23.30088464923126423 ) ) ;
#26205 = CARTESIAN_POINT ( 'NONE',  ( -20.75514604977248112, 13.67500000273118133, 28.56700777964554661 ) ) ;
#26206 = CARTESIAN_POINT ( 'NONE',  ( -32.50000000000000000, 62.09999999999999432, 10.55989012756946366 ) ) ;
#26207 = CARTESIAN_POINT ( 'NONE',  ( 20.08610463437157279, 57.80000000546236549, -27.64615127144129758 ) ) ;
#26208 = CARTESIAN_POINT ( 'NONE',  ( -32.50000000000000000, 29.89999999999998437, -10.55989012756945300 ) ) ;
#26209 = CARTESIAN_POINT ( 'NONE',  ( 15.04653450569339945, 36.48659749907601935, 25.98046417659831775 ) ) ;
#26210 = CARTESIAN_POINT ( 'NONE',  ( -11.25946833292375793, 79.17500000273119554, -8.180482586598733619 ) ) ;
#26211 = CARTESIAN_POINT ( 'NONE',  ( 20.50609665440969565, 43.79687500000000000, -20.50609665441004736 ) ) ;
#26212 = ITEM_DEFINED_TRANSFORMATION ( 'NONE', 'NONE', #24901,  #1376 ) ;
#26213 = LINE ( 'NONE', #18163, #23398 ) ;
#26214 = CARTESIAN_POINT ( 'NONE',  ( -19.82091636218621034, 12.80000000000000604, -14.40073868116559552 ) ) ;
#26215 = CARTESIAN_POINT ( 'NONE',  ( 32.50000000000000000, 5.099999999999983658, -10.55989012756945833 ) ) ;
#26216 = CIRCLE ( 'NONE', #31133, 30.00000000000000000 ) ;
#26217 = CARTESIAN_POINT ( 'NONE',  ( -15.00000000000000000, 74.00000000000001421, 0.000000000000000000 ) ) ;
#26218 = CARTESIAN_POINT ( 'NONE',  ( 7.025853678916867295, 60.69232666574269075, 26.06988505166722803 ) ) ;
#26219 = CARTESIAN_POINT ( 'NONE',  ( 27.16883889988623935, 48.32500000273117990, -19.73931689729374384 ) ) ;
#26220 = CARTESIAN_POINT ( 'NONE',  ( 10.37757302488624056, 52.77500000273120406, -31.93888565452638417 ) ) ;
#26221 = CARTESIAN_POINT ( 'NONE',  ( 27.16883889988624290, 36.17500000273118843, 19.73931689729373673 ) ) ;
#26222 =( BOUNDED_CURVE ( )  B_SPLINE_CURVE ( 2, ( #21111, #10299, #4158, #4972, #13040, #15449, #18200, #13201, #20776, #31555, #31220, #9469, #19951 ),
 .UNSPECIFIED., .F., .F. ) 
 B_SPLINE_CURVE_WITH_KNOTS ( ( 3, 2, 2, 2, 2, 2, 3 ),
 ( 0.4038461538461538547, 0.4051282051282051322, 0.4076923076923076872, 0.4102564102564102422, 0.4128205128205127972, 0.4153846153846154077, 0.4166666666666666852 ),
 .UNSPECIFIED. ) 
 CURVE ( )  GEOMETRIC_REPRESENTATION_ITEM ( )  RATIONAL_B_SPLINE_CURVE ( ( 0.9755282581475768211, 0.9755282581475768211, 1.000000000000000000, 0.9510565162951535312, 1.000000000000000000, 0.9510565162951535312, 1.000000000000000000, 0.9510565162951535312, 1.000000000000000000, 0.9510565162951535312, 1.000000000000000000, 0.9755282581475768211, 0.9755282581475768211 ) ) 
 REPRESENTATION_ITEM ( '' )  );
#26223 = CARTESIAN_POINT ( 'NONE',  ( 2.205017735002230837E-13, 57.49999999999998579, -32.50000000000000000 ) ) ;
#26224 = CARTESIAN_POINT ( 'NONE',  ( -2.428612866367529427E-13, 15.86718749999999822, -27.95245687107223276 ) ) ;
#26225 = CARTESIAN_POINT ( 'NONE',  ( -32.50000000000000000, 61.89999999999999147, -10.55989012756945300 ) ) ;
#26226 = CARTESIAN_POINT ( 'NONE',  ( 4.310114166470925490, 16.99999999999999289, -23.13846340751065611 ) ) ;
#26227 =( BOUNDED_CURVE ( )  B_SPLINE_CURVE ( 2, ( #410, #67, #31979, #12960, #3173, #5574, #31646, #13643, #31813, #8303, #23434, #5743, #23771 ),
 .UNSPECIFIED., .F., .F. ) 
 B_SPLINE_CURVE_WITH_KNOTS ( ( 3, 2, 2, 2, 2, 2, 3 ),
 ( 0.9679487179487179516, 0.9692307692307692291, 0.9717948717948717841, 0.9743589743589743390, 0.9769230769230768940, 0.9794871794871794490, 0.9807692307692307265 ),
 .UNSPECIFIED. ) 
 CURVE ( )  GEOMETRIC_REPRESENTATION_ITEM ( )  RATIONAL_B_SPLINE_CURVE ( ( 0.9755282581475768211, 0.9755282581475768211, 1.000000000000000000, 0.9510565162951535312, 1.000000000000000000, 0.9510565162951535312, 1.000000000000000000, 0.9510565162951535312, 1.000000000000000000, 0.9510565162951535312, 1.000000000000000000, 0.9755282581475768211, 0.9755282581475768211 ) ) 
 REPRESENTATION_ITEM ( '' )  );
#26228 = CARTESIAN_POINT ( 'NONE',  ( 10.04305231718579705, 78.59999999999999432, 30.90933677959248982 ) ) ;
#26229 = CARTESIAN_POINT ( 'NONE',  ( -10.37757302488624411, 16.72500000273117848, -31.93888565452638417 ) ) ;
#26230 = DIRECTION ( 'NONE',  ( 1.000000000000000000, 0.000000000000000000, 0.000000000000000000 ) ) ;
#26231 = CARTESIAN_POINT ( 'NONE',  ( -15.14183272437242067, 12.44999999453762918, -20.84094480462497856 ) ) ;
#26232 = CARTESIAN_POINT ( 'NONE',  ( 7.570916362186207671, 9.349999994537617098, 23.30088464923126779 ) ) ;
#26233 = CARTESIAN_POINT ( 'NONE',  ( 26.06988505166722803, 15.14545166574268897, -7.025853678916862854 ) ) ;
#26234 = CARTESIAN_POINT ( 'NONE',  ( -20.08610463437157989, 36.20000000546237828, -27.64615127144129758 ) ) ;
#26235 = CARTESIAN_POINT ( 'NONE',  ( 5.147494310547217289, 10.55125428154683576, 32.50000000000007105 ) ) ;
#26236 = CARTESIAN_POINT ( 'NONE',  ( -33.58253175000000113, 29.22500000273118914, 10.91162601494193929 ) ) ;
#26237 = CARTESIAN_POINT ( 'NONE',  ( -13.97622843553588901, 45.37239583333333570, 24.20753774853756823 ) ) ;
#26238 = ORIENTED_EDGE ( 'NONE', *, *, #29977, .T. ) ;
#26239 = CARTESIAN_POINT ( 'NONE',  ( 10.37757302488624056, 64.52500000273118985, -31.93888565452638417 ) ) ;
#26240 = EDGE_CURVE ( 'NONE', #28702, #220, #13432, .T. ) ;
#26241 = ORIENTED_EDGE ( 'NONE', *, *, #949, .F. ) ;
#26242 = CARTESIAN_POINT ( 'NONE',  ( -15.01150461594595775, 17.87239583333332149, 26.00068869287368756 ) ) ;
#26243 = CARTESIAN_POINT ( 'NONE',  ( -15.04653450569291984, 12.43527750092397532, 25.98046417659859486 ) ) ;
#26244 = CARTESIAN_POINT ( 'NONE',  ( -33.58253175000000113, 7.225000002731182924, 10.91162601494193929 ) ) ;
#26245 = EDGE_CURVE ( 'NONE', #26701, #21850, #14390, .T. ) ;
#26246 = CARTESIAN_POINT ( 'NONE',  ( -1.778240108872766143E-15, 9.499999999999992895, -32.49999999999999289 ) ) ;
#26247 = CARTESIAN_POINT ( 'NONE',  ( -10.37757302488624411, 36.97500000273118559, -31.93888565452638417 ) ) ;
#26248 = CARTESIAN_POINT ( 'NONE',  ( 10.04305231718578817, 35.90000000546239534, -30.90933677959249337 ) ) ;
#26249 = CARTESIAN_POINT ( 'NONE',  ( 6.277390505771533514E-15, 78.49999999999998579, 34.17252228774368916 ) ) ;
#26250 = CARTESIAN_POINT ( 'NONE',  ( -14.45873412499999944, 71.68750000136559208, 0.000000000000000000 ) ) ;
#26251 = CARTESIAN_POINT ( 'NONE',  ( 10.04305231718579705, 31.10000000546236976, 30.90933677959248982 ) ) ;
#26252 = CARTESIAN_POINT ( 'NONE',  ( -27.16883889988624290, 47.17500000273119554, -19.73931689729374028 ) ) ;
#26253 = CARTESIAN_POINT ( 'NONE',  ( -2.092463501923844636E-15, 23.49999999999998934, -34.17252228774368916 ) ) ;
#26254 = CARTESIAN_POINT ( 'NONE',  ( 32.50000000000000711, 24.90000000000000213, 10.55989012756945122 ) ) ;
#26255 = CARTESIAN_POINT ( 'NONE',  ( -24.50000000000000000, 3.000000000000002665, -3.000384657911015469E-15 ) ) ;
#26256 = CARTESIAN_POINT ( 'NONE',  ( 20.75514604977248467, 70.42500000273119554, -28.56700777964554305 ) ) ;
#26257 = CARTESIAN_POINT ( 'NONE',  ( -19.82091636218621389, 2.949999994537627401, 14.40073868116558842 ) ) ;
#26258 = CARTESIAN_POINT ( 'NONE',  ( 9.724104179731403619, 74.00000000000002842, -10.28132335189565083 ) ) ;
#26259 = CARTESIAN_POINT ( 'NONE',  ( -27.16883889988624290, 57.17500000273118133, -19.73931689729374028 ) ) ;
#26260 = CARTESIAN_POINT ( 'NONE',  ( 5.147494310547408247, 72.55125428154684641, 32.50000000000000711 ) ) ;
#26261 = CARTESIAN_POINT ( 'NONE',  ( -20.75514604977248823, 12.82500000273118168, -28.56700777964554305 ) ) ;
#26262 = CARTESIAN_POINT ( 'NONE',  ( -14.01125832528285109, 29.62277750092397355, 24.18731323226248264 ) ) ;
#26263 = DIRECTION ( 'NONE',  ( 0.000000000000000000, 0.000000000000000000, 1.000000000000000000 ) ) ;
#26264 = CARTESIAN_POINT ( 'NONE',  ( -20.75514604977248112, 5.675000002731203530, 28.56700777964554661 ) ) ;
#26265 = CARTESIAN_POINT ( 'NONE',  ( 27.16883889988624290, 33.92500000273117422, 19.73931689729373673 ) ) ;
#26266 = CARTESIAN_POINT ( 'NONE',  ( 5.779280353836490358E-15, 16.50000000000000000, 32.49999999999999289 ) ) ;
#26267 = DIRECTION ( 'NONE',  ( -0.000000000000000000, -1.000000000000000000, -0.000000000000000000 ) ) ;
#26268 = CARTESIAN_POINT ( 'NONE',  ( 8.601468415847520532, 75.57500000273117280, 11.83890561707634603 ) ) ;
#26269 = CARTESIAN_POINT ( 'NONE',  ( -7.468012846824272799, 43.79128499907601935, 28.02196122052058413 ) ) ;
#26270 = CARTESIAN_POINT ( 'NONE',  ( -32.50000000000000000, 56.50000000546238965, 0.000000000000000000 ) ) ;
#26271 = CARTESIAN_POINT ( 'NONE',  ( -4.300734207923755825, 79.77500000273118985, 13.23629886949340673 ) ) ;
#26272 = CYLINDRICAL_SURFACE ( 'NONE', #33714, 15.00000000000000000 ) ;
#26273 = CARTESIAN_POINT ( 'NONE',  ( 6.988114217767829928, 12.57291666666666252, -26.07999730980489872 ) ) ;
#26274 = CARTESIAN_POINT ( 'NONE',  ( 7.236395654485760609, 3.524999997268824181, -22.27133577429736633 ) ) ;
#26275 = CARTESIAN_POINT ( 'NONE',  ( 10.04305231718578817, 67.90000000546237402, -30.90933677959249337 ) ) ;
#26276 = CARTESIAN_POINT ( 'NONE',  ( -30.02300923189239512, 25.32031250000000000, 2.654126918244515359E-13 ) ) ;
#26277 = CARTESIAN_POINT ( 'NONE',  ( 27.16883889988624290, 30.17500000273119909, 19.73931689729373673 ) ) ;
#26278 = CARTESIAN_POINT ( 'NONE',  ( 14.47279130897151944, 15.42499999726879878, -19.92008829642072598 ) ) ;
#26279 = EDGE_LOOP ( 'NONE', ( #19310, #19987, #7769, #11695 ) ) ;
#26280 = CARTESIAN_POINT ( 'NONE',  ( -20.53372385742071771, 36.64100666759062364, 20.47846945139902530 ) ) ;
#26281 = CARTESIAN_POINT ( 'NONE',  ( 32.50000000000000000, 19.60000000546237686, -10.55989012756945833 ) ) ;
#26282 = CARTESIAN_POINT ( 'NONE',  ( -20.50609665441004736, 56.68749999999998579, -20.50609665440969565 ) ) ;
#26283 = CARTESIAN_POINT ( 'NONE',  ( -5.147494310547430452, 35.55125428154683220, -32.49999999999999289 ) ) ;
#26284 = EDGE_CURVE ( 'NONE', #7065, #16121, #16845, .T. ) ;
#26285 = CARTESIAN_POINT ( 'NONE',  ( 33.58253175000000113, 56.37500000273118417, -4.112674001490185761E-15 ) ) ;
#26286 = ADVANCED_FACE ( 'NONE', ( #1029 ), #8433, .T. ) ;
#26287 = CARTESIAN_POINT ( 'NONE',  ( 6.277390505771533514E-15, 55.00000000546239676, 34.17252228774368916 ) ) ;
#26288 = CARTESIAN_POINT ( 'NONE',  ( 7.313012447739250820E-14, 13.24999999453762456, 24.50000000000000000 ) ) ;
#26289 = CARTESIAN_POINT ( 'NONE',  ( 10.37757302488624767, 39.72500000273118559, 31.93888565452638417 ) ) ;
#26290 = CARTESIAN_POINT ( 'NONE',  ( 10.04305231718578817, 55.40000000000000568, -30.90933677959249337 ) ) ;
#26291 = CARTESIAN_POINT ( 'NONE',  ( -10.37757302488623701, 69.77500000273117564, 31.93888565452638417 ) ) ;
#26292 = CARTESIAN_POINT ( 'NONE',  ( 13.21205807576171232, 74.00000000000002842, -4.468464182411219454 ) ) ;
#26293 = CARTESIAN_POINT ( 'NONE',  ( -33.58253175000000113, 61.12500000273117706, 0.000000000000000000 ) ) ;
#26294 = CARTESIAN_POINT ( 'NONE',  ( -15.01150461594642316, 22.45572916666666430, -26.00068869287341045 ) ) ;
#26295 = CARTESIAN_POINT ( 'NONE',  ( -32.50000000000000000, 45.89999999999999858, -10.55989012756945478 ) ) ;
#26296 = CARTESIAN_POINT ( 'NONE',  ( -23.41746825000000598, 5.724999997268815477, 7.608796670333726198 ) ) ;
#26297 = CARTESIAN_POINT ( 'NONE',  ( 33.58253175000000823, 10.27500000273117564, 10.91162601494192863 ) ) ;
#26298 = CARTESIAN_POINT ( 'NONE',  ( 20.08610463437157279, 35.80000000546235839, -27.64615127144129758 ) ) ;
#26299 = CARTESIAN_POINT ( 'NONE',  ( -26.09010956794245217, 30.90065999907601579, -6.950374756619243755 ) ) ;
#26300 = CARTESIAN_POINT ( 'NONE',  ( 13.91746824999999532, 72.47500000273119269, -4.522059556121118540 ) ) ;
#26301 = CARTESIAN_POINT ( 'NONE',  ( 6.486482029760648627E-15, 77.87500000273118417, 35.31076352940722529 ) ) ;
#26302 = DIRECTION ( 'NONE',  ( -0.000000000000000000, -1.000000000000000000, -0.000000000000000000 ) ) ;
#26303 = CARTESIAN_POINT ( 'NONE',  ( -27.16883889988623935, 73.57500000273118701, 19.73931689729374739 ) ) ;
#26304 = ORIENTED_EDGE ( 'NONE', *, *, #8603, .F. ) ;
#26305 = CARTESIAN_POINT ( 'NONE',  ( 7.236395654485760609, 17.52499999726880731, -22.27133577429736633 ) ) ;
#26306 = CARTESIAN_POINT ( 'NONE',  ( 26.07999730980477437, 57.83333333333333570, -6.988114217768290004 ) ) ;
#26307 = CARTESIAN_POINT ( 'NONE',  ( 20.75514604977248467, 52.42500000273118133, -28.56700777964554305 ) ) ;
#26308 = CARTESIAN_POINT ( 'NONE',  ( 10.37757302488624056, 14.77500000273117209, -31.93888565452638417 ) ) ;
#26309 = CARTESIAN_POINT ( 'NONE',  ( -20.75514604977248823, 5.075000002731193227, -28.56700777964554305 ) ) ;
#26310 = CARTESIAN_POINT ( 'NONE',  ( -19.09188309203660694, 38.64062500000000000, 19.09188309203694800 ) ) ;
#26311 = CARTESIAN_POINT ( 'NONE',  ( 26.02091320914851025, 31.62798583425730925, -14.97647472619946463 ) ) ;
#26312 = CARTESIAN_POINT ( 'NONE',  ( -28.02196122052058413, 20.58815999907601935, -7.468012846824272799 ) ) ;
#26313 = CARTESIAN_POINT ( 'NONE',  ( -10.04305231718579172, 72.10000000546239107, -30.90933677959248982 ) ) ;
#26314 = CARTESIAN_POINT ( 'NONE',  ( 15.01861347032150640, 52.00000000000000711, -29.12398716250640263 ) ) ;
#26315 = CARTESIAN_POINT ( 'NONE',  ( 10.37757302488624056, 36.52500000273117564, -31.93888565452638417 ) ) ;
#26316 = CARTESIAN_POINT ( 'NONE',  ( 26.09010956794244507, 46.36940999907602645, 6.950374756619249084 ) ) ;
#26317 = CARTESIAN_POINT ( 'NONE',  ( -23.41746825000000243, 11.52499999726880553, -7.608796670333730638 ) ) ;
#26318 = CARTESIAN_POINT ( 'NONE',  ( 0.000000000000000000, 0.000000000000000000, 0.000000000000000000 ) ) ;
#26319 = ORIENTED_EDGE ( 'NONE', *, *, #8214, .F. ) ;
#26320 = CARTESIAN_POINT ( 'NONE',  ( -10.37757302488624411, 52.97500000273118559, -31.93888565452638417 ) ) ;
#26321 =( BOUNDED_CURVE ( )  B_SPLINE_CURVE ( 2, ( #9698, #12097, #25143, #7290, #9524, #20005, #1619, #20347, #15199, #30452, #11932, #17775, #6949 ),
 .UNSPECIFIED., .F., .F. ) 
 B_SPLINE_CURVE_WITH_KNOTS ( ( 3, 2, 2, 2, 2, 2, 3 ),
 ( 0.2115384615384615363, 0.2128205128205128138, 0.2153846153846153966, 0.2179487179487179516, 0.2205128205128205066, 0.2230769230769230893, 0.2243589743589743668 ),
 .UNSPECIFIED. ) 
 CURVE ( )  GEOMETRIC_REPRESENTATION_ITEM ( )  RATIONAL_B_SPLINE_CURVE ( ( 0.9755282581475768211, 0.9755282581475768211, 1.000000000000000000, 0.9510565162951535312, 1.000000000000000000, 0.9510565162951535312, 1.000000000000000000, 0.9510565162951535312, 1.000000000000000000, 0.9510565162951535312, 1.000000000000000000, 0.9755282581475768211, 0.9755282581475768211 ) ) 
 REPRESENTATION_ITEM ( '' )  );
#26322 = CARTESIAN_POINT ( 'NONE',  ( 32.50000000000000711, 50.89999999999999147, 10.55989012756945122 ) ) ;
#26323 = CARTESIAN_POINT ( 'NONE',  ( -19.11951029504763611, 43.51600666759065206, 19.06425588902592239 ) ) ;
#26324 = CARTESIAN_POINT ( 'NONE',  ( -27.16883889988624290, 67.17500000273119554, -19.73931689729374028 ) ) ;
#26325 = ORIENTED_EDGE ( 'NONE', *, *, #17014, .T. ) ;
#26326 = CARTESIAN_POINT ( 'NONE',  ( 27.16883889988624290, 23.92500000273119198, 19.73931689729373673 ) ) ;
#26327 = CARTESIAN_POINT ( 'NONE',  ( 28.01184896238290278, 26.89583333333332860, -7.505752307973347470 ) ) ;
#26328 = ORIENTED_EDGE ( 'NONE', *, *, #1847, .F. ) ;
#26329 = CARTESIAN_POINT ( 'NONE',  ( 5.779280353836490358E-15, 15.00000000546237899, 32.49999999999999289 ) ) ;
#26330 = CARTESIAN_POINT ( 'NONE',  ( 10.37757302488624056, 62.52500000273120406, -31.93888565452638417 ) ) ;
#26331 = CARTESIAN_POINT ( 'NONE',  ( -20.50609665440969209, 48.95312500000000000, 20.50609665441005092 ) ) ;
#26332 = DIRECTION ( 'NONE',  ( -0.7069718413157907166, -0.01953538259431455287, 0.7069718413158010417 ) ) ;
#26333 = CARTESIAN_POINT ( 'NONE',  ( 7.236395654485755280, 6.724999997268804819, 22.27133577429736988 ) ) ;
#26334 = CARTESIAN_POINT ( 'NONE',  ( -27.16883889988624290, 6.925000002731191096, -19.73931689729374028 ) ) ;
#26335 = CARTESIAN_POINT ( 'NONE',  ( 33.58253175000000113, 30.47500000273117493, -10.91162601494193751 ) ) ;
#26336 = CARTESIAN_POINT ( 'NONE',  ( 5.147494310547426899, 5.948745723915523698, -32.50000000000000000 ) ) ;
#26337 = CARTESIAN_POINT ( 'NONE',  ( -28.00173670424535644, 58.11420166574269075, 7.543491769121936308 ) ) ;
#26338 = CARTESIAN_POINT ( 'NONE',  ( -7.570916362186215665, 15.39999999999999680, 23.30088464923126423 ) ) ;
#26339 = CARTESIAN_POINT ( 'NONE',  ( -4.300734207923759378, 78.47500000273119269, -13.23629886949340495 ) ) ;
#26340 = CARTESIAN_POINT ( 'NONE',  ( 5.779280353836490358E-15, 75.00000000546236834, 32.49999999999999289 ) ) ;
#26341 = CARTESIAN_POINT ( 'NONE',  ( 20.08610463437158344, 16.69999999999999574, 27.64615127144129403 ) ) ;
#26342 = CARTESIAN_POINT ( 'NONE',  ( 26.07999730980477437, 57.83333333333333570, -6.988114217768290004 ) ) ;
#26343 = CARTESIAN_POINT ( 'NONE',  ( 1.507698388325705758E-15, 1.624999997268827823, -24.62258325217400312 ) ) ;
#26344 = CARTESIAN_POINT ( 'NONE',  ( -15.00000000000000000, 72.15000000546237402, -4.873795443493594171 ) ) ;
#26345 = CARTESIAN_POINT ( 'NONE',  ( 13.97622843553633665, 31.04947916666666075, 24.20753774853730889 ) ) ;
#26346 = CARTESIAN_POINT ( 'NONE',  ( 10.37757302488624767, 27.72500000273120335, 31.93888565452638417 ) ) ;
#26347 = CARTESIAN_POINT ( 'NONE',  ( 27.16883889988624290, 69.92500000273120975, 19.73931689729373673 ) ) ;
#26348 = CARTESIAN_POINT ( 'NONE',  ( -33.58253175000000113, 37.37500000273118417, 0.000000000000000000 ) ) ;
#26349 = CARTESIAN_POINT ( 'NONE',  ( 20.75514604977249178, 14.07500000273119944, 28.56700777964553950 ) ) ;
#26350 = CARTESIAN_POINT ( 'NONE',  ( -7.570916362186210335, 6.599999999999994316, -23.30088464923126779 ) ) ;
#26351 = CARTESIAN_POINT ( 'NONE',  ( -14.01125832528285109, 57.12277750092398065, 24.18731323226248264 ) ) ;
#26352 = CARTESIAN_POINT ( 'NONE',  ( 20.75514604977248467, 76.42500000273118133, -28.56700777964554305 ) ) ;
#26353 = CARTESIAN_POINT ( 'NONE',  ( 0.000000000000000000, 80.00000000000001421, 0.000000000000000000 ) ) ;
#26354 = CARTESIAN_POINT ( 'NONE',  ( -26.29305231718579350, 51.79999999999999716, -19.10302069950537884 ) ) ;
#26355 = CARTESIAN_POINT ( 'NONE',  ( 12.13525491562420910, 79.45000000546237118, -8.816778784387098611 ) ) ;
#26356 = CARTESIAN_POINT ( 'NONE',  ( -20.75514604977248112, 55.42500000273120264, 28.56700777964554661 ) ) ;
#26357 = CARTESIAN_POINT ( 'NONE',  ( -23.41746825000000243, 10.02499999726882507, -7.608796670333730638 ) ) ;
#26358 =( BOUNDED_CURVE ( )  B_SPLINE_CURVE ( 2, ( #15881, #28736, #25996, #15716, #10894, #2827, #23432, #10384, #26508, #21367, #26338, #23769, #18116 ),
 .UNSPECIFIED., .F., .T. ) 
 B_SPLINE_CURVE_WITH_KNOTS ( ( 3, 2, 2, 2, 2, 2, 3 ),
 ( 0.8055555555555555802, 0.8111111111111111160, 0.8222222222222221877, 0.8333333333333333703, 0.8444444444444444420, 0.8555555555555555136, 0.8611111111111111605 ),
 .UNSPECIFIED. ) 
 CURVE ( )  GEOMETRIC_REPRESENTATION_ITEM ( )  RATIONAL_B_SPLINE_CURVE ( ( 0.9755282581475768211, 0.9755282581475768211, 1.000000000000000000, 0.9510565162951535312, 1.000000000000000000, 0.9510565162951535312, 1.000000000000000000, 0.9510565162951535312, 1.000000000000000000, 0.9510565162951535312, 1.000000000000000000, 0.9755282581475765991, 0.9755282581475768211 ) ) 
 REPRESENTATION_ITEM ( '' )  );
#26359 = ORIENTED_EDGE ( 'NONE', *, *, #16405, .F. ) ;
#26360 = CARTESIAN_POINT ( 'NONE',  ( -10.37757302488623701, 75.77500000273117564, 31.93888565452638417 ) ) ;
#26361 = CARTESIAN_POINT ( 'NONE',  ( -33.58253175000000113, 1.225000002731198467, 10.91162601494193929 ) ) ;
#26362 = CARTESIAN_POINT ( 'NONE',  ( -23.41746824999999887, 1.624999997268811169, -2.867812753649727150E-15 ) ) ;
#26363 = CARTESIAN_POINT ( 'NONE',  ( -24.22776226481240514, 12.72173583425731458, 13.94119854578937812 ) ) ;
#26364 = ORIENTED_EDGE ( 'NONE', *, *, #2863, .T. ) ;
#26365 = CARTESIAN_POINT ( 'NONE',  ( 33.58253175000000113, 42.22500000273118559, -10.91162601494193751 ) ) ;
#26366 = DIRECTION ( 'NONE',  ( -0.000000000000000000, 1.000000000000000000, -0.000000000000000000 ) ) ;
#26367 = ADVANCED_FACE ( 'NONE', ( #8602 ), #6028, .T. ) ;
#26368 = VERTEX_POINT ( 'NONE', #19249 ) ;
#26369 = CARTESIAN_POINT ( 'NONE',  ( -15.01150461594595775, 41.93489583333333570, 26.00068869287368756 ) ) ;
#26370 = CARTESIAN_POINT ( 'NONE',  ( -5.147494310547423346, 60.94874572391552903, 32.50000000000000000 ) ) ;
#26371 = CARTESIAN_POINT ( 'NONE',  ( -32.50000000000000000, 4.500000005462371000, 0.000000000000000000 ) ) ;
#26372 = CARTESIAN_POINT ( 'NONE',  ( -20.08610463437157989, 71.69999999999997442, -27.64615127144129758 ) ) ;
#26373 = CARTESIAN_POINT ( 'NONE',  ( -26.00068869287368756, 22.16927083333332504, -15.01150461594595775 ) ) ;
#26374 = CARTESIAN_POINT ( 'NONE',  ( 19.82091636218621389, 0.2000000000000057288, -14.40073868116559197 ) ) ;
#26375 = CARTESIAN_POINT ( 'NONE',  ( -20.75514604977248112, 7.675000002731199089, 28.56700777964554661 ) ) ;
#26376 = CARTESIAN_POINT ( 'NONE',  ( 10.04305231718579705, 60.59999999999998721, 30.90933677959248982 ) ) ;
#26377 = CARTESIAN_POINT ( 'NONE',  ( 4.300734207923757602, 78.27500000273118985, -13.23629886949340673 ) ) ;
#26378 = CARTESIAN_POINT ( 'NONE',  ( 5.779280353836490358E-15, 30.49999999999999645, 32.49999999999999289 ) ) ;
#26379 = CARTESIAN_POINT ( 'NONE',  ( 25.98046417659831775, 39.06472249907601935, -15.04653450569338879 ) ) ;
#26380 = CARTESIAN_POINT ( 'NONE',  ( -13.91746824999999532, 79.27500000273118985, -4.522059556121115875 ) ) ;
#26381 = CARTESIAN_POINT ( 'NONE',  ( 26.00068869287341045, 43.94010416666665719, -15.01150461594642493 ) ) ;
#26382 = PRODUCT_CONTEXT ( 'NONE', #20187, 'mechanical' ) ;
#26383 = DIRECTION ( 'NONE',  ( -0.000000000000000000, -1.000000000000000000, -0.000000000000000000 ) ) ;
#26384 = CARTESIAN_POINT ( 'NONE',  ( -3.880418787951138260, 1.448745718453166020, 24.50000000000000000 ) ) ;
#26385 = CARTESIAN_POINT ( 'NONE',  ( -2.092463501923844636E-15, 3.500000000000005329, -34.17252228774368916 ) ) ;
#26386 = CARTESIAN_POINT ( 'NONE',  ( 5.204170427930421283E-15, -70.99969134886156041, 0.000000000000000000 ) ) ;
#26387 = CARTESIAN_POINT ( 'NONE',  ( -7.025853678916861966, 62.41107666574269075, -26.06988505166722803 ) ) ;
#26388 = CARTESIAN_POINT ( 'NONE',  ( -2.162160676586881955E-15, 44.62500000273119838, -35.31076352940723240 ) ) ;
#26389 = CARTESIAN_POINT ( 'NONE',  ( -15.00000000000000000, 72.25000000546238255, 0.000000000000000000 ) ) ;
#26390 = CARTESIAN_POINT ( 'NONE',  ( 27.16883889988623935, 54.57500000273117280, -19.73931689729374384 ) ) ;
#26391 = CARTESIAN_POINT ( 'NONE',  ( -33.58253175000000113, 37.27500000273118985, -10.91162601494193041 ) ) ;
#26392 = CARTESIAN_POINT ( 'NONE',  ( 5.779280353836490358E-15, 24.50000000000000711, 32.49999999999999289 ) ) ;
#26393 = DIRECTION ( 'NONE',  ( -0.000000000000000000, -1.000000000000000000, -0.000000000000000000 ) ) ;
#26394 = CARTESIAN_POINT ( 'NONE',  ( -34.92499999999992610, 2.020667218593136255E-15, -16.50000000000002842 ) ) ;
#26395 = CARTESIAN_POINT ( 'NONE',  ( 32.50000000000000000, 51.60000000546239107, -10.55989012756945833 ) ) ;
#26396 = CARTESIAN_POINT ( 'NONE',  ( 32.50000000000000000, 75.00000000000000000, -3.980102097228898626E-15 ) ) ;
#26397 = CARTESIAN_POINT ( 'NONE',  ( 20.75514604977248467, 16.42500000273118133, -28.56700777964554305 ) ) ;
#26398 = CARTESIAN_POINT ( 'NONE',  ( -14.47279130897151767, 1.324999997268808238, -19.92008829642072598 ) ) ;
#26399 = CARTESIAN_POINT ( 'NONE',  ( 24.50000000000000000, 9.849999994537622428, -7.960532557706203605 ) ) ;
#26400 = CARTESIAN_POINT ( 'NONE',  ( 24.18731323226221974, 21.87722249907602290, -14.01125832528328985 ) ) ;
#26401 = CARTESIAN_POINT ( 'NONE',  ( 20.08610463437157279, 37.80000000546239391, -27.64615127144129758 ) ) ;
#26402 = CARTESIAN_POINT ( 'NONE',  ( -26.29305231718579350, 11.80000000000000426, -19.10302069950537884 ) ) ;
#26403 = CARTESIAN_POINT ( 'NONE',  ( 20.75514604977249178, 23.82500000273118346, 28.56700777964553950 ) ) ;
#26404 = CONICAL_SURFACE ( 'NONE', #6640, 14.00000000000000178, 0.2617993877991500740 ) ;
#26405 = CARTESIAN_POINT ( 'NONE',  ( -27.95245687107222921, 45.94531249999997868, 2.498001805406602216E-13 ) ) ;
#26406 = ORIENTED_EDGE ( 'NONE', *, *, #16371, .F. ) ;
#26407 = CARTESIAN_POINT ( 'NONE',  ( -20.75514604977248112, 65.42500000273118133, 28.56700777964554661 ) ) ;
#26408 = ORIENTED_EDGE ( 'NONE', *, *, #21950, .T. ) ;
#26409 = CARTESIAN_POINT ( 'NONE',  ( 20.50609665441005092, 13.71874999999999467, 20.50609665440969209 ) ) ;
#26410 = CARTESIAN_POINT ( 'NONE',  ( 20.53372385742072481, 14.29725666759064318, -20.47846945139902175 ) ) ;
#26411 = CARTESIAN_POINT ( 'NONE',  ( 33.58253175000000823, 8.025000002731188076, 10.91162601494192863 ) ) ;
#26412 = ORIENTED_EDGE ( 'NONE', *, *, #3757, .T. ) ;
#26413 = DIRECTION ( 'NONE',  ( 0.000000000000000000, 0.000000000000000000, -1.000000000000000000 ) ) ;
#26414 = CARTESIAN_POINT ( 'NONE',  ( 10.37757302488624767, 31.97500000273117848, 31.93888565452638417 ) ) ;
#26415 = CARTESIAN_POINT ( 'NONE',  ( 20.08610463437158344, 35.20000000546237828, 27.64615127144129403 ) ) ;
#26416 = CARTESIAN_POINT ( 'NONE',  ( 10.04305231718579705, 78.60000000000000853, 30.90933677959248982 ) ) ;
#26417 = CARTESIAN_POINT ( 'NONE',  ( 20.08610463437157279, 53.29999999999999716, -27.64615127144129758 ) ) ;
#26418 = CARTESIAN_POINT ( 'NONE',  ( 26.29305231718578995, 77.19999999999998863, -19.10302069950538240 ) ) ;
#26419 = CARTESIAN_POINT ( 'NONE',  ( 33.58253175000000113, 44.37500000273119838, -4.112674001490185761E-15 ) ) ;
#26420 =( BOUNDED_CURVE ( )  B_SPLINE_CURVE ( 2, ( #14467, #24924, #904, #21862, #19284, #16713, #24592, #29901, #17731, #2100, #12573, #9654, #30753 ),
 .UNSPECIFIED., .F., .T. ) 
 B_SPLINE_CURVE_WITH_KNOTS ( ( 3, 2, 2, 2, 2, 2, 3 ),
 ( 0.6858974358974359031, 0.6871794871794871806, 0.6897435897435897356, 0.6923076923076922906, 0.6948717948717948456, 0.6974358974358974006, 0.6987179487179486781 ),
 .UNSPECIFIED. ) 
 CURVE ( )  GEOMETRIC_REPRESENTATION_ITEM ( )  RATIONAL_B_SPLINE_CURVE ( ( 0.9755282581475768211, 0.9755282581475768211, 1.000000000000000000, 0.9510565162951535312, 1.000000000000000000, 0.9510565162951535312, 1.000000000000000000, 0.9510565162951535312, 1.000000000000000000, 0.9510565162951535312, 1.000000000000000000, 0.9755282581475768211, 0.9755282581475768211 ) ) 
 REPRESENTATION_ITEM ( '' )  );
#26421 = CARTESIAN_POINT ( 'NONE',  ( -26.29305231718578995, 20.19999999999998153, 19.10302069950538595 ) ) ;
#26422 = CARTESIAN_POINT ( 'NONE',  ( -20.08610463437157989, 19.69999999999998863, -27.64615127144129758 ) ) ;
#26423 = CARTESIAN_POINT ( 'NONE',  ( -7.570916362186210335, 8.599999999999996092, -23.30088464923126779 ) ) ;
#26424 = CARTESIAN_POINT ( 'NONE',  ( 27.16883889988624290, 71.92500000273119554, 19.73931689729373673 ) ) ;
#26425 = FACE_OUTER_BOUND ( 'NONE', #27241, .T. ) ;
#26426 = CARTESIAN_POINT ( 'NONE',  ( -10.04305231718578462, 76.90000000546237402, 30.90933677959249337 ) ) ;
#26427 = CARTESIAN_POINT ( 'NONE',  ( 27.16883889988624290, 54.17500000273117422, 19.73931689729373673 ) ) ;
#26428 = CARTESIAN_POINT ( 'NONE',  ( -1.778240108872766143E-15, 40.00000000546237544, -32.49999999999999289 ) ) ;
#26429 = CARTESIAN_POINT ( 'NONE',  ( -10.37757302488623701, 9.525000002731182747, 31.93888565452638417 ) ) ;
#26430 = CARTESIAN_POINT ( 'NONE',  ( 24.22776226481241224, 31.62798583425730925, -13.94119854578936923 ) ) ;
#26431 = EDGE_CURVE ( 'NONE', #22217, #26665, #16998, .T. ) ;
#26432 = CARTESIAN_POINT ( 'NONE',  ( 3.880418787951153803, 9.301254276084472750, 24.49999999999999645 ) ) ;
#26433 = CARTESIAN_POINT ( 'NONE',  ( -25.10896554811091974, 52.00000000000000000, 21.28139962774348604 ) ) ;
#26434 = CARTESIAN_POINT ( 'NONE',  ( 33.58253175000000113, 34.22500000273117848, -10.91162601494193751 ) ) ;
#26435 = CARTESIAN_POINT ( 'NONE',  ( -10.04305231718579172, 64.10000000546239107, -30.90933677959248982 ) ) ;
#26436 = CARTESIAN_POINT ( 'NONE',  ( 0.000000000000000000, 80.00000000000001421, -32.50000000000000000 ) ) ;
#26437 = EDGE_CURVE ( 'NONE', #8956, #438, #2768, .T. ) ;
#26438 = CARTESIAN_POINT ( 'NONE',  ( 13.91746824999999887, 77.87500000273116996, -1.704398294459741270E-15 ) ) ;
#26439 = CARTESIAN_POINT ( 'NONE',  ( 20.53372385742108008, 50.09336833240935505, 20.47846945139866648 ) ) ;
#26440 = CARTESIAN_POINT ( 'NONE',  ( 6.277390505771533514E-15, 53.00000000546237544, 34.17252228774368916 ) ) ;
#26441 = CARTESIAN_POINT ( 'NONE',  ( -13.91746824999999532, 79.27500000273117564, -4.522059556121115875 ) ) ;
#26442 = CARTESIAN_POINT ( 'NONE',  ( 10.04305231718579705, 60.59999999999998721, 30.90933677959248982 ) ) ;
#26443 = AXIS2_PLACEMENT_3D ( 'NONE', #921, #6078, #32162 ) ;
#26444 = CARTESIAN_POINT ( 'NONE',  ( 24.20753774853756113, 17.01302083333332504, 13.97622843553589789 ) ) ;
#26445 = CARTESIAN_POINT ( 'NONE',  ( -2.092463501923844636E-15, 72.00000000546236834, -34.17252228774368916 ) ) ;
#26446 = CARTESIAN_POINT ( 'NONE',  ( -2.584737979205441561E-13, 26.17968750000000000, -30.02300923189239512 ) ) ;
#26447 = CARTESIAN_POINT ( 'NONE',  ( -10.37757302488624411, 26.97500000273118914, -31.93888565452638417 ) ) ;
#26448 = FACE_OUTER_BOUND ( 'NONE', #7269, .T. ) ;
#26449 = ORIENTED_EDGE ( 'NONE', *, *, #21220, .T. ) ;
#26450 = CARTESIAN_POINT ( 'NONE',  ( -30.02300923189239867, 40.50819416759064495, -0.04044903254991731589 ) ) ;
#26451 = CARTESIAN_POINT ( 'NONE',  ( -32.50000000000000000, 16.60000000546238752, 10.55989012756946366 ) ) ;
#26452 = CARTESIAN_POINT ( 'NONE',  ( 7.505752307973351023, 51.81770833333332860, 28.01184896238290278 ) ) ;
#26453 = CARTESIAN_POINT ( 'NONE',  ( 5.147494310547426899, 21.44874571845315003, -32.50000000000000000 ) ) ;
#26454 = CARTESIAN_POINT ( 'NONE',  ( 6.486482029760649416E-15, 53.87500000273118417, 35.31076352940723240 ) ) ;
#26455 = CARTESIAN_POINT ( 'NONE',  ( 32.50000000000000000, 53.50000000546237544, -3.980102097228898626E-15 ) ) ;
#26456 = CARTESIAN_POINT ( 'NONE',  ( 11.25946833292375793, 76.57500000273120122, -8.180482586598735395 ) ) ;
#26457 = CARTESIAN_POINT ( 'NONE',  ( 27.16883889988623935, 38.32500000273120122, -19.73931689729374384 ) ) ;
#26458 = CARTESIAN_POINT ( 'NONE',  ( -15.00000000000000000, 76.15000000546238823, -4.873795443493594171 ) ) ;
#26459 = CARTESIAN_POINT ( 'NONE',  ( -10.37757302488624411, 66.97500000273117848, -31.93888565452638417 ) ) ;
#26460 = CARTESIAN_POINT ( 'NONE',  ( 13.91805153345283230, 74.00000000000007105, -0.9002929780893395018 ) ) ;
#26461 = CARTESIAN_POINT ( 'NONE',  ( 27.16883889988623935, 64.32500000273121543, -19.73931689729374384 ) ) ;
#26462 = CARTESIAN_POINT ( 'NONE',  ( -7.505752307972844761, 21.16666666666666430, 28.01184896238304134 ) ) ;
#26463 = CARTESIAN_POINT ( 'NONE',  ( -32.50000000000000000, 40.09999999999998721, 10.55989012756946366 ) ) ;
#26464 = CARTESIAN_POINT ( 'NONE',  ( 7.236395654485760609, 5.024999997268825069, -22.27133577429736633 ) ) ;
#26465 = CARTESIAN_POINT ( 'NONE',  ( 20.75514604977248467, 8.675000002731195536, -28.56700777964554305 ) ) ;
#26466 = CARTESIAN_POINT ( 'NONE',  ( 24.50000000000000000, 19.74999999453763877, 0.000000000000000000 ) ) ;
#26467 = CARTESIAN_POINT ( 'NONE',  ( -14.01125832528328985, 38.20534749907601935, -24.18731323226223040 ) ) ;
#26468 = DIRECTION ( 'NONE',  ( 0.000000000000000000, 0.000000000000000000, -1.000000000000000000 ) ) ;
#26469 = CARTESIAN_POINT ( 'NONE',  ( -33.58253175000000113, 73.47500000273119269, 10.91162601494193929 ) ) ;
#26470 = CARTESIAN_POINT ( 'NONE',  ( 3.980102097228898626E-15, 80.00000000000001421, 32.50000000000000000 ) ) ;
#26471 = CARTESIAN_POINT ( 'NONE',  ( 10.37757302488624056, 68.77500000273118985, -31.93888565452638417 ) ) ;
#26472 = ORIENTED_EDGE ( 'NONE', *, *, #29672, .F. ) ;
#26473 = CARTESIAN_POINT ( 'NONE',  ( -18.94512977948575738, 17.92499999726882010, -13.76444248337723231 ) ) ;
#26474 = CARTESIAN_POINT ( 'NONE',  ( -6.988114217767819270, 62.41666666666666430, 26.07999730980490583 ) ) ;
#26475 = EDGE_CURVE ( 'NONE', #18611, #5175, #27470, .T. ) ;
#26476 = CARTESIAN_POINT ( 'NONE',  ( -33.58253175000000113, 53.12500000273119838, 0.000000000000000000 ) ) ;
#26477 = CARTESIAN_POINT ( 'NONE',  ( -20.75514604977248112, 15.67500000273117600, 28.56700777964554661 ) ) ;
#26478 = CARTESIAN_POINT ( 'NONE',  ( -27.16883889988623935, 3.575000002731185234, 19.73931689729374739 ) ) ;
#26479 = CARTESIAN_POINT ( 'NONE',  ( -26.07999730980490583, 39.21354166666666430, -6.988114217767815717 ) ) ;
#26480 = CARTESIAN_POINT ( 'NONE',  ( 20.47846945139902530, 28.90663166759063785, 20.53372385742071771 ) ) ;
#26481 = CARTESIAN_POINT ( 'NONE',  ( 26.02091320914876960, 22.45013916574269075, 14.97647472619900455 ) ) ;
#26482 = CARTESIAN_POINT ( 'NONE',  ( -32.50000000000000000, 74.40000000546234560, -10.55989012756945478 ) ) ;
#26483 = CARTESIAN_POINT ( 'NONE',  ( 26.85105675556561167, 51.99999999999999289, -19.27006841923020275 ) ) ;
#26484 = CARTESIAN_POINT ( 'NONE',  ( -2.162160676586882350E-15, 38.62500000273118417, -35.31076352940722529 ) ) ;
#26485 = CARTESIAN_POINT ( 'NONE',  ( -24.18731323226221974, 51.09597249907602645, 14.01125832528330406 ) ) ;
#26486 = CARTESIAN_POINT ( 'NONE',  ( 23.41746825000000243, 18.52499999726881441, 7.608796670333735079 ) ) ;
#26487 = CARTESIAN_POINT ( 'NONE',  ( -4.405589869732278832E-13, 10.49999999999998934, 32.50000000000000000 ) ) ;
#26488 = EDGE_LOOP ( 'NONE', ( #14796, #25236, #31920, #14627 ) ) ;
#26489 = CARTESIAN_POINT ( 'NONE',  ( 33.58253175000000113, 46.37500000273119127, -4.112674001490185761E-15 ) ) ;
#26490 = CARTESIAN_POINT ( 'NONE',  ( 15.00000000000000000, 77.00000000000001421, -1.836970198721029589E-15 ) ) ;
#26491 = CARTESIAN_POINT ( 'NONE',  ( -27.95245687107223986, 54.25819416759065206, -0.04044903254993292840 ) ) ;
#26492 = CARTESIAN_POINT ( 'NONE',  ( -10.37757302488623701, 71.77500000273117564, 31.93888565452638417 ) ) ;
#26493 = ORIENTED_EDGE ( 'NONE', *, *, #9981, .F. ) ;
#26494 = CARTESIAN_POINT ( 'NONE',  ( -2.162160676586881955E-15, 18.62500000273117351, -35.31076352940723240 ) ) ;
#26495 = AXIS2_PLACEMENT_3D ( 'NONE', #31605, #18590, #26468 ) ;
#26496 = CARTESIAN_POINT ( 'NONE',  ( 28.01184896238304134, 23.74479166666666430, 7.505752307972846538 ) ) ;
#26497 = VERTEX_POINT ( 'NONE', #21493 ) ;
#26498 = CARTESIAN_POINT ( 'NONE',  ( 32.50000000000000000, 65.60000000546239107, -10.55989012756945833 ) ) ;
#26499 = CARTESIAN_POINT ( 'NONE',  ( 10.37757302488624056, 64.52500000273120406, -31.93888565452638417 ) ) ;
#26500 = CARTESIAN_POINT ( 'NONE',  ( 20.50609665441005092, 44.65624999999999289, 20.50609665440969209 ) ) ;
#26501 = CARTESIAN_POINT ( 'NONE',  ( -10.04305231718579172, 16.10000000546238397, -30.90933677959248982 ) ) ;
#26502 = CARTESIAN_POINT ( 'NONE',  ( 1.577395562988744260E-15, 16.50000000000000000, -25.76082449383753925 ) ) ;
#26503 = CARTESIAN_POINT ( 'NONE',  ( -18.94512977948576093, 8.324999997268822227, 13.76444248337722698 ) ) ;
#26504 = CARTESIAN_POINT ( 'NONE',  ( 33.58253175000000823, 6.025000002731191628, 10.91162601494192863 ) ) ;
#26505 = CARTESIAN_POINT ( 'NONE',  ( 10.37757302488624056, 32.77500000273120406, -31.93888565452638417 ) ) ;
#26506 = CARTESIAN_POINT ( 'NONE',  ( -26.29305231718578995, 64.20000000000001705, 19.10302069950538595 ) ) ;
#26507 = CARTESIAN_POINT ( 'NONE',  ( -20.53372385742107653, 58.68711833240935505, -20.47846945139867003 ) ) ;
#26508 = CARTESIAN_POINT ( 'NONE',  ( -19.82091636218621389, 15.19999999999999218, 14.40073868116558842 ) ) ;
#26509 = CARTESIAN_POINT ( 'NONE',  ( -20.08610463437157989, 31.69999999999998508, -27.64615127144129758 ) ) ;
#26510 = CARTESIAN_POINT ( 'NONE',  ( -32.50000000000000000, 59.89999999999999147, -10.55989012756945300 ) ) ;
#26511 = CARTESIAN_POINT ( 'NONE',  ( -2.092463501923844636E-15, 17.50000000000000000, -34.17252228774368916 ) ) ;
#26512 = CARTESIAN_POINT ( 'NONE',  ( 2.584737979205442066E-13, 58.83593750000000711, 27.95245687107223276 ) ) ;
#26513 = CARTESIAN_POINT ( 'NONE',  ( -23.41746824999999887, 2.124999997268811391, -2.867812753649727150E-15 ) ) ;
#26514 = CARTESIAN_POINT ( 'NONE',  ( -11.25946833292375793, 73.07500000273120122, 8.180482586598737171 ) ) ;
#26515 = CARTESIAN_POINT ( 'NONE',  ( -19.09188309203660694, 35.20312500000000000, 19.09188309203694800 ) ) ;
#26516 = CARTESIAN_POINT ( 'NONE',  ( 10.37757302488624056, 26.52500000273119696, -31.93888565452638417 ) ) ;
#26517 = CARTESIAN_POINT ( 'NONE',  ( 27.16883889988623935, 72.32500000273118701, -19.73931689729374384 ) ) ;
#26518 = CARTESIAN_POINT ( 'NONE',  ( -27.16883889988624290, 37.17500000273120264, -19.73931689729374028 ) ) ;
#26519 = CARTESIAN_POINT ( 'NONE',  ( -33.58253175000000113, 15.27500000273118985, -10.91162601494193041 ) ) ;
#26520 = CARTESIAN_POINT ( 'NONE',  ( -6.950374756619716266, 58.41184000092398065, -26.09010956794232428 ) ) ;
#26521 = VECTOR ( 'NONE', #5838, 1000.000000000000114 ) ;
#26522 = CARTESIAN_POINT ( 'NONE',  ( -27.16883889988624290, 72.92500000273119554, -19.73931689729374028 ) ) ;
#26523 = CARTESIAN_POINT ( 'NONE',  ( 5.147494310547426899, 3.948745723915525474, -32.50000000000000000 ) ) ;
#26524 =( BOUNDED_CURVE ( )  B_SPLINE_CURVE ( 2, ( #30894, #30719, #1545, #7043, #12368, #14775, #2066, #4813, #17873, #12021, #9796, #22665, #14947 ),
 .UNSPECIFIED., .F., .T. ) 
 B_SPLINE_CURVE_WITH_KNOTS ( ( 3, 2, 2, 2, 2, 2, 3 ),
 ( 0.4166666666666666852, 0.4179487179487179627, 0.4205128205128205177, 0.4230769230769230727, 0.4256410256410256276, 0.4282051282051281826, 0.4294871794871795156 ),
 .UNSPECIFIED. ) 
 CURVE ( )  GEOMETRIC_REPRESENTATION_ITEM ( )  RATIONAL_B_SPLINE_CURVE ( ( 0.9755282581475768211, 0.9755282581475768211, 1.000000000000000000, 0.9510565162951535312, 1.000000000000000000, 0.9510565162951535312, 1.000000000000000000, 0.9510565162951535312, 1.000000000000000000, 0.9510565162951535312, 1.000000000000000000, 0.9755282581475762660, 0.9755282581475768211 ) ) 
 REPRESENTATION_ITEM ( '' )  );
#26525 = CARTESIAN_POINT ( 'NONE',  ( 32.50000000000000000, 53.09999999999998721, -10.55989012756945833 ) ) ;
#26526 = CARTESIAN_POINT ( 'NONE',  ( -4.635254915624208216, 72.65000000546240244, 14.26584774442730463 ) ) ;
#26527 = CARTESIAN_POINT ( 'NONE',  ( -10.37757302488623701, 55.52500000273119696, 31.93888565452638417 ) ) ;
#26528 = CARTESIAN_POINT ( 'NONE',  ( 14.47279130897151767, 13.42499999726880411, -19.92008829642072598 ) ) ;
#26529 = ORIENTED_EDGE ( 'NONE', *, *, #9209, .F. ) ;
#26530 = CARTESIAN_POINT ( 'NONE',  ( 27.16883889988624290, 66.17500000273116711, 19.73931689729373673 ) ) ;
#26531 = CARTESIAN_POINT ( 'NONE',  ( 8.891200544363830713E-16, 81.50000000000000000, -15.00000000000000000 ) ) ;
#26532 = CARTESIAN_POINT ( 'NONE',  ( -7.236395654485757944, 17.72499999726881370, -22.27133577429736988 ) ) ;
#26533 = CARTESIAN_POINT ( 'NONE',  ( -27.95245687107223986, 23.32069416759064140, -0.04044903254993292840 ) ) ;
#26534 = ORIENTED_EDGE ( 'NONE', *, *, #26437, .T. ) ;
#26535 = CARTESIAN_POINT ( 'NONE',  ( 33.58253175000000113, 42.12500000273118417, -4.112674001490185761E-15 ) ) ;
#26536 = CARTESIAN_POINT ( 'NONE',  ( -20.08610463437156923, 42.80000000546237970, 27.64615127144130113 ) ) ;
#26537 = ORIENTED_EDGE ( 'NONE', *, *, #7796, .F. ) ;
#26538 = CARTESIAN_POINT ( 'NONE',  ( -7.505752307972844761, 41.79166666666666430, 28.01184896238304134 ) ) ;
#26539 = CARTESIAN_POINT ( 'NONE',  ( 10.04305231718578817, 5.400000000000016342, -30.90933677959249337 ) ) ;
#26540 = CARTESIAN_POINT ( 'NONE',  ( 23.95873412499999944, 19.43749999590321664, 0.000000000000000000 ) ) ;
#26541 = CARTESIAN_POINT ( 'NONE',  ( 30.02300923189239512, 23.60156250000000000, -2.619432448724977703E-13 ) ) ;
#26542 = CARTESIAN_POINT ( 'NONE',  ( 1.507698388325705758E-15, 17.12499999726880517, -24.62258325217400312 ) ) ;
#26543 = CARTESIAN_POINT ( 'NONE',  ( -33.58253175000000113, 9.275000002731177418, -10.91162601494193218 ) ) ;
#26544 = CARTESIAN_POINT ( 'NONE',  ( -20.08610463437157989, 61.69999999999999574, -27.64615127144129758 ) ) ;
#26545 = CARTESIAN_POINT ( 'NONE',  ( 13.91746824999999532, 79.97500000273119269, -4.522059556121118540 ) ) ;
#26546 = CARTESIAN_POINT ( 'NONE',  ( -4.936660134684515206E-16, -18.96891108675447768, 0.000000000000000000 ) ) ;
#26547 = CARTESIAN_POINT ( 'NONE',  ( 20.47846945139867003, 35.48399333240935505, -20.53372385742107653 ) ) ;
#26548 = CARTESIAN_POINT ( 'NONE',  ( 13.91746824999999887, 74.37500000273116996, -1.704398294459741270E-15 ) ) ;
#26549 = CARTESIAN_POINT ( 'NONE',  ( 30.02300923189239867, 47.66406249999999289, -2.619432448724978208E-13 ) ) ;
#26550 = CONTEXT_DEPENDENT_SHAPE_REPRESENTATION ( #32246, #15351 ) ;
#26551 = DIRECTION ( 'NONE',  ( -0.000000000000000000, -1.000000000000000000, -0.000000000000000000 ) ) ;
#26552 = DIRECTION ( 'NONE',  ( 0.000000000000000000, 0.000000000000000000, -1.000000000000000000 ) ) ;
#26553 = CARTESIAN_POINT ( 'NONE',  ( -26.29305231718578995, 2.199999999999979750, 19.10302069950538595 ) ) ;
#26554 = CARTESIAN_POINT ( 'NONE',  ( 0.000000000000000000, -12.99999999999999822, -33.00000000000000000 ) ) ;
#26555 = CARTESIAN_POINT ( 'NONE',  ( -26.09010956794245217, 58.40065999907601935, -6.950374756619243755 ) ) ;
#26556 = CARTESIAN_POINT ( 'NONE',  ( -27.16883889988624290, 46.92500000273119554, -19.73931689729374028 ) ) ;
#26557 = CARTESIAN_POINT ( 'NONE',  ( 4.635254915624209993, 71.65000000546240244, -14.26584774442730463 ) ) ;
#26558 = CARTESIAN_POINT ( 'NONE',  ( -27.16883889988623935, 55.57500000273117280, 19.73931689729374739 ) ) ;
#26559 = CARTESIAN_POINT ( 'NONE',  ( 33.58253175000000113, 34.37500000273119127, -4.112674001490185761E-15 ) ) ;
#26560 = LINE ( 'NONE', #13527, #17167 ) ;
#26561 = CARTESIAN_POINT ( 'NONE',  ( -26.07999730980490583, 22.02604166666666430, -6.988114217767815717 ) ) ;
#26562 = DIRECTION ( 'NONE',  ( 0.000000000000000000, -0.000000000000000000, -1.000000000000000000 ) ) ;
#26563 = MECHANICAL_DESIGN_GEOMETRIC_PRESENTATION_REPRESENTATION (  '', ( #1949 ), #30379 ) ;
#26564 = CARTESIAN_POINT ( 'NONE',  ( -20.08610463437156923, 44.80000000546236549, 27.64615127144130113 ) ) ;
#26565 = CARTESIAN_POINT ( 'NONE',  ( -26.29305231718578995, 74.20000000000000284, 19.10302069950538595 ) ) ;
#26566 = CARTESIAN_POINT ( 'NONE',  ( -33.58253175000000113, 9.225000002731190918, 10.91162601494193929 ) ) ;
#26567 = CARTESIAN_POINT ( 'NONE',  ( -7.236395654485757944, 3.224999997268801266, -22.27133577429736988 ) ) ;
#26568 = ADVANCED_FACE ( 'NONE', ( #31940 ), #21659, .T. ) ;
#26569 = CYLINDRICAL_SURFACE ( 'NONE', #2329, 32.50000000000000000 ) ;
#26570 = CARTESIAN_POINT ( 'NONE',  ( 24.18731323226221974, 25.31472249907601579, -14.01125832528328985 ) ) ;
#26571 = CARTESIAN_POINT ( 'NONE',  ( 33.58253175000000823, 18.02500000273118985, 10.91162601494192685 ) ) ;
#26572 = CARTESIAN_POINT ( 'NONE',  ( -6.988114217767819270, 41.79166666666666430, 26.07999730980490583 ) ) ;
#26573 = ADVANCED_FACE ( 'NONE', ( #868 ), #31025, .T. ) ;
#26574 = VERTEX_POINT ( 'NONE', #28067 ) ;
#26575 = CARTESIAN_POINT ( 'NONE',  ( -33.58253175000000113, 63.12500000273117706, 0.000000000000000000 ) ) ;
#26576 = EDGE_CURVE ( 'NONE', #20845, #25120, #20522, .T. ) ;
#26577 = ORIENTED_EDGE ( 'NONE', *, *, #25716, .F. ) ;
#26578 = CARTESIAN_POINT ( 'NONE',  ( -7.505752307973343918, 12.28645833333333037, -28.01184896238290989 ) ) ;
#26579 = CARTESIAN_POINT ( 'NONE',  ( 14.97647472619947351, 18.73736083425731636, 26.02091320914850314 ) ) ;
#26580 = CARTESIAN_POINT ( 'NONE',  ( 10.37757302488624056, 2.525000002731189852, -31.93888565452638417 ) ) ;
#26581 = VERTEX_POINT ( 'NONE', #30802 ) ;
#26582 = CARTESIAN_POINT ( 'NONE',  ( -23.41746825000000598, 1.724999997268824581, 7.608796670333726198 ) ) ;
#26583 = CARTESIAN_POINT ( 'NONE',  ( -10.37757302488623701, 25.77500000273119696, 31.93888565452638417 ) ) ;
#26584 = COLOUR_RGB ( '', 0.09019608, 0.27058824, 0.51372549) ;
#26585 = CARTESIAN_POINT ( 'NONE',  ( -10.04305231718579172, 36.10000000546237686, -30.90933677959248982 ) ) ;
#26586 = CARTESIAN_POINT ( 'NONE',  ( -32.50000000000000000, 80.00000000000001421, 0.000000000000000000 ) ) ;
#26587 = FACE_OUTER_BOUND ( 'NONE', #18990, .T. ) ;
#26588 = CARTESIAN_POINT ( 'NONE',  ( -26.29305231718579350, 52.30000000546237970, -19.10302069950537884 ) ) ;
#26589 = CARTESIAN_POINT ( 'NONE',  ( 6.486482029760649416E-15, 43.87500000273118417, 35.31076352940723240 ) ) ;
#26590 = CARTESIAN_POINT ( 'NONE',  ( 20.08610463437157279, 25.29999999999998650, -27.64615127144129758 ) ) ;
#26591 = CARTESIAN_POINT ( 'NONE',  ( 20.08610463437158344, 20.69999999999998508, 27.64615127144129403 ) ) ;
#26592 = CARTESIAN_POINT ( 'NONE',  ( -24.50000000000000355, 4.899999999999989697, -7.960532557706207157 ) ) ;
#26593 = CARTESIAN_POINT ( 'NONE',  ( 33.58253175000000113, 64.22500000273117848, -10.91162601494193751 ) ) ;
#26594 = CARTESIAN_POINT ( 'NONE',  ( -20.08610463437156923, 78.29999999999999716, 27.64615127144130113 ) ) ;
#26595 = CARTESIAN_POINT ( 'NONE',  ( -5.580114035484361246, 74.00000000000002842, -13.73609794928142058 ) ) ;
#26596 = CARTESIAN_POINT ( 'NONE',  ( -33.58253175000000113, 51.47500000273118559, 10.91162601494193929 ) ) ;
#26597 = CARTESIAN_POINT ( 'NONE',  ( -14.47279130897151767, 5.324999997268826668, -19.92008829642072598 ) ) ;
#26598 = FACE_OUTER_BOUND ( 'NONE', #25790, .T. ) ;
#26599 = CARTESIAN_POINT ( 'NONE',  ( 33.58253175000000823, 10.02500000273118275, 10.91162601494192863 ) ) ;
#26600 = CARTESIAN_POINT ( 'NONE',  ( -26.06988505166735237, 26.90142333425731280, -7.025853678916388567 ) ) ;
#26601 = CARTESIAN_POINT ( 'NONE',  ( 0.000000000000000000, 0.000000000000000000, 0.000000000000000000 ) ) ;
#26602 = CARTESIAN_POINT ( 'NONE',  ( -0.3323905815833131383, 52.00000000000001421, 33.36564663192542923 ) ) ;
#26603 = CARTESIAN_POINT ( 'NONE',  ( -33.58253175000000113, 35.22500000273119980, 10.91162601494193929 ) ) ;
#26604 = CARTESIAN_POINT ( 'NONE',  ( 5.779280353836490358E-15, 19.00000000546237544, 32.49999999999999289 ) ) ;
#26605 = CARTESIAN_POINT ( 'NONE',  ( -32.50000000000000000, 58.40000000546237402, -10.55989012756945300 ) ) ;
#26606 = CARTESIAN_POINT ( 'NONE',  ( -11.25946833292375793, 75.07500000273120122, 8.180482586598737171 ) ) ;
#26607 = CARTESIAN_POINT ( 'NONE',  ( 20.53372385742108008, 43.21836833240935505, 20.47846945139866648 ) ) ;
#26608 = CARTESIAN_POINT ( 'NONE',  ( 20.08610463437157279, 53.80000000546237970, -27.64615127144129758 ) ) ;
#26609 = AXIS2_PLACEMENT_3D ( 'NONE', #3123, #31433, #31931 ) ;
#26610 = CARTESIAN_POINT ( 'NONE',  ( -13.91746824999999887, 73.37500000273116996, 0.000000000000000000 ) ) ;
#26611 = CARTESIAN_POINT ( 'NONE',  ( 26.07999730980490227, 16.86979166666666075, 6.988114217767821046 ) ) ;
#26612 = CARTESIAN_POINT ( 'NONE',  ( 10.04305231718578817, 71.90000000546237402, -30.90933677959249337 ) ) ;
#26613 = CARTESIAN_POINT ( 'NONE',  ( -7.505752307972844761, 17.72916666666666430, 28.01184896238304134 ) ) ;
#26614 = CARTESIAN_POINT ( 'NONE',  ( 33.58253175000000113, 26.37500000273117351, -4.112674001490185761E-15 ) ) ;
#26615 = CARTESIAN_POINT ( 'NONE',  ( 7.236395654485755280, 14.72499999726881192, 22.27133577429736988 ) ) ;
#26616 = VERTEX_POINT ( 'NONE', #28238 ) ;
#26617 = CARTESIAN_POINT ( 'NONE',  ( -0.04044903254990864921, 36.21131916759064495, 30.02300923189239867 ) ) ;
#26618 = AXIS2_PLACEMENT_3D ( 'NONE', #12534, #28317, #19917 ) ;
#26619 = CARTESIAN_POINT ( 'NONE',  ( -10.04305231718578462, 18.90000000546236691, 30.90933677959249337 ) ) ;
#26620 = CARTESIAN_POINT ( 'NONE',  ( 15.01150461594643204, 48.23697916666665719, 26.00068869287340334 ) ) ;
#26621 = CARTESIAN_POINT ( 'NONE',  ( 20.08610463437158344, 74.70000000000000284, 27.64615127144129403 ) ) ;
#26622 = CARTESIAN_POINT ( 'NONE',  ( 33.58253175000000113, 50.37500000273120548, -4.112674001490185761E-15 ) ) ;
#26623 = CARTESIAN_POINT ( 'NONE',  ( -32.50000000000000000, 58.60000000546236976, 10.55989012756946366 ) ) ;
#26624 = ADVANCED_FACE ( 'NONE', ( #7124 ), #15553, .T. ) ;
#26625 = CARTESIAN_POINT ( 'NONE',  ( 4.300734207923761154, 77.97500000273122112, 13.23629886949340495 ) ) ;
#26626 = CARTESIAN_POINT ( 'NONE',  ( -33.58253175000000113, 35.02500000273118275, -10.91162601494193218 ) ) ;
#26627 = CARTESIAN_POINT ( 'NONE',  ( 9.270509831248425314, 72.95000000546238539, 12.75976212528059683 ) ) ;
#26628 = CARTESIAN_POINT ( 'NONE',  ( 10.37757302488624767, 63.97500000273120691, 31.93888565452638417 ) ) ;
#26629 = FACE_OUTER_BOUND ( 'NONE', #8807, .T. ) ;
#26630 = CARTESIAN_POINT ( 'NONE',  ( -20.75514604977248112, 55.42500000273120264, 28.56700777964554661 ) ) ;
#26631 = CARTESIAN_POINT ( 'NONE',  ( 20.50609665441005092, 24.03124999999999645, 20.50609665440969209 ) ) ;
#26632 = CARTESIAN_POINT ( 'NONE',  ( 26.29305231718578995, 41.20000000000001705, -19.10302069950538240 ) ) ;
#26633 = CARTESIAN_POINT ( 'NONE',  ( 1.507698388325705758E-15, 5.124999997268805174, -24.62258325217400312 ) ) ;
#26634 = CARTESIAN_POINT ( 'NONE',  ( 33.58253175000000823, 6.275000002731184523, 10.91162601494192863 ) ) ;
#26635 = FACE_OUTER_BOUND ( 'NONE', #23329, .T. ) ;
#26636 = CARTESIAN_POINT ( 'NONE',  ( 13.91746824999999532, 74.47500000273116427, -4.522059556121118540 ) ) ;
#26637 = CARTESIAN_POINT ( 'NONE',  ( -33.58253175000000113, 73.27500000273120406, -10.91162601494193041 ) ) ;
#26638 = CARTESIAN_POINT ( 'NONE',  ( 0.000000000000000000, 80.00000000000001421, -32.50000000000000000 ) ) ;
#26639 = CARTESIAN_POINT ( 'NONE',  ( -33.58253175000000113, 69.37500000273121259, 0.000000000000000000 ) ) ;
#26640 = ORIENTED_EDGE ( 'NONE', *, *, #9990, .F. ) ;
#26641 = FACE_OUTER_BOUND ( 'NONE', #6343, .T. ) ;
#26642 = CARTESIAN_POINT ( 'NONE',  ( -27.95245687107222921, 56.25781249999997868, 2.498001805406602216E-13 ) ) ;
#26643 = CIRCLE ( 'NONE', #28838, 11.32050807568876749 ) ;
#26644 = CARTESIAN_POINT ( 'NONE',  ( -33.58253175000000113, 51.12500000273119127, 0.000000000000000000 ) ) ;
#26645 = CARTESIAN_POINT ( 'NONE',  ( -2.162160676586881955E-15, 12.87500000273117884, -35.31076352940723240 ) ) ;
#26646 = CARTESIAN_POINT ( 'NONE',  ( -10.37757302488623701, 5.775000002731192517, 31.93888565452638417 ) ) ;
#26647 = CARTESIAN_POINT ( 'NONE',  ( 13.97622843553589966, 40.21614583333332860, -24.20753774853756113 ) ) ;
#26648 = CARTESIAN_POINT ( 'NONE',  ( -0.04044903254990864921, 32.77381916759064495, 30.02300923189239867 ) ) ;
#26649 = CARTESIAN_POINT ( 'NONE',  ( 0.04044903255045854962, 16.14805583240936215, 30.02300923189239867 ) ) ;
#26650 = CARTESIAN_POINT ( 'NONE',  ( -32.50000000000000000, 76.50000000546238255, 0.000000000000000000 ) ) ;
#26651 = CARTESIAN_POINT ( 'NONE',  ( -26.29305231718579350, 56.30000000546237260, -19.10302069950537884 ) ) ;
#26652 = CARTESIAN_POINT ( 'NONE',  ( -20.75514604977248823, 38.82500000273120122, -28.56700777964554305 ) ) ;
#26653 = CARTESIAN_POINT ( 'NONE',  ( -0.04044903255042732459, 48.80430583240936215, -27.95245687107223986 ) ) ;
#26654 = CARTESIAN_POINT ( 'NONE',  ( -23.41746824999999887, 13.62499999726882116, -2.867812753649727150E-15 ) ) ;
#26655 = CARTESIAN_POINT ( 'NONE',  ( 24.50000000000000000, 14.00000000000001243, 0.000000000000000000 ) ) ;
#26656 = ORIENTED_EDGE ( 'NONE', *, *, #25523, .F. ) ;
#26657 = CARTESIAN_POINT ( 'NONE',  ( -20.75514604977248823, 45.07500000273117990, -28.56700777964554305 ) ) ;
#26658 = CARTESIAN_POINT ( 'NONE',  ( 5.779280353836490358E-15, 50.50000000000000000, 32.49999999999999289 ) ) ;
#26659 = CARTESIAN_POINT ( 'NONE',  ( -24.22776226481240514, 53.97173583425732346, 13.94119854578937812 ) ) ;
#26660 = CARTESIAN_POINT ( 'NONE',  ( 27.16883889988624290, 72.17500000273119554, 19.73931689729373673 ) ) ;
#26661 = ORIENTED_EDGE ( 'NONE', *, *, #17983, .F. ) ;
#26662 = CARTESIAN_POINT ( 'NONE',  ( 20.75514604977248467, 16.42500000273118133, -28.56700777964554305 ) ) ;
#26663 = CARTESIAN_POINT ( 'NONE',  ( 2.740863092043355209E-13, 24.46093749999999645, 30.02300923189239512 ) ) ;
#26664 = ADVANCED_FACE ( 'NONE', ( #7478 ), #23829, .T. ) ;
#26665 = VERTEX_POINT ( 'NONE', #21397 ) ;
#26666 = CARTESIAN_POINT ( 'NONE',  ( -7.570916362186215665, 3.149999994537633352, 23.30088464923126423 ) ) ;
#26667 = CARTESIAN_POINT ( 'NONE',  ( -27.16883889988623935, 55.32500000273118701, 19.73931689729374739 ) ) ;
#26668 = CARTESIAN_POINT ( 'NONE',  ( -26.00068869287368756, 49.66927083333330728, -15.01150461594595775 ) ) ;
#26669 = EDGE_CURVE ( 'NONE', #17411, #19608, #16803, .T. ) ;
#26670 = CARTESIAN_POINT ( 'NONE',  ( 32.50000000000000000, 15.60000000546238930, -10.55989012756945833 ) ) ;
#26671 = CARTESIAN_POINT ( 'NONE',  ( 0.000000000000000000, 80.00000000000001421, -32.50000000000000000 ) ) ;
#26672 = AXIS2_PLACEMENT_3D ( 'NONE', #19092, #26964, #3465 ) ;
#26673 = CARTESIAN_POINT ( 'NONE',  ( -7.236395654485757944, 9.724999997268806595, -22.27133577429736988 ) ) ;
#26674 = CARTESIAN_POINT ( 'NONE',  ( -33.58253175000000113, 27.47500000273118204, 10.91162601494193929 ) ) ;
#26675 = CARTESIAN_POINT ( 'NONE',  ( -2.375766604868044585, 78.69874572391553613, 14.99999999999999822 ) ) ;
#26676 = CARTESIAN_POINT ( 'NONE',  ( 30.02300923189239867, 63.41368083240934794, -0.04044903255044467877 ) ) ;
#26677 = CARTESIAN_POINT ( 'NONE',  ( -32.50000000000000000, 32.00000000000000000, 0.000000000000000000 ) ) ;
#26678 = CARTESIAN_POINT ( 'NONE',  ( 5.147494310547440222, 75.94874572391553613, -32.50000000000000000 ) ) ;
#26679 = CARTESIAN_POINT ( 'NONE',  ( 26.29305231718578995, 11.20000000000000107, -19.10302069950538240 ) ) ;
#26680 = CARTESIAN_POINT ( 'NONE',  ( -24.20753774853730889, 62.84635416666667140, 13.97622843553634020 ) ) ;
#26681 = CARTESIAN_POINT ( 'NONE',  ( -18.94512977948575738, 1.924999997268805885, -13.76444248337723231 ) ) ;
#26682 = CARTESIAN_POINT ( 'NONE',  ( 13.91746824999999887, 77.87500000273116996, -1.704398294459741270E-15 ) ) ;
#26683 = CARTESIAN_POINT ( 'NONE',  ( -19.09188309203660694, 28.32812499999999645, 19.09188309203694800 ) ) ;
#26684 = CARTESIAN_POINT ( 'NONE',  ( 10.37757302488624767, 23.72500000273119980, 31.93888565452638417 ) ) ;
#26685 = CARTESIAN_POINT ( 'NONE',  ( 10.37757302488624767, 75.72500000273117848, 31.93888565452638417 ) ) ;
#26686 = CARTESIAN_POINT ( 'NONE',  ( -33.58253175000000113, 31.37500000273117706, 0.000000000000000000 ) ) ;
#26687 = CARTESIAN_POINT ( 'NONE',  ( -10.37757302488623701, 13.77500000273118630, 31.93888565452638417 ) ) ;
#26688 = CARTESIAN_POINT ( 'NONE',  ( -0.04044903254992426173, 53.39881916759064495, 27.95245687107223276 ) ) ;
#26689 = CARTESIAN_POINT ( 'NONE',  ( 27.16883889988624290, 67.92500000273119554, 19.73931689729373673 ) ) ;
#26690 = CARTESIAN_POINT ( 'NONE',  ( 3.980102097228898626E-15, 80.00000000000001421, 32.50000000000000000 ) ) ;
#26691 = CARTESIAN_POINT ( 'NONE',  ( -10.04305231718579172, 51.60000000000002274, -30.90933677959248982 ) ) ;
#26692 = CARTESIAN_POINT ( 'NONE',  ( 9.270509831248421762, 79.55000000546237970, -12.75976212528059861 ) ) ;
#26693 = CARTESIAN_POINT ( 'NONE',  ( -27.16883889988624290, 56.92500000273120975, -19.73931689729374028 ) ) ;
#26694 = CARTESIAN_POINT ( 'NONE',  ( -23.41746824999999887, 16.12499999726882294, -2.867812753649727150E-15 ) ) ;
#26695 = CONICAL_SURFACE ( 'NONE', #17358, 13.38432950954957157, 0.2613323016132363952 ) ;
#26696 = VERTEX_POINT ( 'NONE', #29763 ) ;
#26697 = CARTESIAN_POINT ( 'NONE',  ( 27.16883889988623935, 66.57500000273118701, -19.73931689729374384 ) ) ;
#26698 = CARTESIAN_POINT ( 'NONE',  ( -26.29305231718579350, 15.79999999999998117, -19.10302069950537884 ) ) ;
#26699 = CARTESIAN_POINT ( 'NONE',  ( 18.94512977948576093, 8.824999997268822227, -13.76444248337722875 ) ) ;
#26700 = CARTESIAN_POINT ( 'NONE',  ( 7.025853678916403666, 27.76079833425730925, -26.06988505166735237 ) ) ;
#26701 = VERTEX_POINT ( 'NONE', #6270 ) ;
#26702 = AXIS2_PLACEMENT_3D ( 'NONE', #12250, #24616, #1600 ) ;
#26703 = CARTESIAN_POINT ( 'NONE',  ( 27.16883889988623935, 38.32500000273118701, -19.73931689729374384 ) ) ;
#26704 = FACE_BOUND ( 'NONE', #5472, .T. ) ;
#26705 = ORIENTED_EDGE ( 'NONE', *, *, #24376, .T. ) ;
#26706 = CARTESIAN_POINT ( 'NONE',  ( -15.01150461594595775, 55.68489583333332860, 26.00068869287368756 ) ) ;
#26707 = CARTESIAN_POINT ( 'NONE',  ( -11.54700538379251817, 96.00000000000002842, 19.99999999999999645 ) ) ;
#26708 = CARTESIAN_POINT ( 'NONE',  ( -15.14183272437242778, 3.300000000000012257, 20.84094480462497856 ) ) ;
#26709 = CARTESIAN_POINT ( 'NONE',  ( 10.37757302488624056, 74.52500000273118985, -31.93888565452638417 ) ) ;
#26710 = CARTESIAN_POINT ( 'NONE',  ( -7.505752307973343918, 22.59895833333332860, -28.01184896238290989 ) ) ;
#26711 = CARTESIAN_POINT ( 'NONE',  ( -7.570916362186215665, 1.400000000000012346, 23.30088464923126423 ) ) ;
#26712 = EDGE_CURVE ( 'NONE', #26368, #23797, #551, .T. ) ;
#26713 = CARTESIAN_POINT ( 'NONE',  ( -33.58253175000000113, 11.37500000273117351, 0.000000000000000000 ) ) ;
#26714 = CARTESIAN_POINT ( 'NONE',  ( -27.16883889988624290, 20.92500000273117422, -19.73931689729374028 ) ) ;
#26715 = CARTESIAN_POINT ( 'NONE',  ( 2.688165632520823219E-15, 77.37500000273116996, 14.63369212191046209 ) ) ;
#26716 = DIRECTION ( 'NONE',  ( -1.000000000000000000, 0.000000000000000000, 0.000000000000000000 ) ) ;
#26717 = CARTESIAN_POINT ( 'NONE',  ( 26.02091320914876960, 32.76263916574268364, 14.97647472619900455 ) ) ;
#26718 = CARTESIAN_POINT ( 'NONE',  ( 4.300734207923761154, 73.97500000273119269, 13.23629886949340495 ) ) ;
#26719 = CARTESIAN_POINT ( 'NONE',  ( -20.50609665441004736, 46.37500000000000000, -20.50609665440969565 ) ) ;
#26720 = CARTESIAN_POINT ( 'NONE',  ( -24.50000000000000000, 10.90000000000000568, -7.960532557706207157 ) ) ;
#26721 = CARTESIAN_POINT ( 'NONE',  ( -4.934616302121927505E-14, 70.50000000000000000, 32.50000000000000000 ) ) ;
#26722 = CARTESIAN_POINT ( 'NONE',  ( 26.06988505166722803, 59.83295166574269075, -7.025853678916862854 ) ) ;
#26723 =( BOUNDED_CURVE ( )  B_SPLINE_CURVE ( 2, ( #21629, #13573, #8574, #837, #11318, #16646, #30002, #26605, #27101, #11483, #32409, #21464, #24037 ),
 .UNSPECIFIED., .F., .T. ) 
 B_SPLINE_CURVE_WITH_KNOTS ( ( 3, 2, 2, 2, 2, 2, 3 ),
 ( 0.2500000000000000000, 0.2512820512820512775, 0.2538461538461538325, 0.2564102564102563875, 0.2589743589743589980, 0.2615384615384615530, 0.2628205128205128305 ),
 .UNSPECIFIED. ) 
 CURVE ( )  GEOMETRIC_REPRESENTATION_ITEM ( )  RATIONAL_B_SPLINE_CURVE ( ( 0.9755282581475768211, 0.9755282581475768211, 1.000000000000000000, 0.9510565162951535312, 1.000000000000000000, 0.9510565162951535312, 1.000000000000000000, 0.9510565162951535312, 1.000000000000000000, 0.9510565162951535312, 1.000000000000000000, 0.9755282581475768211, 0.9755282581475768211 ) ) 
 REPRESENTATION_ITEM ( '' )  );
#26724 = CARTESIAN_POINT ( 'NONE',  ( -33.58253175000000113, 43.02500000273118275, -10.91162601494193218 ) ) ;
#26725 = CARTESIAN_POINT ( 'NONE',  ( -13.91746824999999532, 78.97500000273117848, 4.522059556121122093 ) ) ;
#26726 = CARTESIAN_POINT ( 'NONE',  ( -10.37757302488623701, 57.77500000273121117, 31.93888565452638417 ) ) ;
#26727 = CARTESIAN_POINT ( 'NONE',  ( -27.16883889988624290, 37.17500000273118843, -19.73931689729374028 ) ) ;
#26728 = CARTESIAN_POINT ( 'NONE',  ( 3.880418787951134707, 17.55125428154684641, 24.50000000000000000 ) ) ;
#26729 = AXIS2_PLACEMENT_3D ( 'NONE', #1905, #23026, #4146 ) ;
#26730 = CARTESIAN_POINT ( 'NONE',  ( 26.07999730980477437, 26.89583333333332860, -6.988114217768290004 ) ) ;
#26731 = CARTESIAN_POINT ( 'NONE',  ( 0.000000000000000000, -10.99999999999999645, 0.000000000000000000 ) ) ;
#26732 = EDGE_CURVE ( 'NONE', #601, #12338, #25109, .T. ) ;
#26733 = DIRECTION ( 'NONE',  ( -0.000000000000000000, -1.000000000000000000, -0.000000000000000000 ) ) ;
#26734 = CARTESIAN_POINT ( 'NONE',  ( 26.29305231718579350, 72.80000000000001137, 19.10302069950537529 ) ) ;
#26735 = CARTESIAN_POINT ( 'NONE',  ( 33.58253175000000823, 12.02500000273117742, 10.91162601494192863 ) ) ;
#26736 = CARTESIAN_POINT ( 'NONE',  ( -7.236395654485757944, 5.224999997268803043, -22.27133577429736988 ) ) ;
#26737 = CARTESIAN_POINT ( 'NONE',  ( -32.50000000000000000, 52.50000000546236834, 0.000000000000000000 ) ) ;
#26738 = CARTESIAN_POINT ( 'NONE',  ( -27.95245687107223986, 23.88243083240935505, 0.04044903255043252877 ) ) ;
#26739 = CARTESIAN_POINT ( 'NONE',  ( -19.82091636218621389, 13.19999999999998863, 14.40073868116558842 ) ) ;
#26740 = CARTESIAN_POINT ( 'NONE',  ( -27.16883889988623935, 17.32500000273118346, 19.73931689729374739 ) ) ;
#26741 = CARTESIAN_POINT ( 'NONE',  ( 26.07999730980490227, 51.24479166666666430, 6.988114217767821046 ) ) ;
#26742 = ORIENTED_EDGE ( 'NONE', *, *, #2025, .T. ) ;
#26743 = CARTESIAN_POINT ( 'NONE',  ( 33.58253175000000113, 56.22500000273117138, -10.91162601494193751 ) ) ;
#26744 = ORIENTED_EDGE ( 'NONE', *, *, #33, .T. ) ;
#26745 = CARTESIAN_POINT ( 'NONE',  ( -15.01150461594642138, 12.14322916666666430, -26.00068869287340334 ) ) ;
#26746 = CARTESIAN_POINT ( 'NONE',  ( -7.543491769121417612, 12.29204833425730925, 28.00173670424549499 ) ) ;
#26747 = CARTESIAN_POINT ( 'NONE',  ( -27.16883889988624290, 2.925000002731187543, -19.73931689729374028 ) ) ;
#26748 = ORIENTED_EDGE ( 'NONE', *, *, #6275, .F. ) ;
#26749 = CARTESIAN_POINT ( 'NONE',  ( 6.486482029760649416E-15, 27.87500000273120193, 35.31076352940723240 ) ) ;
#26750 = AXIS2_PLACEMENT_3D ( 'NONE', #17652, #32895, #14903 ) ;
#26751 = CARTESIAN_POINT ( 'NONE',  ( 10.04305231718579705, 31.10000000546236976, 30.90933677959248982 ) ) ;
#26752 = CARTESIAN_POINT ( 'NONE',  ( -9.657523855033125146E-16, 73.50000000000001421, -15.77193336357400710 ) ) ;
#26753 = CARTESIAN_POINT ( 'NONE',  ( -5.147494310547430452, 54.05125428700922185, -32.49999999999999289 ) ) ;
#26754 = CARTESIAN_POINT ( 'NONE',  ( 32.50000000000000000, 37.60000000546235555, -10.55989012756945833 ) ) ;
#26755 = CARTESIAN_POINT ( 'NONE',  ( 33.58253175000000113, 42.37500000273119838, -4.112674001490185761E-15 ) ) ;
#26756 = SURFACE_SIDE_STYLE ('',( #29987 ) ) ;
#26757 = CARTESIAN_POINT ( 'NONE',  ( 6.277390505771533514E-15, 22.49999999999998934, 34.17252228774368916 ) ) ;
#26758 = CARTESIAN_POINT ( 'NONE',  ( 32.50000000000000000, 23.09999999999999787, -10.55989012756945833 ) ) ;
#26759 = CARTESIAN_POINT ( 'NONE',  ( 15.14183272437241889, 9.699999999999985079, 20.84094480462498211 ) ) ;
#26760 = CARTESIAN_POINT ( 'NONE',  ( -33.58253175000000113, 61.12500000273119127, 0.000000000000000000 ) ) ;
#26761 = CARTESIAN_POINT ( 'NONE',  ( -24.50000000000000355, 8.649999994537630243, -7.960532557706207157 ) ) ;
#26762 = CARTESIAN_POINT ( 'NONE',  ( -20.75514604977248823, 55.07500000273117990, -28.56700777964554305 ) ) ;
#26763 = CARTESIAN_POINT ( 'NONE',  ( 7.236395654485760609, 7.024999997268826846, -22.27133577429736633 ) ) ;
#26764 = EDGE_CURVE ( 'NONE', #29527, #24126, #10011, .T. ) ;
#26765 = DIRECTION ( 'NONE',  ( -1.000000000000000000, -1.224646799147353454E-16, 0.000000000000000000 ) ) ;
#26766 = CARTESIAN_POINT ( 'NONE',  ( 33.58253175000000113, 8.125000002731198379, -4.112674001490185761E-15 ) ) ;
#26767 = CARTESIAN_POINT ( 'NONE',  ( -0.04044903254992426173, 39.64881916759063074, 27.95245687107223276 ) ) ;
#26768 = CARTESIAN_POINT ( 'NONE',  ( 32.24336671818456779, 66.99999999999997158, -4.711964452985279550 ) ) ;
#26769 = CARTESIAN_POINT ( 'NONE',  ( -29.96643421716997224, 51.99999999999999289, 13.17858490638463387 ) ) ;
#26770 = UNCERTAINTY_MEASURE_WITH_UNIT (LENGTH_MEASURE( 1.000000000000000082E-05 ), #24512, 'distance_accuracy_value', 'NONE');
#26771 = CARTESIAN_POINT ( 'NONE',  ( 10.37757302488624767, 27.72500000273118914, 31.93888565452638417 ) ) ;
#26772 = CARTESIAN_POINT ( 'NONE',  ( -20.08610463437157989, 18.20000000546239605, -27.64615127144129758 ) ) ;
#26773 = LINE ( 'NONE', #3263, #13901 ) ;
#26774 = EDGE_CURVE ( 'NONE', #33755, #28845, #19869, .T. ) ;
#26775 = CARTESIAN_POINT ( 'NONE',  ( 15.14183272437242067, 13.70000000000000462, 20.84094480462498211 ) ) ;
#26776 = CARTESIAN_POINT ( 'NONE',  ( 7.468012846824281681, 52.38503499907601224, -28.02196122052058058 ) ) ;
#26777 = CARTESIAN_POINT ( 'NONE',  ( 6.277390505771533514E-15, 45.00000000546235412, 34.17252228774368916 ) ) ;
#26778 = CARTESIAN_POINT ( 'NONE',  ( 26.29305231718578995, 49.19999999999999574, -19.10302069950538240 ) ) ;
#26779 = CARTESIAN_POINT ( 'NONE',  ( -2.428612866367529427E-13, 26.17968750000000000, -27.95245687107222921 ) ) ;
#26780 = CARTESIAN_POINT ( 'NONE',  ( -10.04305231718579172, 68.10000000546237686, -30.90933677959248982 ) ) ;
#26781 = CARTESIAN_POINT ( 'NONE',  ( 26.00068869287367335, 34.20052083333332860, 15.01150461594596308 ) ) ;
#26782 = CARTESIAN_POINT ( 'NONE',  ( -23.41746825000000243, 16.22499999726880304, 7.608796670333725309 ) ) ;
#26783 = ORIENTED_EDGE ( 'NONE', *, *, #8324, .F. ) ;
#26784 = CARTESIAN_POINT ( 'NONE',  ( -25.98046417659859486, 40.79465250092398065, -15.04653450569291628 ) ) ;
#26785 = CARTESIAN_POINT ( 'NONE',  ( -26.29305231718578995, 16.70000000546238539, 19.10302069950538595 ) ) ;
#26786 = CARTESIAN_POINT ( 'NONE',  ( -15.01150461594642138, 49.95572916666665009, -26.00068869287340334 ) ) ;
#26787 = CARTESIAN_POINT ( 'NONE',  ( 5.779280353836490358E-15, 74.50000000000001421, 32.49999999999999289 ) ) ;
#26788 = CARTESIAN_POINT ( 'NONE',  ( -33.58253175000000113, 49.47500000273118559, 10.91162601494193929 ) ) ;
#26789 = CARTESIAN_POINT ( 'NONE',  ( 10.04305231718579705, 51.10000000546238397, 30.90933677959248982 ) ) ;
#26790 = CARTESIAN_POINT ( 'NONE',  ( 13.91746824999999887, 80.37500000273118417, -1.704398294459741270E-15 ) ) ;
#26791 = CARTESIAN_POINT ( 'NONE',  ( -10.37757302488624411, 36.72500000273118559, -31.93888565452638417 ) ) ;
#26792 = CARTESIAN_POINT ( 'NONE',  ( 0.000000000000000000, 70.00000000000000000, 24.50000000000000000 ) ) ;
#26793 = CARTESIAN_POINT ( 'NONE',  ( 10.37757302488624767, 61.97500000273120691, 31.93888565452638417 ) ) ;
#26794 = CARTESIAN_POINT ( 'NONE',  ( 13.82681134000903356, 73.99999999999998579, 1.827769615135852233 ) ) ;
#26795 = CARTESIAN_POINT ( 'NONE',  ( -33.58253175000000113, 55.02500000273118985, -10.91162601494193041 ) ) ;
#26796 = CARTESIAN_POINT ( 'NONE',  ( 6.277390505771533514E-15, 38.50000000000000711, 34.17252228774368916 ) ) ;
#26797 = CARTESIAN_POINT ( 'NONE',  ( -7.236395654485763274, 2.024999997268822405, 22.27133577429736633 ) ) ;
#26798 = CARTESIAN_POINT ( 'NONE',  ( -33.58253175000000113, 7.375000002731169069, 0.000000000000000000 ) ) ;
#26799 = CARTESIAN_POINT ( 'NONE',  ( -26.29305231718579350, 66.30000000546236549, -19.10302069950537884 ) ) ;
#26800 = CARTESIAN_POINT ( 'NONE',  ( -8.601468415847515203, 71.67500000273116711, 11.83890561707634959 ) ) ;
#26801 = CARTESIAN_POINT ( 'NONE',  ( -20.75514604977248823, 71.07500000273117280, -28.56700777964554305 ) ) ;
#26802 = CARTESIAN_POINT ( 'NONE',  ( 6.001560367445586717E-15, 3.249999994537631665, 24.50000000000000000 ) ) ;
#26803 = CARTESIAN_POINT ( 'NONE',  ( -10.37757302488624411, 70.97500000273120691, -31.93888565452638417 ) ) ;
#26804 = EDGE_LOOP ( 'NONE', ( #22186, #13794, #3981, #12080 ) ) ;
#26805 = CARTESIAN_POINT ( 'NONE',  ( -4.223320258572819786E-15, 13.50000000000000355, 24.50000000000000000 ) ) ;
#26806 = CARTESIAN_POINT ( 'NONE',  ( -6.988114217767819270, 65.85416666666665719, 26.07999730980490583 ) ) ;
#26807 = CARTESIAN_POINT ( 'NONE',  ( -1.778240108872766143E-15, 25.50000000000000711, -32.49999999999999289 ) ) ;
#26808 = CARTESIAN_POINT ( 'NONE',  ( -33.58253175000000113, 47.12500000273119127, 0.000000000000000000 ) ) ;
#26809 = CARTESIAN_POINT ( 'NONE',  ( -33.58253175000000113, 11.47500000273119625, 10.91162601494193929 ) ) ;
#26810 = CARTESIAN_POINT ( 'NONE',  ( -20.75514604977248112, 61.67500000273117422, 28.56700777964554661 ) ) ;
#26811 = CARTESIAN_POINT ( 'NONE',  ( -13.97622843553632777, 49.95572916666665009, -24.20753774853731599 ) ) ;
#26812 = CARTESIAN_POINT ( 'NONE',  ( -25.98046417659859486, 30.48215250092397710, -15.04653450569291628 ) ) ;
#26813 = CARTESIAN_POINT ( 'NONE',  ( -0.04044903255044120238, 24.74180583240935505, -30.02300923189239867 ) ) ;
#26814 = CARTESIAN_POINT ( 'NONE',  ( 20.08610463437157279, 71.80000000546236549, -27.64615127144129758 ) ) ;
#26815 = CARTESIAN_POINT ( 'NONE',  ( 13.91746824999999532, 75.97500000273116427, -4.522059556121118540 ) ) ;
#26816 = CARTESIAN_POINT ( 'NONE',  ( -27.16883889988624290, 38.92500000273118843, -19.73931689729374028 ) ) ;
#26817 = CARTESIAN_POINT ( 'NONE',  ( 14.01125832528330051, 43.36159749907602645, 24.18731323226221974 ) ) ;
#26818 = CARTESIAN_POINT ( 'NONE',  ( 23.41746825000000243, 16.52499999726882152, 7.608796670333735079 ) ) ;
#26819 = CARTESIAN_POINT ( 'NONE',  ( 32.50000000000000000, 13.60000000546239107, -10.55989012756945833 ) ) ;
#26820 = ORIENTED_EDGE ( 'NONE', *, *, #28712, .T. ) ;
#26821 = CARTESIAN_POINT ( 'NONE',  ( 20.75514604977249178, 48.07500000273120122, 28.56700777964553950 ) ) ;
#26822 = CARTESIAN_POINT ( 'NONE',  ( 5.147494310547434893, 50.55125428154684641, 32.49999999999999289 ) ) ;
#26823 = CARTESIAN_POINT ( 'NONE',  ( -13.94119854578936923, 51.39361083425730925, -24.22776226481241224 ) ) ;
#26824 = CARTESIAN_POINT ( 'NONE',  ( -20.75514604977248112, 67.67500000273116711, 28.56700777964554661 ) ) ;
#26825 = ORIENTED_EDGE ( 'NONE', *, *, #7949, .F. ) ;
#26826 = CARTESIAN_POINT ( 'NONE',  ( 20.75514604977249178, 15.82500000273117102, 28.56700777964553950 ) ) ;
#26827 = CARTESIAN_POINT ( 'NONE',  ( -28.01184896238290278, 25.17708333333332860, 7.505752307973363457 ) ) ;
#26828 = EDGE_LOOP ( 'NONE', ( #24451, #19110, #24864, #1542 ) ) ;
#26829 = DIRECTION ( 'NONE',  ( 0.000000000000000000, -0.000000000000000000, -1.000000000000000000 ) ) ;
#26830 = CARTESIAN_POINT ( 'NONE',  ( 33.58253175000000113, 54.22500000273117848, -10.91162601494193751 ) ) ;
#26831 = CARTESIAN_POINT ( 'NONE',  ( 15.01150461594596308, 57.40364583333333570, -26.00068869287367335 ) ) ;
#26832 = CARTESIAN_POINT ( 'NONE',  ( 20.08610463437158344, 15.20000000546237118, 27.64615127144129403 ) ) ;
#26833 = CARTESIAN_POINT ( 'NONE',  ( -4.223320258572819786E-15, 11.24999999453763344, 24.50000000000000000 ) ) ;
#26834 = CARTESIAN_POINT ( 'NONE',  ( 18.94512977948575738, 10.92499999726881299, 13.76444248337723408 ) ) ;
#26835 = CARTESIAN_POINT ( 'NONE',  ( 6.486482029760649416E-15, 23.87500000273117706, 35.31076352940723240 ) ) ;
#26836 = SURFACE_SIDE_STYLE ('',( #18960 ) ) ;
#26837 = CARTESIAN_POINT ( 'NONE',  ( -26.02091320914878025, 68.85638916574269786, -14.97647472619899389 ) ) ;
#26838 = CARTESIAN_POINT ( 'NONE',  ( 5.147494310547434893, 65.05125428700921475, 32.49999999999999289 ) ) ;
#26839 = CARTESIAN_POINT ( 'NONE',  ( 26.29305231718579350, 14.79999999999997939, 19.10302069950537529 ) ) ;
#26840 = CARTESIAN_POINT ( 'NONE',  ( 10.04305231718578817, 9.400000000000005684, -30.90933677959249337 ) ) ;
#26841 = ORIENTED_EDGE ( 'NONE', *, *, #18514, .F. ) ;
#26842 = CARTESIAN_POINT ( 'NONE',  ( -4.523095164977116484E-15, 2.624999997268825158, 24.62258325217400312 ) ) ;
#26843 = CARTESIAN_POINT ( 'NONE',  ( 11.25946833292375793, 77.67500000273119554, 8.180482586598731842 ) ) ;
#26844 = CARTESIAN_POINT ( 'NONE',  ( 13.97622843553633665, 34.48697916666667140, 24.20753774853730889 ) ) ;
#26845 = CARTESIAN_POINT ( 'NONE',  ( -27.16883889988623935, 23.32500000273118701, 19.73931689729374739 ) ) ;
#26846 = CARTESIAN_POINT ( 'NONE',  ( 10.37757302488624056, 70.52500000273118985, -31.93888565452638417 ) ) ;
#26847 = CARTESIAN_POINT ( 'NONE',  ( -27.16883889988623935, 29.57500000273117990, 19.73931689729374739 ) ) ;
#26848 = CARTESIAN_POINT ( 'NONE',  ( -27.16883889988623935, 13.57500000273119412, 19.73931689729374739 ) ) ;
#26849 = CARTESIAN_POINT ( 'NONE',  ( -33.58253175000000113, 17.27500000273118630, -10.91162601494193041 ) ) ;
#26850 = CARTESIAN_POINT ( 'NONE',  ( -27.95245687107223986, 61.13319416759063785, -0.04044903254993292840 ) ) ;
#26851 = CARTESIAN_POINT ( 'NONE',  ( -10.37757302488624411, 68.72500000273117848, -31.93888565452638417 ) ) ;
#26852 = DIRECTION ( 'NONE',  ( -0.000000000000000000, 1.000000000000000000, -0.000000000000000000 ) ) ;
#26853 = EDGE_CURVE ( 'NONE', #7955, #18361, #21424, .T. ) ;
#26854 = CARTESIAN_POINT ( 'NONE',  ( -8.601468415847515203, 79.67500000273118133, 11.83890561707634959 ) ) ;
#26855 = CARTESIAN_POINT ( 'NONE',  ( -20.08610463437157989, 53.69999999999999574, -27.64615127144129758 ) ) ;
#26856 = DIRECTION ( 'NONE',  ( 0.000000000000000000, -1.000000000000000000, 0.000000000000000000 ) ) ;
#26857 = CARTESIAN_POINT ( 'NONE',  ( 6.486482029760648627E-15, 57.62500000273119127, 35.31076352940722529 ) ) ;
#26858 = EDGE_CURVE ( 'NONE', #774, #390, #24903, .T. ) ;
#26859 = CARTESIAN_POINT ( 'NONE',  ( 1.507698388325705758E-15, 15.62499999726882116, -24.62258325217400312 ) ) ;
#26860 = ORIENTED_EDGE ( 'NONE', *, *, #8724, .F. ) ;
#26861 = CARTESIAN_POINT ( 'NONE',  ( 20.75514604977249178, 66.07500000273118701, 28.56700777964553950 ) ) ;
#26862 = CARTESIAN_POINT ( 'NONE',  ( -33.58253175000000113, 1.125000002731191273, 0.000000000000000000 ) ) ;
#26863 = CARTESIAN_POINT ( 'NONE',  ( -7.236395654485757944, 9.224999997268806595, -22.27133577429736988 ) ) ;
#26864 = CARTESIAN_POINT ( 'NONE',  ( -26.06988505166735237, 20.02642333425731280, -7.025853678916388567 ) ) ;
#26865 = ORIENTED_EDGE ( 'NONE', *, *, #11313, .F. ) ;
#26866 = CARTESIAN_POINT ( 'NONE',  ( 6.486482029760649416E-15, 37.62500000273118417, 35.31076352940723240 ) ) ;
#26867 = CARTESIAN_POINT ( 'NONE',  ( -26.29305231718578995, 42.70000000546237118, 19.10302069950538595 ) ) ;
#26868 = ORIENTED_EDGE ( 'NONE', *, *, #11730, .F. ) ;
#26869 = CARTESIAN_POINT ( 'NONE',  ( -20.50609665440969209, 48.95312500000000000, 20.50609665441005092 ) ) ;
#26870 = CARTESIAN_POINT ( 'NONE',  ( 5.779280353836490358E-15, 61.00000000546238255, 32.49999999999999289 ) ) ;
#26871 = CARTESIAN_POINT ( 'NONE',  ( -7.570916362186215665, 3.400000000000014122, 23.30088464923126423 ) ) ;
#26872 = CARTESIAN_POINT ( 'NONE',  ( 33.58253175000000823, 76.02500000273118985, 10.91162601494192863 ) ) ;
#26873 = CARTESIAN_POINT ( 'NONE',  ( 28.01184896238290278, 20.02083333333332860, -7.505752307973347470 ) ) ;
#26874 = CARTESIAN_POINT ( 'NONE',  ( -24.50000000000001066, 9.100000000000004974, 7.960532557706201828 ) ) ;
#26875 = CARTESIAN_POINT ( 'NONE',  ( 6.486482029760649416E-15, 9.875000002731187720, 35.31076352940723240 ) ) ;
#26876 = CARTESIAN_POINT ( 'NONE',  ( -2.162160676586881955E-15, 16.62500000273120548, -35.31076352940723240 ) ) ;
#26877 = CARTESIAN_POINT ( 'NONE',  ( 8.601468415847520532, 79.57500000273120122, 11.83890561707634603 ) ) ;
#26878 = CARTESIAN_POINT ( 'NONE',  ( 2.375766604868043252, 77.69874572391549350, -14.99999999999999822 ) ) ;
#26879 = CARTESIAN_POINT ( 'NONE',  ( 28.02196122052058413, 32.61940999907601224, 7.468012846824272799 ) ) ;
#26880 = CARTESIAN_POINT ( 'NONE',  ( 2.897257156509938333E-15, 80.50000000000000000, 15.77193336357400710 ) ) ;
#26881 = CARTESIAN_POINT ( 'NONE',  ( -20.50609665440969209, 48.95312500000000000, 20.50609665441005092 ) ) ;
#26882 = CARTESIAN_POINT ( 'NONE',  ( 7.313012447739250820E-14, 11.49999999999999112, 24.50000000000000000 ) ) ;
#26883 = CARTESIAN_POINT ( 'NONE',  ( 26.29305231718579350, 70.79999999999999716, 19.10302069950537529 ) ) ;
#26884 = CARTESIAN_POINT ( 'NONE',  ( -0.04044903255042732459, 65.99180583240935505, -27.95245687107223986 ) ) ;
#26885 = CARTESIAN_POINT ( 'NONE',  ( -33.58253175000000113, 47.02500000273116854, -10.91162601494193218 ) ) ;
#26886 = CARTESIAN_POINT ( 'NONE',  ( -11.25946833292375793, 78.67500000273119554, -8.180482586598733619 ) ) ;
#26887 = CARTESIAN_POINT ( 'NONE',  ( 27.16883889988624290, 48.17500000273118843, 19.73931689729373673 ) ) ;
#26888 = CARTESIAN_POINT ( 'NONE',  ( 27.16883889988623935, 32.57500000273119412, -19.73931689729374384 ) ) ;
#26889 = CARTESIAN_POINT ( 'NONE',  ( 9.103978835402296355, 16.99999999999999645, 22.05180196682243832 ) ) ;
#26890 = CARTESIAN_POINT ( 'NONE',  ( 26.07999730980490227, 23.74479166666666430, 6.988114217767821046 ) ) ;
#26891 = CARTESIAN_POINT ( 'NONE',  ( -9.270509831248419985, 80.30000000000002558, 12.75976212528060039 ) ) ;
#26892 = CARTESIAN_POINT ( 'NONE',  ( -26.29305231718578995, 70.20000000000000284, 19.10302069950538595 ) ) ;
#26893 = CARTESIAN_POINT ( 'NONE',  ( -10.37757302488624411, 8.725000002731173154, -31.93888565452638417 ) ) ;
#26894 = CARTESIAN_POINT ( 'NONE',  ( 18.94512977948576093, 4.824999997268819563, -13.76444248337722875 ) ) ;
#26895 = CYLINDRICAL_SURFACE ( 'NONE', #2881, 15.00000000000000000 ) ;
#26896 = CARTESIAN_POINT ( 'NONE',  ( -24.22776226481266448, 24.16888916574269075, -13.94119854578892514 ) ) ;
#26897 = CARTESIAN_POINT ( 'NONE',  ( -4.635254915624211769, 75.85000000546237686, -14.26584774442730286 ) ) ;
#26898 = CARTESIAN_POINT ( 'NONE',  ( -2.162160676586882350E-15, 18.62500000273117351, -35.31076352940722529 ) ) ;
#26899 = CARTESIAN_POINT ( 'NONE',  ( -7.236395654485763274, 8.524999997268800200, 22.27133577429736633 ) ) ;
#26900 = CARTESIAN_POINT ( 'NONE',  ( -24.20753774853756823, 56.54427083333332149, -13.97622843553588723 ) ) ;
#26901 = VERTEX_POINT ( 'NONE', #14334 ) ;
#26902 = CARTESIAN_POINT ( 'NONE',  ( 20.75514604977249178, 57.82500000273118701, 28.56700777964553950 ) ) ;
#26903 = EDGE_LOOP ( 'NONE', ( #22033, #9987, #18823, #33179 ) ) ;
#26904 = CARTESIAN_POINT ( 'NONE',  ( 26.00068869287367335, 20.45052083333332504, 15.01150461594596308 ) ) ;
#26905 = CARTESIAN_POINT ( 'NONE',  ( 15.04653450569292872, 21.02902750092397710, -25.98046417659857710 ) ) ;
#26906 = CARTESIAN_POINT ( 'NONE',  ( -5.147494310547640062, 10.44874571845314293, 32.49999999999992895 ) ) ;
#26907 = CARTESIAN_POINT ( 'NONE',  ( 7.236395654485760609, 3.024999997268823293, -22.27133577429736633 ) ) ;
#26908 = CARTESIAN_POINT ( 'NONE',  ( 10.37757302488624767, 29.97500000273117848, 31.93888565452638417 ) ) ;
#26909 = CARTESIAN_POINT ( 'NONE',  ( -32.50000000000000000, 32.60000000546237686, 10.55989012756946366 ) ) ;
#26910 =( BOUNDED_CURVE ( )  B_SPLINE_CURVE ( 2, ( #17661, #17154, #9406, #22630, #27613, #4268, #19723, #30169, #22300, #7352, #27955, #25378, #1858 ),
 .UNSPECIFIED., .F., .T. ) 
 B_SPLINE_CURVE_WITH_KNOTS ( ( 3, 2, 2, 2, 2, 2, 3 ),
 ( 0.5705128205128204844, 0.5717948717948717618, 0.5743589743589743168, 0.5769230769230768718, 0.5794871794871795379, 0.5820512820512820928, 0.5833333333333333703 ),
 .UNSPECIFIED. ) 
 CURVE ( )  GEOMETRIC_REPRESENTATION_ITEM ( )  RATIONAL_B_SPLINE_CURVE ( ( 0.9755282581475768211, 0.9755282581475768211, 1.000000000000000000, 0.9510565162951535312, 1.000000000000000000, 0.9510565162951535312, 1.000000000000000000, 0.9510565162951535312, 1.000000000000000000, 0.9510565162951535312, 1.000000000000000000, 0.9755282581475768211, 0.9755282581475768211 ) ) 
 REPRESENTATION_ITEM ( '' )  );
#26911 = CARTESIAN_POINT ( 'NONE',  ( -10.04305231718579172, 77.60000000000000853, -30.90933677959248982 ) ) ;
#26912 = CARTESIAN_POINT ( 'NONE',  ( 5.779280353836490358E-15, 55.00000000546238965, 32.49999999999999289 ) ) ;
#26913 = CARTESIAN_POINT ( 'NONE',  ( 32.50000000000000711, 37.40000000546236691, 10.55989012756945122 ) ) ;
#26914 = CARTESIAN_POINT ( 'NONE',  ( -20.75514604977248823, 41.07500000273119412, -28.56700777964554305 ) ) ;
#26915 = FILL_AREA_STYLE_COLOUR ( '', #12287 ) ;
#26916 = CARTESIAN_POINT ( 'NONE',  ( -32.50000000000000000, 22.09999999999999787, 10.55989012756946366 ) ) ;
#26917 = CARTESIAN_POINT ( 'NONE',  ( -26.29305231718578995, 24.19999999999999929, 19.10302069950538595 ) ) ;
#26918 = VECTOR ( 'NONE', #20112, 1000.000000000000000 ) ;
#26919 = CARTESIAN_POINT ( 'NONE',  ( -19.82091636218621034, 14.80000000000000782, -14.40073868116559552 ) ) ;
#26920 = CARTESIAN_POINT ( 'NONE',  ( -27.16883889988623935, 65.32500000273117280, 19.73931689729374739 ) ) ;
#26921 = CARTESIAN_POINT ( 'NONE',  ( 33.58253175000000113, 56.37500000273118417, -4.112674001490185761E-15 ) ) ;
#26922 = CARTESIAN_POINT ( 'NONE',  ( 14.47279130897151767, 10.32499999726881335, 19.92008829642072953 ) ) ;
#26923 = CARTESIAN_POINT ( 'NONE',  ( 19.82091636218621389, 4.200000000000009059, -14.40073868116559197 ) ) ;
#26924 = CARTESIAN_POINT ( 'NONE',  ( -27.16883889988623935, 7.325000002731174575, 19.73931689729374739 ) ) ;
#26925 = CARTESIAN_POINT ( 'NONE',  ( -24.22776226481240514, 43.65923583425730925, 13.94119854578937812 ) ) ;
#26926 = CARTESIAN_POINT ( 'NONE',  ( -20.30017892146885217, 52.00000000000002132, 26.02681000244164267 ) ) ;
#26927 = CARTESIAN_POINT ( 'NONE',  ( 33.58253175000000823, 28.02500000273119340, 10.91162601494192863 ) ) ;
#26928 = VECTOR ( 'NONE', #7595, 1000.000000000000000 ) ;
#26929 = CARTESIAN_POINT ( 'NONE',  ( 32.50000000000000000, 65.10000000000000853, -10.55989012756945833 ) ) ;
#26930 = CARTESIAN_POINT ( 'NONE',  ( 4.412827539393359662E-15, -59.03347138510255832, 0.000000000000000000 ) ) ;
#26931 = CARTESIAN_POINT ( 'NONE',  ( -32.50000000000000000, 30.40000000546238823, -10.55989012756945300 ) ) ;
#26932 = CARTESIAN_POINT ( 'NONE',  ( -28.00173670424535644, 58.11420166574269075, 7.543491769121936308 ) ) ;
#26933 = CARTESIAN_POINT ( 'NONE',  ( 20.08610463437158344, 51.20000000546237828, 27.64615127144129403 ) ) ;
#26934 = CARTESIAN_POINT ( 'NONE',  ( -8.446640517145639571E-15, 78.49999999999998579, 32.49999999999999289 ) ) ;
#26935 = CARTESIAN_POINT ( 'NONE',  ( -7.579748464070165821E-14, 16.50000000000000355, -24.50000000000000000 ) ) ;
#26936 = CARTESIAN_POINT ( 'NONE',  ( -2.428612866367529427E-13, 22.74218749999999645, -27.95245687107222921 ) ) ;
#26937 = ORIENTED_EDGE ( 'NONE', *, *, #6314, .F. ) ;
#26938 = CARTESIAN_POINT ( 'NONE',  ( 27.16883889988624290, 75.92500000273120975, 19.73931689729373673 ) ) ;
#26939 = CARTESIAN_POINT ( 'NONE',  ( 15.01150461594596308, 26.46614583333332149, -26.00068869287367335 ) ) ;
#26940 = DIRECTION ( 'NONE',  ( -1.224646799147353207E-16, -1.499759782661857882E-32, 1.000000000000000000 ) ) ;
#26941 = ORIENTED_EDGE ( 'NONE', *, *, #3988, .F. ) ;
#26942 = CARTESIAN_POINT ( 'NONE',  ( 14.97647472619947351, 49.67486083425730925, 26.02091320914850314 ) ) ;
#26943 = CARTESIAN_POINT ( 'NONE',  ( 10.04305231718579705, 15.10000000546239640, 30.90933677959248982 ) ) ;
#26944 = CARTESIAN_POINT ( 'NONE',  ( -30.02300923189239512, 49.38281249999997868, 2.654126918244515359E-13 ) ) ;
#26945 = CARTESIAN_POINT ( 'NONE',  ( -20.50609665440969209, 66.14062500000000000, 20.50609665441005092 ) ) ;
#26946 = CARTESIAN_POINT ( 'NONE',  ( 10.37757302488624767, 49.97500000273119269, 31.93888565452638417 ) ) ;
#26947 = CARTESIAN_POINT ( 'NONE',  ( -26.29305231718578995, 48.70000000546237118, 19.10302069950538595 ) ) ;
#26948 = CARTESIAN_POINT ( 'NONE',  ( -13.91746824999999532, 79.27500000273117564, -4.522059556121115875 ) ) ;
#26949 = CARTESIAN_POINT ( 'NONE',  ( 20.75514604977249178, 37.82500000273117280, 28.56700777964553950 ) ) ;
#26950 = FACE_OUTER_BOUND ( 'NONE', #10411, .T. ) ;
#26951 = VECTOR ( 'NONE', #15714, 1000.000000000000000 ) ;
#26952 = CARTESIAN_POINT ( 'NONE',  ( 33.58253175000000823, 60.27500000273116143, 10.91162601494192863 ) ) ;
#26953 = CARTESIAN_POINT ( 'NONE',  ( 6.277390505771533514E-15, 40.50000000000000711, 34.17252228774368916 ) ) ;
#26954 = CARTESIAN_POINT ( 'NONE',  ( -23.41746825000000598, 13.72499999726882258, 7.608796670333726198 ) ) ;
#26955 = CARTESIAN_POINT ( 'NONE',  ( -20.75514604977248112, 3.675000002731179549, 28.56700777964554661 ) ) ;
#26956 = CARTESIAN_POINT ( 'NONE',  ( 20.08610463437158344, 12.70000000000000639, 27.64615127144129403 ) ) ;
#26957 = CARTESIAN_POINT ( 'NONE',  ( 4.300734207923761154, 71.97500000273119269, 13.23629886949340495 ) ) ;
#26958 = CARTESIAN_POINT ( 'NONE',  ( 33.58253175000000823, 72.27500000273118985, 10.91162601494192685 ) ) ;
#26959 = DIRECTION ( 'NONE',  ( -0.000000000000000000, -1.000000000000000000, -0.000000000000000000 ) ) ;
#26960 = CARTESIAN_POINT ( 'NONE',  ( 27.16883889988623935, 70.57500000273118701, -19.73931689729374384 ) ) ;
#26961 = ORIENTED_EDGE ( 'NONE', *, *, #18507, .F. ) ;
#26962 = CARTESIAN_POINT ( 'NONE',  ( 7.570916362186213000, 2.149999994537632464, -23.30088464923126423 ) ) ;
#26963 = CARTESIAN_POINT ( 'NONE',  ( -19.06425588902591173, 10.00038166759064140, -19.11951029504763611 ) ) ;
#26964 = DIRECTION ( 'NONE',  ( -1.224646799147353454E-16, 1.000000000000000000, -0.000000000000000000 ) ) ;
#26965 = CARTESIAN_POINT ( 'NONE',  ( -10.37757302488624411, 46.72500000273120691, -31.93888565452638417 ) ) ;
#26966 = CARTESIAN_POINT ( 'NONE',  ( 27.16883889988623935, 8.575000002731188786, -19.73931689729374384 ) ) ;
#26967 = CARTESIAN_POINT ( 'NONE',  ( 10.37757302488624056, 62.77500000273118985, -31.93888565452638417 ) ) ;
#26968 = CARTESIAN_POINT ( 'NONE',  ( -13.97622843553588901, 48.80989583333332860, 24.20753774853756823 ) ) ;
#26969 = CARTESIAN_POINT ( 'NONE',  ( 26.02091320914851025, 35.06548583425731636, -14.97647472619946463 ) ) ;
#26970 = CARTESIAN_POINT ( 'NONE',  ( -0.04044903255044120238, 31.61680583240936215, -30.02300923189239867 ) ) ;
#26971 = CARTESIAN_POINT ( 'NONE',  ( 26.29305231718578995, 69.70000000546238539, -19.10302069950538240 ) ) ;
#26972 = ADVANCED_FACE ( 'NONE', ( #17422 ), #33184, .F. ) ;
#26973 = CARTESIAN_POINT ( 'NONE',  ( -4.300734207923759378, 76.47500000273116427, -13.23629886949340495 ) ) ;
#26974 = CARTESIAN_POINT ( 'NONE',  ( -26.06988505166722803, 54.67670166574269075, 7.025853678916877953 ) ) ;
#26975 = CARTESIAN_POINT ( 'NONE',  ( -14.47279130897152122, 15.92499999726881121, 19.92008829642072243 ) ) ;
#26976 = EDGE_CURVE ( 'NONE', #28845, #24251, #9512, .T. ) ;
#26977 = CARTESIAN_POINT ( 'NONE',  ( 2.067204126564591252E-14, 4.249999994537631665, -24.50000000000000000 ) ) ;
#26978 = EDGE_LOOP ( 'NONE', ( #28554, #13662, #27982, #2162 ) ) ;
#26979 = CARTESIAN_POINT ( 'NONE',  ( -20.75514604977248112, 47.67500000273118843, 28.56700777964554661 ) ) ;
#26980 = CARTESIAN_POINT ( 'NONE',  ( 3.000384657911015469E-15, 16.99999999999998579, 24.50000000000000000 ) ) ;
#26981 = CARTESIAN_POINT ( 'NONE',  ( 14.01125832528286352, 51.96652750092398065, -24.18731323226246843 ) ) ;
#26982 = CARTESIAN_POINT ( 'NONE',  ( 27.16883889988624290, 70.17500000273119554, 19.73931689729373673 ) ) ;
#26983 = ORIENTED_EDGE ( 'NONE', *, *, #27320, .F. ) ;
#26984 = CARTESIAN_POINT ( 'NONE',  ( -10.37757302488624411, 14.72500000273117848, -31.93888565452638417 ) ) ;
#26985 = ADVANCED_FACE ( 'NONE', ( #17250 ), #14385, .F. ) ;
#26986 = CARTESIAN_POINT ( 'NONE',  ( 15.01150461594643204, 20.73697916666666075, 26.00068869287340334 ) ) ;
#26987 = VERTEX_POINT ( 'NONE', #28051 ) ;
#26988 = ORIENTED_EDGE ( 'NONE', *, *, #32828, .T. ) ;
#26989 = CARTESIAN_POINT ( 'NONE',  ( -7.570916362186210335, 2.349999994537638415, -23.30088464923126779 ) ) ;
#26990 = CARTESIAN_POINT ( 'NONE',  ( 20.75514604977248467, 54.42500000273117422, -28.56700777964554305 ) ) ;
#26991 = CARTESIAN_POINT ( 'NONE',  ( 7.505752307973351023, 55.25520833333333570, 28.01184896238290278 ) ) ;
#26992 = CARTESIAN_POINT ( 'NONE',  ( 26.29305231718579350, 9.300000005462383257, 19.10302069950537529 ) ) ;
#26993 = VECTOR ( 'NONE', #23395, 999.9999999999998863 ) ;
#26994 = FACE_OUTER_BOUND ( 'NONE', #31134, .T. ) ;
#26995 = CARTESIAN_POINT ( 'NONE',  ( -23.41746824999999887, 8.024999997268800200, -7.608796670333730638 ) ) ;
#26996 = CARTESIAN_POINT ( 'NONE',  ( -20.75514604977248112, 21.67500000273119554, 28.56700777964554661 ) ) ;
#26997 = PRESENTATION_STYLE_ASSIGNMENT (( #29727 ) ) ;
#26998 = CARTESIAN_POINT ( 'NONE',  ( 24.22776226481265383, 15.57513916574268720, 13.94119854578893580 ) ) ;
#26999 = CARTESIAN_POINT ( 'NONE',  ( -11.25946833292375793, 78.67500000273119554, -8.180482586598733619 ) ) ;
#27000 = DIRECTION ( 'NONE',  ( 1.224646799147353454E-16, -1.000000000000000000, 0.000000000000000000 ) ) ;
#27001 = CARTESIAN_POINT ( 'NONE',  ( -32.50000000000000000, 7.900000000000012790, -10.55989012756945478 ) ) ;
#27002 = ORIENTED_EDGE ( 'NONE', *, *, #29131, .F. ) ;
#27003 = CARTESIAN_POINT ( 'NONE',  ( 7.236395654485760609, 3.524999997268824181, -22.27133577429736633 ) ) ;
#27004 = CARTESIAN_POINT ( 'NONE',  ( -11.25946833292375793, 76.67500000273119554, -8.180482586598733619 ) ) ;
#27005 = CARTESIAN_POINT ( 'NONE',  ( 13.97622843553589966, 43.65364583333332860, -24.20753774853756113 ) ) ;
#27006 =( BOUNDED_CURVE ( )  B_SPLINE_CURVE ( 2, ( #32889, #9388, #30665, #22788, #30325, #6821, #17303, #14726, #1838, #12318, #33241, #9739, #20225 ),
 .UNSPECIFIED., .F., .T. ) 
 B_SPLINE_CURVE_WITH_KNOTS ( ( 3, 2, 2, 2, 2, 2, 3 ),
 ( 0.8782051282051281937, 0.8794871794871794712, 0.8820512820512820262, 0.8846153846153845812, 0.8871794871794871362, 0.8897435897435896912, 0.8910256410256410797 ),
 .UNSPECIFIED. ) 
 CURVE ( )  GEOMETRIC_REPRESENTATION_ITEM ( )  RATIONAL_B_SPLINE_CURVE ( ( 0.9755282581475768211, 0.9755282581475768211, 1.000000000000000000, 0.9510565162951535312, 1.000000000000000000, 0.9510565162951535312, 1.000000000000000000, 0.9510565162951535312, 1.000000000000000000, 0.9510565162951535312, 1.000000000000000000, 0.9755282581475757109, 0.9755282581475768211 ) ) 
 REPRESENTATION_ITEM ( '' )  );
#27007 = CARTESIAN_POINT ( 'NONE',  ( 27.16883889988624290, 25.92500000273118133, 19.73931689729373673 ) ) ;
#27008 = CARTESIAN_POINT ( 'NONE',  ( 33.58253175000000113, 68.12500000273118417, -4.112674001490185761E-15 ) ) ;
#27009 = CARTESIAN_POINT ( 'NONE',  ( -33.58253175000000113, 33.27500000273120406, -10.91162601494193218 ) ) ;
#27010 = CARTESIAN_POINT ( 'NONE',  ( 20.75514604977249178, 18.07500000273119056, 28.56700777964553950 ) ) ;
#27011 = CARTESIAN_POINT ( 'NONE',  ( -20.75514604977248823, 7.075000002731187898, -28.56700777964554305 ) ) ;
#27012 = CARTESIAN_POINT ( 'NONE',  ( -24.18731323226248264, 64.85715250092397355, -14.01125832528284931 ) ) ;
#27013 = CARTESIAN_POINT ( 'NONE',  ( 27.16883889988624290, 71.92500000273119554, 19.73931689729373673 ) ) ;
#27014 = CARTESIAN_POINT ( 'NONE',  ( 26.00068869287367335, 54.82552083333331439, 15.01150461594596308 ) ) ;
#27015 = DIRECTION ( 'NONE',  ( -0.8660254037844363761, -0.5000000000000038858, 1.060575238724904326E-16 ) ) ;
#27016 = CARTESIAN_POINT ( 'NONE',  ( -8.601468415847515203, 75.67500000273119554, 11.83890561707634959 ) ) ;
#27017 = AXIS2_PLACEMENT_3D ( 'NONE', #16100, #15927, #10934 ) ;
#27018 = CARTESIAN_POINT ( 'NONE',  ( -10.04305231718578462, 50.39999999999998437, 30.90933677959249337 ) ) ;
#27019 = CARTESIAN_POINT ( 'NONE',  ( -9.270509831248419985, 72.55000000546236549, 12.75976212528060039 ) ) ;
#27020 = CARTESIAN_POINT ( 'NONE',  ( -20.75514604977248112, 57.42500000273119554, 28.56700777964554661 ) ) ;
#27021 = VECTOR ( 'NONE', #25821, 1000.000000000000000 ) ;
#27022 = CARTESIAN_POINT ( 'NONE',  ( 14.47279130897151589, 16.82499999726881512, 19.92008829642072953 ) ) ;
#27023 = VERTEX_POINT ( 'NONE', #9331 ) ;
#27024 = CARTESIAN_POINT ( 'NONE',  ( 10.37757302488624056, 68.77500000273118985, -31.93888565452638417 ) ) ;
#27025 = CARTESIAN_POINT ( 'NONE',  ( -2.162160676586882350E-15, 2.625000002731183280, -35.31076352940722529 ) ) ;
#27026 = CARTESIAN_POINT ( 'NONE',  ( 18.94512977948575738, 4.424999997268807661, 13.76444248337723408 ) ) ;
#27027 = CARTESIAN_POINT ( 'NONE',  ( -26.06988505166735237, 26.90142333425731280, -7.025853678916388567 ) ) ;
#27028 = ORIENTED_EDGE ( 'NONE', *, *, #18187, .F. ) ;
#27029 = CARTESIAN_POINT ( 'NONE',  ( 10.37757302488624056, 34.52500000273118985, -31.93888565452638417 ) ) ;
#27030 = CARTESIAN_POINT ( 'NONE',  ( -1.778240108872766143E-15, 68.00000000546238255, -32.49999999999999289 ) ) ;
#27031 = VERTEX_POINT ( 'NONE', #11920 ) ;
#27032 = CARTESIAN_POINT ( 'NONE',  ( 15.01150461594643204, 51.67447916666665719, 26.00068869287340334 ) ) ;
#27033 = CARTESIAN_POINT ( 'NONE',  ( 27.16883889988623935, 62.57500000273119412, -19.73931689729374384 ) ) ;
#27034 = CARTESIAN_POINT ( 'NONE',  ( -1.778240108872766143E-15, 70.00000000546238255, -32.49999999999999289 ) ) ;
#27035 = CARTESIAN_POINT ( 'NONE',  ( -27.16883889988623935, 71.32500000273117280, 19.73931689729374739 ) ) ;
#27036 = CARTESIAN_POINT ( 'NONE',  ( -7.505752307972844761, 28.04166666666666075, 28.01184896238304134 ) ) ;
#27037 = CARTESIAN_POINT ( 'NONE',  ( -19.82091636218621389, 5.200000000000009948, 14.40073868116558842 ) ) ;
#27038 = CARTESIAN_POINT ( 'NONE',  ( 20.75514604977249178, 8.075000002731185234, 28.56700777964553950 ) ) ;
#27039 = EDGE_CURVE ( 'NONE', #23106, #12231, #31385, .T. ) ;
#27040 = CARTESIAN_POINT ( 'NONE',  ( -20.75514604977248112, 17.42500000273117777, 28.56700777964554661 ) ) ;
#27041 = CARTESIAN_POINT ( 'NONE',  ( 11.25946833292375793, 80.07500000273121543, -8.180482586598735395 ) ) ;
#27042 = CARTESIAN_POINT ( 'NONE',  ( 15.00000000000000355, 77.15000000546235981, 4.873795443493592394 ) ) ;
#27043 = CARTESIAN_POINT ( 'NONE',  ( 7.543491769121922985, 43.50482666574268364, 28.00173670424535644 ) ) ;
#27044 = CARTESIAN_POINT ( 'NONE',  ( -12.13525491562421088, 79.80000000000001137, -8.816778784387096835 ) ) ;
#27045 = CARTESIAN_POINT ( 'NONE',  ( 15.01150461594643382, 51.67447916666665719, 26.00068869287340334 ) ) ;
#27046 = AXIS2_PLACEMENT_3D ( 'NONE', #33786, #10784, #30855 ) ;
#27047 = CARTESIAN_POINT ( 'NONE',  ( 32.50000000000000711, 53.40000000546238113, 10.55989012756945122 ) ) ;
#27048 = CARTESIAN_POINT ( 'NONE',  ( -10.04305231718579172, 38.10000000546237686, -30.90933677959248982 ) ) ;
#27049 = CARTESIAN_POINT ( 'NONE',  ( -6.988114217768288228, 12.28645833333333037, -26.07999730980477437 ) ) ;
#27050 = CARTESIAN_POINT ( 'NONE',  ( 6.486482029760649416E-15, 43.62500000273116285, 35.31076352940723240 ) ) ;
#27051 = CARTESIAN_POINT ( 'NONE',  ( -11.25946833292375793, 77.07500000273121543, 8.180482586598737171 ) ) ;
#27052 = CARTESIAN_POINT ( 'NONE',  ( 33.58253175000000113, 46.37500000273119127, -4.112674001490185761E-15 ) ) ;
#27053 = CARTESIAN_POINT ( 'NONE',  ( 33.58253175000000113, 28.47500000273117848, -10.91162601494193574 ) ) ;
#27054 = CARTESIAN_POINT ( 'NONE',  ( -4.223320258572819786E-15, 17.50000000000000000, 24.50000000000000000 ) ) ;
#27055 = CARTESIAN_POINT ( 'NONE',  ( -26.07999730980477437, 21.73958333333332860, 6.988114217768305103 ) ) ;
#27056 = CARTESIAN_POINT ( 'NONE',  ( -4.635254915624211769, 79.85000000546239107, -14.26584774442730286 ) ) ;
#27057 = CARTESIAN_POINT ( 'NONE',  ( -15.00000000000000000, 76.00000000000001421, 0.000000000000000000 ) ) ;
#27058 = CARTESIAN_POINT ( 'NONE',  ( 10.04305231718579705, 70.59999999999998010, 30.90933677959248982 ) ) ;
#27059 = CARTESIAN_POINT ( 'NONE',  ( -20.75514604977248112, 7.425000002731191984, 28.56700777964554661 ) ) ;
#27060 = CARTESIAN_POINT ( 'NONE',  ( 23.41746824999999887, 6.524999997268818852, 7.608796670333735079 ) ) ;
#27061 = CARTESIAN_POINT ( 'NONE',  ( -26.29305231718579350, 52.30000000546236549, -19.10302069950537884 ) ) ;
#27062 = CARTESIAN_POINT ( 'NONE',  ( -26.09010956794245217, 27.46315999907601935, -6.950374756619243755 ) ) ;
#27063 = CARTESIAN_POINT ( 'NONE',  ( -3.880418787951142701, 13.44874571845315536, 24.49999999999999645 ) ) ;
#27064 = CARTESIAN_POINT ( 'NONE',  ( -33.58253175000000113, 19.22500000273118204, 10.91162601494193929 ) ) ;
#27065 = CARTESIAN_POINT ( 'NONE',  ( 23.41746824999999887, 7.124999997268815832, 0.000000000000000000 ) ) ;
#27066 = CLOSED_SHELL ( 'NONE', ( #19856, #8035, #29083, #31783, #6974, #30118 ) ) ;
#27067 = CARTESIAN_POINT ( 'NONE',  ( 6.988114217768294445, 51.81770833333332860, 26.07999730980477437 ) ) ;
#27068 = AXIS2_PLACEMENT_3D ( 'NONE', #30451, #30621, #17774 ) ;
#27069 = EDGE_LOOP ( 'NONE', ( #516, #12939, #32872, #13113 ) ) ;
#27070 = CARTESIAN_POINT ( 'NONE',  ( 27.16883889988623935, 58.32500000273120833, -19.73931689729374384 ) ) ;
#27071 = ORIENTED_EDGE ( 'NONE', *, *, #18882, .T. ) ;
#27072 = CARTESIAN_POINT ( 'NONE',  ( 28.01184896238304134, 20.30729166666666430, 7.505752307972846538 ) ) ;
#27073 = CARTESIAN_POINT ( 'NONE',  ( -15.04653450569291984, 26.18527750092397710, 25.98046417659859486 ) ) ;
#27074 = CARTESIAN_POINT ( 'NONE',  ( 10.04305231718578817, 39.39999999999999147, -30.90933677959249337 ) ) ;
#27075 = CARTESIAN_POINT ( 'NONE',  ( -4.732186688966233175E-15, 13.24999999453763166, 25.76082449383753925 ) ) ;
#27076 = CARTESIAN_POINT ( 'NONE',  ( 14.47279130897151589, 8.324999997268818674, 19.92008829642072953 ) ) ;
#27077 = CARTESIAN_POINT ( 'NONE',  ( 10.37757302488624767, 25.97500000273117493, 31.93888565452638417 ) ) ;
#27078 = CARTESIAN_POINT ( 'NONE',  ( -10.04305231718578462, 30.90000000546239178, 30.90933677959249337 ) ) ;
#27079 = EDGE_CURVE ( 'NONE', #22980, #20845, #6267, .T. ) ;
#27080 = CARTESIAN_POINT ( 'NONE',  ( -10.04305231718579172, 73.59999999999999432, -30.90933677959248982 ) ) ;
#27081 = CARTESIAN_POINT ( 'NONE',  ( 10.04305231718578817, 53.40000000000000568, -30.90933677959249337 ) ) ;
#27082 = CARTESIAN_POINT ( 'NONE',  ( 10.04305231718578817, 37.90000000546236691, -30.90933677959249337 ) ) ;
#27083 = CARTESIAN_POINT ( 'NONE',  ( 28.02196122052045268, 52.39621500092398065, -7.468012846824774620 ) ) ;
#27084 = CARTESIAN_POINT ( 'NONE',  ( 20.75514604977248467, 44.67500000273118843, -28.56700777964554305 ) ) ;
#27085 = ADVANCED_FACE ( 'NONE', ( #6939 ), #27883, .T. ) ;
#27086 = CARTESIAN_POINT ( 'NONE',  ( 23.41746824999999887, 11.12499999726881938, 0.000000000000000000 ) ) ;
#27087 = CARTESIAN_POINT ( 'NONE',  ( 32.50000000000000711, 20.90000000000000924, 10.55989012756945122 ) ) ;
#27088 = CARTESIAN_POINT ( 'NONE',  ( 7.570916362186207671, 13.60000000000000142, 23.30088464923126779 ) ) ;
#27089 = CARTESIAN_POINT ( 'NONE',  ( -26.06988505166722803, 37.48920166574269075, 7.025853678916877953 ) ) ;
#27090 = CARTESIAN_POINT ( 'NONE',  ( -10.37757302488624411, 60.72500000273117848, -31.93888565452638417 ) ) ;
#27091 = CARTESIAN_POINT ( 'NONE',  ( -27.16883889988623935, 51.57500000273118701, 19.73931689729374739 ) ) ;
#27092 = CARTESIAN_POINT ( 'NONE',  ( -7.236395654485763274, 8.024999997268828622, 22.27133577429736633 ) ) ;
#27093 = CARTESIAN_POINT ( 'NONE',  ( 2.067204126564591252E-14, 4.249999994537631665, -24.50000000000000000 ) ) ;
#27094 = CARTESIAN_POINT ( 'NONE',  ( -10.37757302488623701, 3.525000002731204507, 31.93888565452638417 ) ) ;
#27095 = CARTESIAN_POINT ( 'NONE',  ( 24.22776226481241224, 38.50298583425730925, -13.94119854578936923 ) ) ;
#27096 = FACE_OUTER_BOUND ( 'NONE', #13193, .T. ) ;
#27097 = CARTESIAN_POINT ( 'NONE',  ( -11.54700538379251995, 96.00000000000002842, -19.99999999999999645 ) ) ;
#27098 = PRODUCT_DEFINITION_CONTEXT ( 'detailed design', #31353, 'design' ) ;
#27099 = CARTESIAN_POINT ( 'NONE',  ( -33.58253175000000113, 31.02500000273118630, -10.91162601494193218 ) ) ;
#27100 = CARTESIAN_POINT ( 'NONE',  ( 20.08610463437158344, 56.69999999999998153, 27.64615127144129403 ) ) ;
#27101 = CARTESIAN_POINT ( 'NONE',  ( -26.29305231718579350, 58.30000000546237260, -19.10302069950537884 ) ) ;
#27102 = CARTESIAN_POINT ( 'NONE',  ( 7.570916362186213000, 14.39999999999999680, -23.30088464923126423 ) ) ;
#27103 = CARTESIAN_POINT ( 'NONE',  ( -0.04044903255044120238, 55.67930583240935505, -30.02300923189239867 ) ) ;
#27104 = CARTESIAN_POINT ( 'NONE',  ( 10.04305231718579705, 47.10000000546236976, 30.90933677959248982 ) ) ;
#27105 = CARTESIAN_POINT ( 'NONE',  ( 11.25946833292375793, 72.57500000273120122, -8.180482586598735395 ) ) ;
#27106 = DIRECTION ( 'NONE',  ( 0.000000000000000000, 0.000000000000000000, -1.000000000000000000 ) ) ;
#27107 = CARTESIAN_POINT ( 'NONE',  ( -6.988114217768288228, 22.59895833333332860, -26.07999730980477437 ) ) ;
#27108 = VERTEX_POINT ( 'NONE', #33363 ) ;
#27109 = CARTESIAN_POINT ( 'NONE',  ( -33.58253175000000113, 77.02500000273118985, -10.91162601494193218 ) ) ;
#27110 = CARTESIAN_POINT ( 'NONE',  ( 7.505752307973351023, 27.75520833333332860, 28.01184896238290278 ) ) ;
#27111 =( GEOMETRIC_REPRESENTATION_CONTEXT ( 3 ) GLOBAL_UNCERTAINTY_ASSIGNED_CONTEXT ( ( #10988 ) ) GLOBAL_UNIT_ASSIGNED_CONTEXT ( ( #15818, #32081, #16652 ) ) REPRESENTATION_CONTEXT ( 'NONE', 'WORKASPACE' ) );
#27112 =( BOUNDED_CURVE ( )  B_SPLINE_CURVE ( 2, ( #762, #13986, #26526, #27019, #3515, #31662, #24448, #18978, #5757, #21720, #21549, #31995, #3018 ),
 .UNSPECIFIED., .F., .T. ) 
 B_SPLINE_CURVE_WITH_KNOTS ( ( 3, 2, 2, 2, 2, 2, 3 ),
 ( 0.7500000000000000000, 0.7600000000000000089, 0.7800000000000000266, 0.8000000000000000444, 0.8199999999999999512, 0.8399999999999999689, 0.8499999999999999778 ),
 .UNSPECIFIED. ) 
 CURVE ( )  GEOMETRIC_REPRESENTATION_ITEM ( )  RATIONAL_B_SPLINE_CURVE ( ( 0.9755282581475768211, 0.9755282581475768211, 1.000000000000000000, 0.9510565162951535312, 1.000000000000000000, 0.9510565162951535312, 1.000000000000000000, 0.9510565162951535312, 1.000000000000000000, 0.9510565162951535312, 1.000000000000000000, 0.9755282581475768211, 0.9755282581475768211 ) ) 
 REPRESENTATION_ITEM ( '' )  );
#27113 = DIRECTION ( 'NONE',  ( 0.000000000000000000, 1.000000000000000000, 0.000000000000000000 ) ) ;
#27114 = ORIENTED_EDGE ( 'NONE', *, *, #4908, .T. ) ;
#27115 = CARTESIAN_POINT ( 'NONE',  ( -7.543491769121417612, 53.54204833425730925, 28.00173670424549499 ) ) ;
#27116 = CARTESIAN_POINT ( 'NONE',  ( 26.29305231718579350, 11.30000000546237082, 19.10302069950537529 ) ) ;
#27117 = CARTESIAN_POINT ( 'NONE',  ( 7.505752307973351023, 62.13020833333334281, 28.01184896238290278 ) ) ;
#27118 = CARTESIAN_POINT ( 'NONE',  ( -26.29305231718578995, 46.70000000546237118, 19.10302069950538595 ) ) ;
#27119 = CARTESIAN_POINT ( 'NONE',  ( -33.58253175000000113, 45.27500000273116854, -10.91162601494193218 ) ) ;
#27120 = CARTESIAN_POINT ( 'NONE',  ( 32.50000000000000000, 47.50000000546239676, -3.980102097228898626E-15 ) ) ;
#27121 = CARTESIAN_POINT ( 'NONE',  ( 15.00000000000000000, 81.09999999999999432, -4.873795443493596835 ) ) ;
#27122 = CARTESIAN_POINT ( 'NONE',  ( -2.162160676586881955E-15, 36.62500000273119127, -35.31076352940723240 ) ) ;
#27123 = CARTESIAN_POINT ( 'NONE',  ( -5.147494310547478413, 62.94874572391552192, 32.49999999999998579 ) ) ;
#27124 = CARTESIAN_POINT ( 'NONE',  ( 27.16883889988623935, 64.57500000273120122, -19.73931689729374384 ) ) ;
#27125 = CARTESIAN_POINT ( 'NONE',  ( 20.08610463437158344, 32.69999999999998863, 27.64615127144129403 ) ) ;
#27126 = CARTESIAN_POINT ( 'NONE',  ( -26.29305231718579350, 37.79999999999999716, -19.10302069950537884 ) ) ;
#27127 = CARTESIAN_POINT ( 'NONE',  ( -23.41746825000000598, 11.72499999726880127, 7.608796670333726198 ) ) ;
#27128 = CARTESIAN_POINT ( 'NONE',  ( 6.486482029760649416E-15, 1.875000002731177728, 35.31076352940723240 ) ) ;
#27129 = DIRECTION ( 'NONE',  ( 0.000000000000000000, 0.000000000000000000, 1.000000000000000000 ) ) ;
#27130 = CARTESIAN_POINT ( 'NONE',  ( 33.58253175000000113, 72.37500000273116996, -4.112674001490185761E-15 ) ) ;
#27131 = CARTESIAN_POINT ( 'NONE',  ( -24.50000000000000000, 18.74999999453763522, -3.000384657911015469E-15 ) ) ;
#27132 = CARTESIAN_POINT ( 'NONE',  ( 33.58253175000000823, 70.27500000273118985, 10.91162601494192863 ) ) ;
#27133 = ORIENTED_EDGE ( 'NONE', *, *, #5804, .T. ) ;
#27134 = CARTESIAN_POINT ( 'NONE',  ( 7.570916362186207671, 5.349999994537613546, 23.30088464923126779 ) ) ;
#27135 = CIRCLE ( 'NONE', #9593, 1.999999999999993117 ) ;
#27136 = CARTESIAN_POINT ( 'NONE',  ( 13.94119854578937812, 15.29986083425731280, 24.22776226481240514 ) ) ;
#27137 = CARTESIAN_POINT ( 'NONE',  ( 4.635254915624212657, 74.59999999999999432, 14.26584774442730286 ) ) ;
#27138 = CARTESIAN_POINT ( 'NONE',  ( 33.58253175000000823, 48.02500000273119696, 10.91162601494192863 ) ) ;
#27139 = CARTESIAN_POINT ( 'NONE',  ( 27.16883889988624290, 8.175000002731177773, 19.73931689729373673 ) ) ;
#27140 = CARTESIAN_POINT ( 'NONE',  ( 10.37757302488624767, 61.97500000273119269, 31.93888565452638417 ) ) ;
#27141 = CARTESIAN_POINT ( 'NONE',  ( -19.09188309203694445, 46.37500000000000000, -19.09188309203661049 ) ) ;
#27142 = CARTESIAN_POINT ( 'NONE',  ( -0.04044903254990864921, 39.64881916759063074, 30.02300923189239867 ) ) ;
#27143 = CARTESIAN_POINT ( 'NONE',  ( -20.53372385742107653, 24.31211833240934794, -20.47846945139867003 ) ) ;
#27144 = CARTESIAN_POINT ( 'NONE',  ( -32.50000000000000000, 68.40000000546237402, -10.55989012756945478 ) ) ;
#27145 = ADVANCED_FACE ( 'NONE', ( #9859 ), #30786, .F. ) ;
#27146 = DIRECTION ( 'NONE',  ( 0.000000000000000000, 1.000000000000000000, 0.000000000000000000 ) ) ;
#27147 = CARTESIAN_POINT ( 'NONE',  ( 27.95245687107223276, 59.97618083240934794, -0.04044903255042905932 ) ) ;
#27148 = CARTESIAN_POINT ( 'NONE',  ( -14.47279130897151589, 17.32499999726879381, -19.92008829642072598 ) ) ;
#27149 = CARTESIAN_POINT ( 'NONE',  ( -24.50000000000000711, 17.10000000000001208, 7.960532557706201828 ) ) ;
#27150 = ORIENTED_EDGE ( 'NONE', *, *, #21677, .F. ) ;
#27151 = CARTESIAN_POINT ( 'NONE',  ( -33.58253175000000113, 45.27500000273116854, -10.91162601494193218 ) ) ;
#27152 = CARTESIAN_POINT ( 'NONE',  ( -14.47279130897151767, 3.824999997268816454, -19.92008829642072598 ) ) ;
#27153 = CARTESIAN_POINT ( 'NONE',  ( 19.11951029504763611, 48.67225666759065206, -19.06425588902591173 ) ) ;
#27154 = CARTESIAN_POINT ( 'NONE',  ( -10.04305231718579172, 28.10000000546238041, -30.90933677959248982 ) ) ;
#27155 = ORIENTED_EDGE ( 'NONE', *, *, #2025, .F. ) ;
#27156 = CARTESIAN_POINT ( 'NONE',  ( 33.58253175000000113, 18.22500000273118559, -10.91162601494193751 ) ) ;
#27157 = CARTESIAN_POINT ( 'NONE',  ( 7.505752307973351023, 38.06770833333332860, 28.01184896238290278 ) ) ;
#27158 = ORIENTED_EDGE ( 'NONE', *, *, #21264, .F. ) ;
#27159 = CARTESIAN_POINT ( 'NONE',  ( 0.000000000000000000, 0.000000000000000000, 0.000000000000000000 ) ) ;
#27160 = CARTESIAN_POINT ( 'NONE',  ( -33.58253175000000113, 53.12500000273118417, 0.000000000000000000 ) ) ;
#27161 = CARTESIAN_POINT ( 'NONE',  ( -20.50609665441004736, 60.12500000000000000, -20.50609665440969565 ) ) ;
#27162 = CARTESIAN_POINT ( 'NONE',  ( 6.277390505771533514E-15, 13.00000000546238255, 34.17252228774368916 ) ) ;
#27163 = CARTESIAN_POINT ( 'NONE',  ( -32.50000000000000000, 66.40000000546238823, -10.55989012756945300 ) ) ;
#27164 = CARTESIAN_POINT ( 'NONE',  ( 18.94512977948575738, 12.92499999726881654, 13.76444248337723408 ) ) ;
#27165 = CARTESIAN_POINT ( 'NONE',  ( 10.04305231718578817, 57.40000000000000568, -30.90933677959249337 ) ) ;
#27166 = CARTESIAN_POINT ( 'NONE',  ( 10.37757302488624056, 22.77500000273119340, -31.93888565452638417 ) ) ;
#27167 = LINE ( 'NONE', #6570, #10188 ) ;
#27168 = CARTESIAN_POINT ( 'NONE',  ( 0.04044903255044120238, 19.58555583240935860, 27.95245687107223276 ) ) ;
#27169 = CARTESIAN_POINT ( 'NONE',  ( -13.91746824999999532, 74.97500000273115006, 4.522059556121122093 ) ) ;
#27170 = CARTESIAN_POINT ( 'NONE',  ( 0.000000000000000000, 80.00000000000001421, 0.000000000000000000 ) ) ;
#27171 = CARTESIAN_POINT ( 'NONE',  ( -32.50000000000000000, 28.40000000546235981, -10.55989012756945300 ) ) ;
#27172 = EDGE_CURVE ( 'NONE', #23797, #24301, #4056, .T. ) ;
#27173 = CARTESIAN_POINT ( 'NONE',  ( 26.29305231718579350, 10.80000000000001847, 19.10302069950537529 ) ) ;
#27174 = ORIENTED_EDGE ( 'NONE', *, *, #1030, .F. ) ;
#27175 = CARTESIAN_POINT ( 'NONE',  ( -23.41746825000000243, 4.024999997268810858, -7.608796670333730638 ) ) ;
#27176 = CARTESIAN_POINT ( 'NONE',  ( -11.25946833292375793, 75.07500000273120122, 8.180482586598737171 ) ) ;
#27177 = CARTESIAN_POINT ( 'NONE',  ( -27.95245687107222921, 42.50781249999997868, 2.498001805406602216E-13 ) ) ;
#27178 = CARTESIAN_POINT ( 'NONE',  ( -10.37757302488623701, 15.52500000273118808, 31.93888565452638417 ) ) ;
#27179 = CARTESIAN_POINT ( 'NONE',  ( -27.16883889988623935, 67.32500000273118701, 19.73931689729374739 ) ) ;
#27180 = CARTESIAN_POINT ( 'NONE',  ( -33.58253175000000113, 29.47500000273117848, 10.91162601494193929 ) ) ;
#27181 = CARTESIAN_POINT ( 'NONE',  ( -20.75514604977248112, 17.67500000273117422, 28.56700777964554661 ) ) ;
#27182 = CARTESIAN_POINT ( 'NONE',  ( 33.58253175000000823, 6.275000002731184523, 10.91162601494192685 ) ) ;
#27183 = CARTESIAN_POINT ( 'NONE',  ( 14.01125832528286352, 62.27902750092396644, -24.18731323226246843 ) ) ;
#27184 = EDGE_CURVE ( 'NONE', #33138, #21829, #6471, .T. ) ;
#27185 = CARTESIAN_POINT ( 'NONE',  ( 20.50609665441005092, 58.40625000000000711, 20.50609665440969209 ) ) ;
#27186 = CARTESIAN_POINT ( 'NONE',  ( -13.38408793869266056, -57.48236190979495319, 1.639078045362666731E-15 ) ) ;
#27187 = CARTESIAN_POINT ( 'NONE',  ( 8.601468415847516980, 74.67500000273118133, -11.83890561707634603 ) ) ;
#27188 = CARTESIAN_POINT ( 'NONE',  ( 26.29305231718579350, 48.79999999999999716, 19.10302069950537529 ) ) ;
#27189 = CARTESIAN_POINT ( 'NONE',  ( 10.04305231718578817, 57.90000000546240244, -30.90933677959249337 ) ) ;
#27190 = CARTESIAN_POINT ( 'NONE',  ( -20.75514604977248823, 52.82500000273116569, -28.56700777964554305 ) ) ;
#27191 = APPLICATION_CONTEXT ( 'automotive_design' ) ;
#27192 = CARTESIAN_POINT ( 'NONE',  ( 1.507698388325705758E-15, 13.62499999726882827, -24.62258325217400312 ) ) ;
#27193 = ADVANCED_FACE ( 'NONE', ( #225, #7793 ), #23591, .T. ) ;
#27194 = ORIENTED_EDGE ( 'NONE', *, *, #22056, .F. ) ;
#27195 = CARTESIAN_POINT ( 'NONE',  ( -33.58253175000000113, 65.37500000273121259, 0.000000000000000000 ) ) ;
#27196 = CARTESIAN_POINT ( 'NONE',  ( 20.08610463437157279, 17.30000000000000782, -27.64615127144129758 ) ) ;
#27197 = CARTESIAN_POINT ( 'NONE',  ( -18.94512977948576093, 7.824999997268822227, 13.76444248337722698 ) ) ;
#27198 = CARTESIAN_POINT ( 'NONE',  ( -13.94119854578936923, 27.33111083425731280, -24.22776226481241224 ) ) ;
#27199 = ORIENTED_EDGE ( 'NONE', *, *, #33754, .F. ) ;
#27200 = CARTESIAN_POINT ( 'NONE',  ( 10.37757302488624056, 36.52500000273118985, -31.93888565452638417 ) ) ;
#27201 = DIRECTION ( 'NONE',  ( 0.000000000000000000, 1.000000000000000000, 0.000000000000000000 ) ) ;
#27202 = ORIENTED_EDGE ( 'NONE', *, *, #33841, .F. ) ;
#27203 = CARTESIAN_POINT ( 'NONE',  ( 15.01150461594643204, 55.11197916666664298, 26.00068869287340334 ) ) ;
#27204 = CARTESIAN_POINT ( 'NONE',  ( -33.58253175000000113, 63.47500000273117138, 10.91162601494193929 ) ) ;
#27205 = CARTESIAN_POINT ( 'NONE',  ( 26.29305231718579350, 58.80000000000000426, 19.10302069950537529 ) ) ;
#27206 = CARTESIAN_POINT ( 'NONE',  ( -33.58253175000000113, 71.02500000273118985, -10.91162601494193218 ) ) ;
#27207 = CARTESIAN_POINT ( 'NONE',  ( 7.505752307973351023, 31.19270833333333215, 28.01184896238290278 ) ) ;
#27208 = CARTESIAN_POINT ( 'NONE',  ( 7.570916362186213000, 6.399999999999988809, -23.30088464923126423 ) ) ;
#27209 = CARTESIAN_POINT ( 'NONE',  ( 10.37757302488624767, 1.975000002731180926, 31.93888565452638417 ) ) ;
#27210 = CARTESIAN_POINT ( 'NONE',  ( 33.58253175000000113, 18.12500000273117706, -4.112674001490185761E-15 ) ) ;
#27211 =( BOUNDED_CURVE ( )  B_SPLINE_CURVE ( 2, ( #22995, #33454, #9256, #9953, #20428, #19741, #4118, #14592, #32925, #30531, #26251, #31055, #25906 ),
 .UNSPECIFIED., .F., .T. ) 
 B_SPLINE_CURVE_WITH_KNOTS ( ( 3, 2, 2, 2, 2, 2, 3 ),
 ( 0.5961538461538461453, 0.5974358974358974228, 0.5999999999999999778, 0.6025641025641025328, 0.6051282051282050878, 0.6076923076923076428, 0.6089743589743590313 ),
 .UNSPECIFIED. ) 
 CURVE ( )  GEOMETRIC_REPRESENTATION_ITEM ( )  RATIONAL_B_SPLINE_CURVE ( ( 0.9755282581475768211, 0.9755282581475768211, 1.000000000000000000, 0.9510565162951535312, 1.000000000000000000, 0.9510565162951535312, 1.000000000000000000, 0.9510565162951535312, 1.000000000000000000, 0.9510565162951535312, 1.000000000000000000, 0.9755282581475757109, 0.9755282581475768211 ) ) 
 REPRESENTATION_ITEM ( '' )  );
#27212 = DIRECTION ( 'NONE',  ( 0.000000000000000000, 0.000000000000000000, 1.000000000000000000 ) ) ;
#27213 = CARTESIAN_POINT ( 'NONE',  ( 7.468012846824281681, 42.07253499907601935, -28.02196122052058058 ) ) ;
#27214 = CARTESIAN_POINT ( 'NONE',  ( 4.635254915624209993, 77.39999999999999147, -14.26584774442730463 ) ) ;
#27215 = CARTESIAN_POINT ( 'NONE',  ( -26.00068869287368756, 49.66927083333332149, -15.01150461594595775 ) ) ;
#27216 = CARTESIAN_POINT ( 'NONE',  ( -24.50000000000000000, 16.74999999453763522, -3.000384657911015469E-15 ) ) ;
#27217 = CARTESIAN_POINT ( 'NONE',  ( 32.50000000000000711, 49.40000000546236691, 10.55989012756945122 ) ) ;
#27218 = CARTESIAN_POINT ( 'NONE',  ( 24.20753774853731244, 16.44010416666666430, -13.97622843553632599 ) ) ;
#27219 = CARTESIAN_POINT ( 'NONE',  ( -10.37757302488624411, 34.72500000273118559, -31.93888565452638417 ) ) ;
#27220 = CARTESIAN_POINT ( 'NONE',  ( -13.91746824999999532, 72.77500000273120406, -4.522059556121115875 ) ) ;
#27221 = CARTESIAN_POINT ( 'NONE',  ( 6.486482029760649416E-15, 51.87500000273119127, 35.31076352940723240 ) ) ;
#27222 = CARTESIAN_POINT ( 'NONE',  ( -33.58253175000000113, 27.47500000273118204, 10.91162601494193929 ) ) ;
#27223 = CARTESIAN_POINT ( 'NONE',  ( 19.09188309203694800, 34.34374999999999289, 19.09188309203660694 ) ) ;
#27224 = CARTESIAN_POINT ( 'NONE',  ( 0.000000000000000000, 102.0000000000000284, 0.000000000000000000 ) ) ;
#27225 = AXIS2_PLACEMENT_3D ( 'NONE', #15771, #28962, #2548 ) ;
#27226 = CARTESIAN_POINT ( 'NONE',  ( 10.04305231718578817, 31.39999999999998437, -30.90933677959249337 ) ) ;
#27227 = CARTESIAN_POINT ( 'NONE',  ( 20.08610463437158344, 64.70000000000001705, 27.64615127144129403 ) ) ;
#27228 = CARTESIAN_POINT ( 'NONE',  ( -10.37757302488624411, 6.725000002731185589, -31.93888565452638417 ) ) ;
#27229 = CARTESIAN_POINT ( 'NONE',  ( -18.94512977948575738, 7.424999997268811214, -13.76444248337723231 ) ) ;
#27230 = CARTESIAN_POINT ( 'NONE',  ( 25.98046417659831775, 25.31472249907601579, -15.04653450569338879 ) ) ;
#27231 = AXIS2_PLACEMENT_3D ( 'NONE', #30518, #27961, #33442 ) ;
#27232 = CARTESIAN_POINT ( 'NONE',  ( 0.000000000000000000, -20.99999999999998934, 0.000000000000000000 ) ) ;
#27233 = CARTESIAN_POINT ( 'NONE',  ( 19.11951029504797006, 29.46836833240935505, 19.06425588902558133 ) ) ;
#27234 = CARTESIAN_POINT ( 'NONE',  ( -8.891200544363830713E-16, 75.75000000546236834, -15.00000000000000000 ) ) ;
#27235 = CARTESIAN_POINT ( 'NONE',  ( -33.58253175000000113, 17.12500000273120548, 0.000000000000000000 ) ) ;
#27236 = CARTESIAN_POINT ( 'NONE',  ( -23.41746825000000598, 6.224999997268827023, 7.608796670333726198 ) ) ;
#27237 = CARTESIAN_POINT ( 'NONE',  ( -13.97622843553632421, 56.83072916666665009, -24.20753774853731599 ) ) ;
#27238 = ORIENTED_EDGE ( 'NONE', *, *, #15661, .F. ) ;
#27239 = CARTESIAN_POINT ( 'NONE',  ( -10.37757302488624411, 54.72500000273118559, -31.93888565452638417 ) ) ;
#27240 = CARTESIAN_POINT ( 'NONE',  ( -33.58253175000000113, 29.47500000273117848, 10.91162601494193929 ) ) ;
#27241 = EDGE_LOOP ( 'NONE', ( #27533, #14366, #8941, #27537, #10029, #28131, #15952, #14127, #17891, #11351, #3858, #30911, #4362, #2062, #25627, #12857, #12215, #16327, #18147 ) ) ;
#27242 = CARTESIAN_POINT ( 'NONE',  ( 30.02300923189239512, 27.03906250000000000, -2.619432448724977703E-13 ) ) ;
#27243 = CARTESIAN_POINT ( 'NONE',  ( -25.98046417659859486, 23.60715250092398421, -15.04653450569291628 ) ) ;
#27244 = DIRECTION ( 'NONE',  ( -0.000000000000000000, 1.000000000000000000, -0.000000000000000000 ) ) ;
#27245 = CARTESIAN_POINT ( 'NONE',  ( -19.82091636218621034, 18.54999999453762882, -14.40073868116559552 ) ) ;
#27246 = CARTESIAN_POINT ( 'NONE',  ( 18.94512977948576093, 8.824999997268822227, -13.76444248337722875 ) ) ;
#27247 = CARTESIAN_POINT ( 'NONE',  ( 20.75514604977249178, 20.07500000273118346, 28.56700777964553950 ) ) ;
#27248 = CARTESIAN_POINT ( 'NONE',  ( -26.29305231718578995, 30.70000000546238539, 19.10302069950538595 ) ) ;
#27249 = CARTESIAN_POINT ( 'NONE',  ( -26.29305231718578995, 74.19999999999998863, 19.10302069950538595 ) ) ;
#27250 = CARTESIAN_POINT ( 'NONE',  ( -5.147494310547423346, 6.948745723915522809, 32.50000000000000000 ) ) ;
#27251 = CARTESIAN_POINT ( 'NONE',  ( -8.891200544363830713E-16, 73.50000000000001421, -15.00000000000000000 ) ) ;
#27252 = CARTESIAN_POINT ( 'NONE',  ( 20.47846945139902530, 52.96913166759063785, 20.53372385742071771 ) ) ;
#27253 = CARTESIAN_POINT ( 'NONE',  ( 27.16883889988624290, 38.17500000273118843, 19.73931689729373673 ) ) ;
#27254 = CARTESIAN_POINT ( 'NONE',  ( 7.505752307973351023, 24.31770833333332504, 28.01184896238290278 ) ) ;
#27255 = AXIS2_PLACEMENT_3D ( 'NONE', #8752, #19736, #13915 ) ;
#27256 = CARTESIAN_POINT ( 'NONE',  ( 7.236395654485755280, 8.724999997268806595, 22.27133577429736988 ) ) ;
#27257 = CARTESIAN_POINT ( 'NONE',  ( 10.04305231718579705, 14.60000000000000142, 30.90933677959248982 ) ) ;
#27258 = CARTESIAN_POINT ( 'NONE',  ( -24.50000000000001066, 15.09999999999998899, 7.960532557706201828 ) ) ;
#27259 = CARTESIAN_POINT ( 'NONE',  ( 7.025853678916867295, 46.94232666574269075, 26.06988505166722803 ) ) ;
#27260 = CARTESIAN_POINT ( 'NONE',  ( -27.16883889988623935, 63.32500000273119412, 19.73931689729374739 ) ) ;
#27261 = CARTESIAN_POINT ( 'NONE',  ( -27.16883889988624290, 45.17500000273119554, -19.73931689729374028 ) ) ;
#27262 = CARTESIAN_POINT ( 'NONE',  ( 23.41746824999999887, 10.52499999726880731, 7.608796670333735079 ) ) ;
#27263 = CARTESIAN_POINT ( 'NONE',  ( -24.50000000000000711, 9.100000000000003197, 7.960532557706201828 ) ) ;
#27264 = CARTESIAN_POINT ( 'NONE',  ( 27.16883889988623935, 8.325000002731176352, -19.73931689729374384 ) ) ;
#27265 = CARTESIAN_POINT ( 'NONE',  ( 7.025853678916403666, 41.51079833425730214, -26.06988505166735237 ) ) ;
#27266 = DIRECTION ( 'NONE',  ( -0.5000000000000001110, 0.000000000000000000, -0.8660254037844387076 ) ) ;
#27267 = CARTESIAN_POINT ( 'NONE',  ( -32.24336671818454647, 52.00000000000002132, 4.711964452985278662 ) ) ;
#27268 = CARTESIAN_POINT ( 'NONE',  ( -33.58253175000000113, 31.22500000273118559, 10.91162601494193929 ) ) ;
#27269 = CARTESIAN_POINT ( 'NONE',  ( 3.673940397442059178E-15, -12.99999999999999822, -30.00000000000000000 ) ) ;
#27270 = FACE_OUTER_BOUND ( 'NONE', #7874, .T. ) ;
#27271 = CARTESIAN_POINT ( 'NONE',  ( 32.50000000000000000, 1.600000005462365760, -10.55989012756945833 ) ) ;
#27272 = CARTESIAN_POINT ( 'NONE',  ( 14.97647472619900455, 59.40326416574269075, -26.02091320914876960 ) ) ;
#27273 = CARTESIAN_POINT ( 'NONE',  ( 20.08610463437158344, 45.20000000546239249, 27.64615127144129403 ) ) ;
#27274 = EDGE_CURVE ( 'NONE', #16950, #2254, #7822, .T. ) ;
#27275 = CARTESIAN_POINT ( 'NONE',  ( -12.11000150615021553, -45.00000000000001421, 1.483047458217649221E-15 ) ) ;
#27276 = CARTESIAN_POINT ( 'NONE',  ( 2.584737979205441561E-13, 24.46093749999999645, 27.95245687107222921 ) ) ;
#27277 = EDGE_CURVE ( 'NONE', #17375, #4296, #9448, .T. ) ;
#27278 = CARTESIAN_POINT ( 'NONE',  ( 27.16883889988624290, 73.92500000273120975, 19.73931689729373673 ) ) ;
#27279 = CARTESIAN_POINT ( 'NONE',  ( -7.505752307973343918, 29.47395833333332860, -28.01184896238290989 ) ) ;
#27280 = CIRCLE ( 'NONE', #30575, 3.500000000000010214 ) ;
#27281 = DIRECTION ( 'NONE',  ( -1.000000000000000000, 0.000000000000000000, 0.000000000000000000 ) ) ;
#27282 = ORIENTED_EDGE ( 'NONE', *, *, #22716, .T. ) ;
#27283 = CARTESIAN_POINT ( 'NONE',  ( -20.47846945139902175, 51.25038166759065206, -20.53372385742072481 ) ) ;
#27284 = CARTESIAN_POINT ( 'NONE',  ( -10.04305231718578462, 12.90000000546236159, 30.90933677959249337 ) ) ;
#27285 = CARTESIAN_POINT ( 'NONE',  ( -28.01184896238290278, 59.55208333333332149, 7.505752307973363457 ) ) ;
#27286 = CARTESIAN_POINT ( 'NONE',  ( -5.147494310547430452, 64.05125428700922896, -32.49999999999999289 ) ) ;
#27287 = CARTESIAN_POINT ( 'NONE',  ( 27.16883889988624290, 50.17500000273117422, 19.73931689729373673 ) ) ;
#27288 = CARTESIAN_POINT ( 'NONE',  ( 32.50000000000000000, 49.60000000546239818, -10.55989012756945833 ) ) ;
#27289 = CARTESIAN_POINT ( 'NONE',  ( -15.00000000000000000, 82.00000000000001421, 0.000000000000000000 ) ) ;
#27290 = CARTESIAN_POINT ( 'NONE',  ( -33.58253175000000113, 31.02500000273118630, -10.91162601494193218 ) ) ;
#27291 = CARTESIAN_POINT ( 'NONE',  ( 5.779280353836490358E-15, 57.00000000546238965, 32.49999999999999289 ) ) ;
#27292 = CARTESIAN_POINT ( 'NONE',  ( -33.58253175000000113, 65.27500000273117564, -10.91162601494193218 ) ) ;
#27293 = FILL_AREA_STYLE ('',( #29518 ) ) ;
#27294 = CARTESIAN_POINT ( 'NONE',  ( 26.29305231718579350, 38.79999999999999005, 19.10302069950537529 ) ) ;
#27295 = CARTESIAN_POINT ( 'NONE',  ( -32.50000000000000000, 34.00000000000000000, 0.000000000000000000 ) ) ;
#27296 = CARTESIAN_POINT ( 'NONE',  ( 7.236395654485755280, 10.22499999726880837, 22.27133577429736988 ) ) ;
#27297 = CARTESIAN_POINT ( 'NONE',  ( 27.16883889988624290, 4.175000002731188431, 19.73931689729373673 ) ) ;
#27298 = DIRECTION ( 'NONE',  ( -0.000000000000000000, -1.000000000000000000, -0.000000000000000000 ) ) ;
#27299 = CARTESIAN_POINT ( 'NONE',  ( -11.25946833292375793, 79.17500000273119554, -8.180482586598733619 ) ) ;
#27300 = CARTESIAN_POINT ( 'NONE',  ( 10.37757302488624767, 67.97500000273117848, 31.93888565452638417 ) ) ;
#27301 = CARTESIAN_POINT ( 'NONE',  ( 15.14183272437242422, 4.049999994537630599, -20.84094480462497856 ) ) ;
#27302 = CARTESIAN_POINT ( 'NONE',  ( -33.58253175000000113, 61.47500000273117848, 10.91162601494193929 ) ) ;
#27303 = EDGE_LOOP ( 'NONE', ( #21277, #22895, #20596, #2606 ) ) ;
#27304 = CARTESIAN_POINT ( 'NONE',  ( 15.14183272437241889, 5.449999994537614079, 20.84094480462498211 ) ) ;
#27305 = CIRCLE ( 'NONE', #22927, 24.50000000000000000 ) ;
#27306 = CARTESIAN_POINT ( 'NONE',  ( -26.07999730980477437, 66.42708333333332860, 6.988114217768305103 ) ) ;
#27307 = CARTESIAN_POINT ( 'NONE',  ( 2.375766604868043252, 75.44874571845315359, -14.99999999999999822 ) ) ;
#27308 = CARTESIAN_POINT ( 'NONE',  ( 10.37757302488624056, 50.52500000273117564, -31.93888565452638417 ) ) ;
#27309 = CARTESIAN_POINT ( 'NONE',  ( -10.37757302488624411, 8.975000002731201576, -31.93888565452638417 ) ) ;
#27310 = CARTESIAN_POINT ( 'NONE',  ( -33.58253175000000113, 61.27500000273118985, -10.91162601494193041 ) ) ;
#27311 = CARTESIAN_POINT ( 'NONE',  ( -6.988114217768288228, 50.09895833333332860, -26.07999730980477437 ) ) ;
#27312 =( BOUNDED_CURVE ( )  B_SPLINE_CURVE ( 2, ( #24133, #935, #21561, #21393, #11414, #1095, #21890, #13502, #11091, #32340, #18821, #19317, #6265 ),
 .UNSPECIFIED., .F., .F. ) 
 B_SPLINE_CURVE_WITH_KNOTS ( ( 3, 2, 2, 2, 2, 2, 3 ),
 ( 0.02777777777777777971, 0.03333333333333333287, 0.04444444444444444614, 0.05555555555555555247, 0.06666666666666667962, 0.07777777777777777901, 0.08333333333333334259 ),
 .UNSPECIFIED. ) 
 CURVE ( )  GEOMETRIC_REPRESENTATION_ITEM ( )  RATIONAL_B_SPLINE_CURVE ( ( 0.9755282581475768211, 0.9755282581475768211, 1.000000000000000000, 0.9510565162951535312, 1.000000000000000000, 0.9510565162951535312, 1.000000000000000000, 0.9510565162951535312, 1.000000000000000000, 0.9510565162951535312, 1.000000000000000000, 0.9755282581475767101, 0.9755282581475768211 ) ) 
 REPRESENTATION_ITEM ( '' )  );
#27313 = CARTESIAN_POINT ( 'NONE',  ( 28.00173670424549499, 35.49517333425730214, 7.543491769121417612 ) ) ;
#27314 = CARTESIAN_POINT ( 'NONE',  ( -0.04044903255044120238, 28.17930583240935860, -30.02300923189239867 ) ) ;
#27315 = CARTESIAN_POINT ( 'NONE',  ( 10.04305231718578817, 69.90000000546238823, -30.90933677959249337 ) ) ;
#27316 = CARTESIAN_POINT ( 'NONE',  ( 2.688165632520823219E-15, 77.37500000273118417, 14.63369212191046387 ) ) ;
#27317 =( BOUNDED_CURVE ( )  B_SPLINE_CURVE ( 2, ( #28192, #9658, #33506, #17221, #20138, #25624, #30933, #28365, #12405, #22526, #22875, #20482, #33333 ),
 .UNSPECIFIED., .F., .T. ) 
 B_SPLINE_CURVE_WITH_KNOTS ( ( 3, 2, 2, 2, 2, 2, 3 ),
 ( 0.3141025641025640969, 0.3153846153846153744, 0.3179487179487179294, 0.3205128205128205399, 0.3230769230769230949, 0.3256410256410256499, 0.3269230769230769273 ),
 .UNSPECIFIED. ) 
 CURVE ( )  GEOMETRIC_REPRESENTATION_ITEM ( )  RATIONAL_B_SPLINE_CURVE ( ( 0.9755282581475768211, 0.9755282581475768211, 1.000000000000000000, 0.9510565162951535312, 1.000000000000000000, 0.9510565162951535312, 1.000000000000000000, 0.9510565162951535312, 1.000000000000000000, 0.9510565162951535312, 1.000000000000000000, 0.9755282581475768211, 0.9755282581475768211 ) ) 
 REPRESENTATION_ITEM ( '' )  );
#27318 = CARTESIAN_POINT ( 'NONE',  ( 19.06425588902558133, 52.67149333240935505, -19.11951029504797006 ) ) ;
#27319 = CARTESIAN_POINT ( 'NONE',  ( 0.000000000000000000, 80.00000000000001421, 0.000000000000000000 ) ) ;
#27320 = EDGE_CURVE ( 'NONE', #11374, #19067, #4881, .T. ) ;
#27321 = DIRECTION ( 'NONE',  ( -1.224646799147353454E-16, 1.000000000000000000, -0.000000000000000000 ) ) ;
#27322 = EDGE_CURVE ( 'NONE', #7039, #9545, #56, .T. ) ;
#27323 = VERTEX_POINT ( 'NONE', #28555 ) ;
#27324 = CARTESIAN_POINT ( 'NONE',  ( -10.37757302488623701, 39.77500000273119696, 31.93888565452638417 ) ) ;
#27325 = CARTESIAN_POINT ( 'NONE',  ( -7.236395654485763274, 4.524999997268825069, 22.27133577429736633 ) ) ;
#27326 = CARTESIAN_POINT ( 'NONE',  ( -32.50000000000000000, 30.40000000546238823, -10.55989012756945478 ) ) ;
#27327 = EDGE_LOOP ( 'NONE', ( #14282, #30093, #21704, #29926 ) ) ;
#27328 = CARTESIAN_POINT ( 'NONE',  ( 2.740863092043355209E-13, 38.21093750000000000, 30.02300923189239512 ) ) ;
#27329 = ORIENTED_EDGE ( 'NONE', *, *, #32821, .T. ) ;
#27330 = EDGE_LOOP ( 'NONE', ( #8107, #20684, #15353, #910 ) ) ;
#27331 = CARTESIAN_POINT ( 'NONE',  ( 5.779280353836490358E-15, 75.00000000546236834, 32.49999999999999289 ) ) ;
#27332 = CARTESIAN_POINT ( 'NONE',  ( -27.16883889988624290, 56.92500000273120975, -19.73931689729374028 ) ) ;
#27333 = CARTESIAN_POINT ( 'NONE',  ( -7.505752307972844761, 58.97916666666666430, 28.01184896238304134 ) ) ;
#27334 = EDGE_CURVE ( 'NONE', #3193, #3734, #9774, .T. ) ;
#27335 = CARTESIAN_POINT ( 'NONE',  ( 32.50000000000000000, 9.500000005462361230, -3.980102097228898626E-15 ) ) ;
#27336 = CARTESIAN_POINT ( 'NONE',  ( -15.31642273298460744, -59.03347138510255832, 0.000000000000000000 ) ) ;
#27337 = CARTESIAN_POINT ( 'NONE',  ( 14.47279130897151767, 14.82499999726881690, 19.92008829642072953 ) ) ;
#27338 = CARTESIAN_POINT ( 'NONE',  ( 26.29305231718579350, 56.80000000000001847, 19.10302069950537529 ) ) ;
#27339 = CARTESIAN_POINT ( 'NONE',  ( -20.75514604977248112, 25.67500000273118488, 28.56700777964554661 ) ) ;
#27340 = CARTESIAN_POINT ( 'NONE',  ( 11.54700538379251107, 96.00000000000002842, -19.99999999999999645 ) ) ;
#27341 = CARTESIAN_POINT ( 'NONE',  ( 7.543491769121922985, 67.56732666574268364, 28.00173670424535644 ) ) ;
#27342 = CARTESIAN_POINT ( 'NONE',  ( -13.91746824999999887, 76.87500000273116996, 0.000000000000000000 ) ) ;
#27343 = CARTESIAN_POINT ( 'NONE',  ( -24.50000000000000000, 0.9000000000000005773, -7.960532557706207157 ) ) ;
#27344 = CARTESIAN_POINT ( 'NONE',  ( -20.08610463437156923, 28.80000000546237970, 27.64615127144130113 ) ) ;
#27345 = CARTESIAN_POINT ( 'NONE',  ( -10.04305231718578462, 8.400000000000003908, 30.90933677959249337 ) ) ;
#27346 = ORIENTED_EDGE ( 'NONE', *, *, #9844, .F. ) ;
#27347 = CARTESIAN_POINT ( 'NONE',  ( 14.47279130897151589, 6.824999997268808904, 19.92008829642072953 ) ) ;
#27348 = PLANE ( 'NONE',  #13242 ) ;
#27349 = CARTESIAN_POINT ( 'NONE',  ( -13.97622843553632421, 39.64322916666667140, -24.20753774853731599 ) ) ;
#27350 = CARTESIAN_POINT ( 'NONE',  ( 10.37757302488624767, 15.72500000273119269, 31.93888565452638417 ) ) ;
#27351 = CARTESIAN_POINT ( 'NONE',  ( 33.58253175000000823, 68.02500000273117564, 10.91162601494192863 ) ) ;
#27352 = CARTESIAN_POINT ( 'NONE',  ( 27.16883889988623935, 28.57500000273117990, -19.73931689729374384 ) ) ;
#27353 = CARTESIAN_POINT ( 'NONE',  ( -33.58253175000000113, 17.37500000273119127, 0.000000000000000000 ) ) ;
#27354 = CARTESIAN_POINT ( 'NONE',  ( -33.58253175000000113, 11.37500000273117351, 0.000000000000000000 ) ) ;
#27355 = CARTESIAN_POINT ( 'NONE',  ( 27.95245687107223986, 62.85194416759064495, 0.04044903254993640479 ) ) ;
#27356 = CARTESIAN_POINT ( 'NONE',  ( 20.50609665440969565, 50.67187500000000000, -20.50609665441004736 ) ) ;
#27357 = CARTESIAN_POINT ( 'NONE',  ( 8.891200544363830713E-16, 81.50000000000001421, -15.00000000000000000 ) ) ;
#27358 = CARTESIAN_POINT ( 'NONE',  ( 13.91746824999999887, 74.37500000273116996, -1.704398294459741270E-15 ) ) ;
#27359 = CARTESIAN_POINT ( 'NONE',  ( 10.04305231718579705, 48.59999999999998721, 30.90933677959248982 ) ) ;
#27360 = FILL_AREA_STYLE_COLOUR ( '', #818 ) ;
#27361 = CARTESIAN_POINT ( 'NONE',  ( -20.75514604977248823, 48.82500000273117990, -28.56700777964554305 ) ) ;
#27362 = CARTESIAN_POINT ( 'NONE',  ( 1.507698388325705758E-15, 5.124999997268805174, -24.62258325217400312 ) ) ;
#27363 = VERTEX_POINT ( 'NONE', #17942 ) ;
#27364 = CARTESIAN_POINT ( 'NONE',  ( 27.16883889988623935, 62.57500000273117990, -19.73931689729374384 ) ) ;
#27365 = CARTESIAN_POINT ( 'NONE',  ( -1.778240108872766143E-15, 17.50000000000000000, -32.49999999999999289 ) ) ;
#27366 = CARTESIAN_POINT ( 'NONE',  ( 7.236395654485755280, 8.224999997268806595, 22.27133577429736988 ) ) ;
#27367 = CARTESIAN_POINT ( 'NONE',  ( 24.22776226481241224, 35.06548583425731636, -13.94119854578936923 ) ) ;
#27368 = VERTEX_POINT ( 'NONE', #29058 ) ;
#27369 = CARTESIAN_POINT ( 'NONE',  ( -27.16883889988624290, 34.92500000273117422, -19.73931689729374028 ) ) ;
#27370 = DIRECTION ( 'NONE',  ( 0.5000000000000000000, 0.000000000000000000, 0.8660254037844385966 ) ) ;
#27371 = EDGE_LOOP ( 'NONE', ( #8478, #27835, #17624, #22183 ) ) ;
#27372 = CARTESIAN_POINT ( 'NONE',  ( -26.00068869287340334, 52.53385416666666430, 15.01150461594643382 ) ) ;
#27373 = CARTESIAN_POINT ( 'NONE',  ( -10.37757302488624411, 60.97500000273120691, -31.93888565452638417 ) ) ;
#27374 = CARTESIAN_POINT ( 'NONE',  ( 6.486482029760649416E-15, 75.62500000273121259, 35.31076352940723240 ) ) ;
#27375 = CARTESIAN_POINT ( 'NONE',  ( 15.01150461594596308, 26.46614583333332149, -26.00068869287367335 ) ) ;
#27376 = CARTESIAN_POINT ( 'NONE',  ( -4.732186688966233175E-15, 7.499999999999995559, 25.76082449383753925 ) ) ;
#27377 = CARTESIAN_POINT ( 'NONE',  ( -33.58253175000000113, 1.475000002731190474, 10.91162601494193929 ) ) ;
#27378 = CARTESIAN_POINT ( 'NONE',  ( -33.58253175000000113, 17.22500000273118559, 10.91162601494193929 ) ) ;
#27379 = CARTESIAN_POINT ( 'NONE',  ( 8.601468415847516980, 72.17500000273119554, -11.83890561707634603 ) ) ;
#27380 = CARTESIAN_POINT ( 'NONE',  ( 26.02091320914876960, 43.07513916574269786, 14.97647472619900455 ) ) ;
#27381 = CARTESIAN_POINT ( 'NONE',  ( 4.635254915624209993, 81.40000000000000568, -14.26584774442730463 ) ) ;
#27382 = CARTESIAN_POINT ( 'NONE',  ( 15.01150461594643382, 55.11197916666665719, 26.00068869287340334 ) ) ;
#27383 = CARTESIAN_POINT ( 'NONE',  ( -19.82091636218621389, 8.949999994537632730, 14.40073868116558842 ) ) ;
#27384 = CARTESIAN_POINT ( 'NONE',  ( 24.50000000000000355, 7.649999994537632908, 7.960532557706212486 ) ) ;
#27385 = CYLINDRICAL_SURFACE ( 'NONE', #32406, 24.50000000000000000 ) ;
#27386 = CARTESIAN_POINT ( 'NONE',  ( -13.94119854578892514, 67.99701416574269786, 24.22776226481266448 ) ) ;
#27387 = CARTESIAN_POINT ( 'NONE',  ( 27.16883889988624290, 37.92500000273118843, 19.73931689729373673 ) ) ;
#27388 = CARTESIAN_POINT ( 'NONE',  ( 13.91746824999999887, 73.87500000273116996, -1.704398294459741270E-15 ) ) ;
#27389 = CARTESIAN_POINT ( 'NONE',  ( 20.75514604977249178, 50.07500000273120122, 28.56700777964553950 ) ) ;
#27390 = CARTESIAN_POINT ( 'NONE',  ( -20.75514604977248112, 29.67500000273119909, 28.56700777964554661 ) ) ;
#27391 = CARTESIAN_POINT ( 'NONE',  ( -2.361898896031838557, 16.99999999999998579, 24.02576800177196503 ) ) ;
#27392 = CARTESIAN_POINT ( 'NONE',  ( 26.07999730980477437, 33.77083333333333570, -6.988114217768290004 ) ) ;
#27393 = CARTESIAN_POINT ( 'NONE',  ( 3.880418787951132042, 2.448745718453165576, -24.50000000000000355 ) ) ;
#27394 = CARTESIAN_POINT ( 'NONE',  ( 32.50000000000000000, 79.10000000000000853, -10.55989012756945833 ) ) ;
#27395 = CARTESIAN_POINT ( 'NONE',  ( 32.50000000000000711, 66.90000000000001990, 10.55989012756945122 ) ) ;
#27396 = CARTESIAN_POINT ( 'NONE',  ( 23.41746824999999887, 8.624999997268817609, 0.000000000000000000 ) ) ;
#27397 = CARTESIAN_POINT ( 'NONE',  ( -15.04653450569338524, 27.89284749907601935, -25.98046417659831775 ) ) ;
#27398 = DIRECTION ( 'NONE',  ( 0.8660254037844365982, -0.5000000000000036637, 0.000000000000000000 ) ) ;
#27399 = CARTESIAN_POINT ( 'NONE',  ( -26.06988505166722803, 40.92670166574268364, 7.025853678916877953 ) ) ;
#27400 = EDGE_CURVE ( 'NONE', #1133, #771, #1775, .T. ) ;
#27401 = CARTESIAN_POINT ( 'NONE',  ( -20.75514604977248823, 77.07500000273117280, -28.56700777964554305 ) ) ;
#27402 = CARTESIAN_POINT ( 'NONE',  ( -10.37757302488624411, 10.72500000273118914, -31.93888565452638417 ) ) ;
#27403 = CARTESIAN_POINT ( 'NONE',  ( 7.236395654485755280, 6.724999997268804819, 22.27133577429736988 ) ) ;
#27404 = CARTESIAN_POINT ( 'NONE',  ( 13.97622843553589966, 57.40364583333333570, -24.20753774853756113 ) ) ;
#27405 = ORIENTED_EDGE ( 'NONE', *, *, #7993, .T. ) ;
#27406 = CARTESIAN_POINT ( 'NONE',  ( -33.58253175000000113, 53.12500000273119838, 0.000000000000000000 ) ) ;
#27407 = CARTESIAN_POINT ( 'NONE',  ( -2.162160676586881955E-15, 30.87500000273119483, -35.31076352940723240 ) ) ;
#27408 =( BOUNDED_CURVE ( )  B_SPLINE_CURVE ( 2, ( #29617, #18686, #6120, #10948, #29295, #16603, #27057, #24486, #959, #6291, #16767, #16112, #29958 ),
 .UNSPECIFIED., .F., .T. ) 
 B_SPLINE_CURVE_WITH_KNOTS ( ( 3, 2, 2, 2, 2, 2, 3 ),
 ( 0.5500000000000000444, 0.5600000000000000533, 0.5799999999999999600, 0.5999999999999999778, 0.6199999999999999956, 0.6400000000000000133, 0.6500000000000000222 ),
 .UNSPECIFIED. ) 
 CURVE ( )  GEOMETRIC_REPRESENTATION_ITEM ( )  RATIONAL_B_SPLINE_CURVE ( ( 0.9755282581475768211, 0.9755282581475768211, 1.000000000000000000, 0.9510565162951535312, 1.000000000000000000, 0.9510565162951535312, 1.000000000000000000, 0.9510565162951535312, 1.000000000000000000, 0.9510565162951535312, 1.000000000000000000, 0.9755282581475768211, 0.9755282581475768211 ) ) 
 REPRESENTATION_ITEM ( '' )  );
#27409 = ORIENTED_EDGE ( 'NONE', *, *, #33358, .F. ) ;
#27410 = CARTESIAN_POINT ( 'NONE',  ( -26.00068869287340334, 28.47135416666666075, 15.01150461594643382 ) ) ;
#27411 = CARTESIAN_POINT ( 'NONE',  ( 0.04044903254992426173, 20.74256916759064495, -30.02300923189239867 ) ) ;
#27412 = CARTESIAN_POINT ( 'NONE',  ( 3.880418787951140036, 16.19874571299077459, -24.49999999999999645 ) ) ;
#27413 = CARTESIAN_POINT ( 'NONE',  ( -19.82091636218621034, 14.54999999453762705, -14.40073868116559552 ) ) ;
#27414 = CARTESIAN_POINT ( 'NONE',  ( -14.47279130897152122, 5.924999997268808549, 19.92008829642072243 ) ) ;
#27415 = CARTESIAN_POINT ( 'NONE',  ( -33.58253175000000113, 19.27500000273117919, -10.91162601494193218 ) ) ;
#27416 = CARTESIAN_POINT ( 'NONE',  ( 10.04305231718578817, 29.90000000546239178, -30.90933677959249337 ) ) ;
#27417 = CARTESIAN_POINT ( 'NONE',  ( 32.50000000000000000, 73.09999999999996589, -10.55989012756945833 ) ) ;
#27418 = CYLINDRICAL_SURFACE ( 'NONE', #11591, 26.50000000000000000 ) ;
#27419 = CARTESIAN_POINT ( 'NONE',  ( 0.04044903254992426173, 58.55506916759063785, -30.02300923189239867 ) ) ;
#27420 = CARTESIAN_POINT ( 'NONE',  ( -20.75514604977248112, 33.67500000273119554, 28.56700777964554661 ) ) ;
#27421 = CARTESIAN_POINT ( 'NONE',  ( 10.37757302488624056, 54.52500000273118275, -31.93888565452638417 ) ) ;
#27422 = CARTESIAN_POINT ( 'NONE',  ( 28.01184896238304134, 34.05729166666666430, 7.505752307972846538 ) ) ;
#27423 = CARTESIAN_POINT ( 'NONE',  ( 14.47279130897151589, 10.82499999726880091, 19.92008829642072953 ) ) ;
#27424 = CARTESIAN_POINT ( 'NONE',  ( 32.50000000000000000, 13.09999999999999432, -10.55989012756945833 ) ) ;
#27425 = CARTESIAN_POINT ( 'NONE',  ( 24.50000000000000000, 10.00000000000000888, 0.000000000000000000 ) ) ;
#27426 = CARTESIAN_POINT ( 'NONE',  ( -27.95245687107223986, 47.94493083240935505, 0.04044903255043252877 ) ) ;
#27427 = CARTESIAN_POINT ( 'NONE',  ( -2.162160676586881955E-15, 56.62500000273116996, -35.31076352940723240 ) ) ;
#27428 = CARTESIAN_POINT ( 'NONE',  ( 27.16883889988623935, 44.57500000273117990, -19.73931689729374384 ) ) ;
#27429 = CARTESIAN_POINT ( 'NONE',  ( 14.47279130897151944, 12.92499999726881832, -19.92008829642072598 ) ) ;
#27430 = CARTESIAN_POINT ( 'NONE',  ( 7.890940483122900408E-14, 10.49999999999999112, -24.50000000000000000 ) ) ;
#27431 = DIRECTION ( 'NONE',  ( -1.000000000000000000, 0.000000000000000000, 0.000000000000000000 ) ) ;
#27432 = CARTESIAN_POINT ( 'NONE',  ( -24.18731323226248264, 40.79465250092398065, -14.01125832528284931 ) ) ;
#27433 = DIRECTION ( 'NONE',  ( 0.000000000000000000, 0.000000000000000000, -1.000000000000000000 ) ) ;
#27434 = CARTESIAN_POINT ( 'NONE',  ( 5.779280353836490358E-15, 42.49999999999999289, 32.49999999999999289 ) ) ;
#27435 = CARTESIAN_POINT ( 'NONE',  ( -2.162160676586881955E-15, 30.62500000273119838, -35.31076352940723240 ) ) ;
#27436 = CARTESIAN_POINT ( 'NONE',  ( 5.147494310547434893, 66.55125428154683220, 32.49999999999999289 ) ) ;
#27437 = DIRECTION ( 'NONE',  ( 0.000000000000000000, -1.000000000000000000, 0.000000000000000000 ) ) ;
#27438 = CARTESIAN_POINT ( 'NONE',  ( 10.04305231718579705, 1.100000005462370423, 30.90933677959248982 ) ) ;
#27439 = CARTESIAN_POINT ( 'NONE',  ( -20.47846945139866648, 54.39024333240934794, 20.53372385742108008 ) ) ;
#27440 = CARTESIAN_POINT ( 'NONE',  ( -2.092463501923844636E-15, 50.00000000546237544, -34.17252228774368916 ) ) ;
#27441 =( LENGTH_UNIT ( ) NAMED_UNIT ( * ) SI_UNIT ( .MILLI., .METRE. ) );
#27442 = CARTESIAN_POINT ( 'NONE',  ( -2.162160676586882350E-15, 34.62500000273119127, -35.31076352940722529 ) ) ;
#27443 = CARTESIAN_POINT ( 'NONE',  ( 19.09188309203661049, 30.04687500000000000, -19.09188309203694445 ) ) ;
#27444 = ORIENTED_EDGE ( 'NONE', *, *, #18568, .F. ) ;
#27445 = CARTESIAN_POINT ( 'NONE',  ( -10.37757302488624411, 76.72500000273117848, -31.93888565452638417 ) ) ;
#27446 = CARTESIAN_POINT ( 'NONE',  ( -26.00068869287368756, 29.04427083333332504, -15.01150461594595775 ) ) ;
#27447 =( BOUNDED_CURVE ( )  B_SPLINE_CURVE ( 2, ( #11476, #24521, #21789, #16145, #19049, #21622, #29488, #3419, #26923, #8730, #29650, #5662, #991 ),
 .UNSPECIFIED., .F., .F. ) 
 B_SPLINE_CURVE_WITH_KNOTS ( ( 3, 2, 2, 2, 2, 2, 3 ),
 ( 0.1944444444444444475, 0.2000000000000000111, 0.2111111111111111105, 0.2222222222222222099, 0.2333333333333333370, 0.2444444444444444364, 0.2500000000000000000 ),
 .UNSPECIFIED. ) 
 CURVE ( )  GEOMETRIC_REPRESENTATION_ITEM ( )  RATIONAL_B_SPLINE_CURVE ( ( 0.9755282581475768211, 0.9755282581475768211, 1.000000000000000000, 0.9510565162951535312, 1.000000000000000000, 0.9510565162951535312, 1.000000000000000000, 0.9510565162951535312, 1.000000000000000000, 0.9510565162951535312, 1.000000000000000000, 0.9755282581475767101, 0.9755282581475768211 ) ) 
 REPRESENTATION_ITEM ( '' )  );
#27448 = FACE_OUTER_BOUND ( 'NONE', #14158, .T. ) ;
#27449 = ORIENTED_EDGE ( 'NONE', *, *, #19642, .F. ) ;
#27450 = CARTESIAN_POINT ( 'NONE',  ( -30.02300923189239867, 54.25819416759065206, -0.04044903254991731589 ) ) ;
#27451 = CARTESIAN_POINT ( 'NONE',  ( -20.08610463437157989, 12.20000000546237828, -27.64615127144129758 ) ) ;
#27452 = CARTESIAN_POINT ( 'NONE',  ( -26.00068869287368756, 63.41927083333333570, -15.01150461594595775 ) ) ;
#27453 = DIRECTION ( 'NONE',  ( -1.224646799147353454E-16, 1.000000000000000000, -0.000000000000000000 ) ) ;
#27454 = CARTESIAN_POINT ( 'NONE',  ( -27.16883889988624290, 43.17500000273119554, -19.73931689729374028 ) ) ;
#27455 = CARTESIAN_POINT ( 'NONE',  ( -20.08610463437156923, 50.80000000546237970, 27.64615127144130113 ) ) ;
#27456 = CARTESIAN_POINT ( 'NONE',  ( -4.300734207923755825, 73.77500000273118985, 13.23629886949340673 ) ) ;
#27457 = CARTESIAN_POINT ( 'NONE',  ( -33.58253175000000113, 29.12500000273118772, 0.000000000000000000 ) ) ;
#27458 = CARTESIAN_POINT ( 'NONE',  ( 2.667360163309149608E-15, 78.00000000546238255, -32.50000000000000000 ) ) ;
#27459 = CARTESIAN_POINT ( 'NONE',  ( -20.75514604977248112, 53.67500000273119554, 28.56700777964554661 ) ) ;
#27460 = DIRECTION ( 'NONE',  ( 0.000000000000000000, 0.000000000000000000, 1.000000000000000000 ) ) ;
#27461 = CARTESIAN_POINT ( 'NONE',  ( -20.08610463437157989, 35.70000000000000995, -27.64615127144129758 ) ) ;
#27462 = CARTESIAN_POINT ( 'NONE',  ( -32.50000000000000000, 34.10000000000000142, 10.55989012756946366 ) ) ;
#27463 = CARTESIAN_POINT ( 'NONE',  ( 18.94512977948575738, 10.42499999726881299, 13.76444248337723408 ) ) ;
#27464 = EDGE_CURVE ( 'NONE', #28463, #30412, #29174, .T. ) ;
#27465 = CARTESIAN_POINT ( 'NONE',  ( -2.162160676586881955E-15, 78.62500000273115575, -35.31076352940723240 ) ) ;
#27466 = CYLINDRICAL_SURFACE ( 'NONE', #9628, 32.50000000000000000 ) ;
#27467 = AXIS2_PLACEMENT_3D ( 'NONE', #29933, #14839, #6437 ) ;
#27468 = CARTESIAN_POINT ( 'NONE',  ( 13.91746825000000065, 76.27500000273116143, 4.522059556121115875 ) ) ;
#27469 = CARTESIAN_POINT ( 'NONE',  ( -27.16883889988623935, 65.57500000273120122, 19.73931689729374739 ) ) ;
#27470 = LINE ( 'NONE', #536, #18254 ) ;
#27471 = EDGE_CURVE ( 'NONE', #27323, #12256, #8672, .T. ) ;
#27472 = CARTESIAN_POINT ( 'NONE',  ( 3.980102097228898626E-15, 80.00000000000001421, 32.50000000000000000 ) ) ;
#27473 = CARTESIAN_POINT ( 'NONE',  ( -24.50000000000000000, 2.749999994537621895, -3.000384657911015469E-15 ) ) ;
#27474 = CARTESIAN_POINT ( 'NONE',  ( 27.95245687107223986, 14.72694416759064318, 0.04044903254993640479 ) ) ;
#27475 = DIRECTION ( 'NONE',  ( -0.000000000000000000, 1.000000000000000000, -0.000000000000000000 ) ) ;
#27476 = CARTESIAN_POINT ( 'NONE',  ( -27.16883889988624290, 48.92500000273118843, -19.73931689729374028 ) ) ;
#27477 = CARTESIAN_POINT ( 'NONE',  ( 10.37757302488624767, 5.975000002731184701, 31.93888565452638417 ) ) ;
#27478 = CARTESIAN_POINT ( 'NONE',  ( -33.58253175000000113, 59.37500000273119838, 0.000000000000000000 ) ) ;
#27479 = CARTESIAN_POINT ( 'NONE',  ( 26.07999730980490227, 51.24479166666666430, 6.988114217767821046 ) ) ;
#27480 = CARTESIAN_POINT ( 'NONE',  ( 25.98046417659858420, 35.63840250092398065, 15.04653450569292872 ) ) ;
#27481 = CARTESIAN_POINT ( 'NONE',  ( -7.468012846824272799, 26.60378499907601579, 28.02196122052058413 ) ) ;
#27482 = CARTESIAN_POINT ( 'NONE',  ( -20.08610463437157989, 68.20000000546239960, -27.64615127144129758 ) ) ;
#27483 = CARTESIAN_POINT ( 'NONE',  ( -8.960552108402742093E-16, 80.37500000273118417, -14.63369212191046387 ) ) ;
#27484 = CARTESIAN_POINT ( 'NONE',  ( -27.95245687107223986, 58.25743083240935505, 0.04044903255043252877 ) ) ;
#27485 = CARTESIAN_POINT ( 'NONE',  ( -20.08610463437156923, 54.30000000000000426, 27.64615127144130113 ) ) ;
#27486 = CARTESIAN_POINT ( 'NONE',  ( 32.50000000000000000, 59.09999999999999432, -10.55989012756945833 ) ) ;
#27487 = ORIENTED_EDGE ( 'NONE', *, *, #5855, .T. ) ;
#27488 = CARTESIAN_POINT ( 'NONE',  ( 33.58253175000000113, 42.37500000273118417, -4.112674001490185761E-15 ) ) ;
#27489 = CARTESIAN_POINT ( 'NONE',  ( 14.47279130897151767, 2.824999997268819119, 19.92008829642072953 ) ) ;
#27490 = AXIS2_PLACEMENT_3D ( 'NONE', #31180, #2701, #2352 ) ;
#27491 = CARTESIAN_POINT ( 'NONE',  ( -20.08610463437156923, 26.80000000546238681, 27.64615127144130113 ) ) ;
#27492 = ORIENTED_EDGE ( 'NONE', *, *, #16924, .T. ) ;
#27493 = CARTESIAN_POINT ( 'NONE',  ( -20.50609665441004736, 36.06250000000000000, -20.50609665440969565 ) ) ;
#27494 = EDGE_LOOP ( 'NONE', ( #25937, #4877, #10794, #2477 ) ) ;
#27495 = VERTEX_POINT ( 'NONE', #24263 ) ;
#27496 = CARTESIAN_POINT ( 'NONE',  ( 7.890940483122900408E-14, 12.24999999453763166, -24.50000000000000000 ) ) ;
#27497 = CARTESIAN_POINT ( 'NONE',  ( 33.58253175000000113, 48.22500000273119269, -10.91162601494193751 ) ) ;
#27498 = CARTESIAN_POINT ( 'NONE',  ( 26.00068869287340334, 54.25260416666666430, -15.01150461594642316 ) ) ;
#27499 = CARTESIAN_POINT ( 'NONE',  ( 26.29305231718579350, 11.30000000546238503, 19.10302069950537529 ) ) ;
#27500 = CARTESIAN_POINT ( 'NONE',  ( 0.000000000000000000, 11.99999999999999645, 0.000000000000000000 ) ) ;
#27501 = CARTESIAN_POINT ( 'NONE',  ( -18.94512977948576093, 14.32499999726882756, 13.76444248337722698 ) ) ;
#27502 = CARTESIAN_POINT ( 'NONE',  ( -26.29305231718579350, 51.80000000000001137, -19.10302069950537884 ) ) ;
#27503 = EDGE_CURVE ( 'NONE', #3774, #15262, #731, .T. ) ;
#27504 = CARTESIAN_POINT ( 'NONE',  ( 27.16883889988624290, 24.17500000273117777, 19.73931689729373673 ) ) ;
#27505 = CARTESIAN_POINT ( 'NONE',  ( 3.000384657911015469E-15, 16.99999999999998579, 24.50000000000000000 ) ) ;
#27506 = CARTESIAN_POINT ( 'NONE',  ( 24.18731323226221974, 15.00222249907602112, -14.01125832528328985 ) ) ;
#27507 = CARTESIAN_POINT ( 'NONE',  ( 2.688165632520823219E-15, 77.37500000273118417, 14.63369212191046387 ) ) ;
#27508 = CARTESIAN_POINT ( 'NONE',  ( 0.000000000000000000, -22.99999999999999289, -15.00000000000000000 ) ) ;
#27509 = DIRECTION ( 'NONE',  ( 0.000000000000000000, 0.000000000000000000, 1.000000000000000000 ) ) ;
#27510 =( BOUNDED_CURVE ( )  B_SPLINE_CURVE ( 2, ( #14498, #25480, #12255, #33181, #14667, #1265, #19813, #30436, #24786, #9684, #19989, #22224, #28049 ),
 .UNSPECIFIED., .F., .T. ) 
 B_SPLINE_CURVE_WITH_KNOTS ( ( 3, 2, 2, 2, 2, 2, 3 ),
 ( 0.5576923076923077094, 0.5589743589743589869, 0.5615384615384615419, 0.5641025641025640969, 0.5666666666666666519, 0.5692307692307692069, 0.5705128205128204844 ),
 .UNSPECIFIED. ) 
 CURVE ( )  GEOMETRIC_REPRESENTATION_ITEM ( )  RATIONAL_B_SPLINE_CURVE ( ( 0.9755282581475768211, 0.9755282581475768211, 1.000000000000000000, 0.9510565162951535312, 1.000000000000000000, 0.9510565162951535312, 1.000000000000000000, 0.9510565162951535312, 1.000000000000000000, 0.9510565162951535312, 1.000000000000000000, 0.9755282581475768211, 0.9755282581475768211 ) ) 
 REPRESENTATION_ITEM ( '' )  );
#27511 = CARTESIAN_POINT ( 'NONE',  ( 10.04305231718579705, 2.599999999999991207, 30.90933677959248982 ) ) ;
#27512 = ORIENTED_EDGE ( 'NONE', *, *, #17994, .T. ) ;
#27513 = CARTESIAN_POINT ( 'NONE',  ( 23.41746825000000243, 5.024999997268808194, 7.608796670333735079 ) ) ;
#27514 = DIRECTION ( 'NONE',  ( 0.5000000000000002220, 0.000000000000000000, 0.8660254037844384856 ) ) ;
#27515 = CARTESIAN_POINT ( 'NONE',  ( 24.20753774853756113, 44.51302083333331439, 13.97622843553589789 ) ) ;
#27516 =( BOUNDED_CURVE ( )  B_SPLINE_CURVE ( 2, ( #11056, #897, #24420, #16043, #11379, #26498, #18952, #3162, #19277, #14128, #16376, #11216, #29719 ),
 .UNSPECIFIED., .F., .T. ) 
 B_SPLINE_CURVE_WITH_KNOTS ( ( 3, 2, 2, 2, 2, 2, 3 ),
 ( 0.1602564102564102699, 0.1615384615384615474, 0.1641025641025641024, 0.1666666666666666574, 0.1692307692307692402, 0.1717948717948717952, 0.1730769230769230727 ),
 .UNSPECIFIED. ) 
 CURVE ( )  GEOMETRIC_REPRESENTATION_ITEM ( )  RATIONAL_B_SPLINE_CURVE ( ( 0.9755282581475768211, 0.9755282581475770431, 1.000000000000000000, 0.9510565162951535312, 1.000000000000000000, 0.9510565162951535312, 1.000000000000000000, 0.9510565162951535312, 1.000000000000000000, 0.9510565162951535312, 1.000000000000000000, 0.9755282581475768211, 0.9755282581475768211 ) ) 
 REPRESENTATION_ITEM ( '' )  );
#27517 = CARTESIAN_POINT ( 'NONE',  ( 33.58253175000000823, 64.02500000273118985, 10.91162601494192863 ) ) ;
#27518 = CARTESIAN_POINT ( 'NONE',  ( -10.37757302488624411, 22.97500000273118559, -31.93888565452638417 ) ) ;
#27519 = CARTESIAN_POINT ( 'NONE',  ( -33.58253175000000113, 17.27500000273118630, -10.91162601494193218 ) ) ;
#27520 = CARTESIAN_POINT ( 'NONE',  ( -10.37757302488623701, 9.775000002731182747, 31.93888565452638417 ) ) ;
#27521 = CARTESIAN_POINT ( 'NONE',  ( 20.47846945139902530, 11.71913166759064318, 20.53372385742071771 ) ) ;
#27522 = CARTESIAN_POINT ( 'NONE',  ( 20.50609665440969565, 54.10937499999999289, -20.50609665441004736 ) ) ;
#27523 = CARTESIAN_POINT ( 'NONE',  ( 11.25946833292375793, 80.57500000273121543, -8.180482586598735395 ) ) ;
#27524 = CARTESIAN_POINT ( 'NONE',  ( -20.08610463437156923, 46.29999999999999716, 27.64615127144130113 ) ) ;
#27525 = CARTESIAN_POINT ( 'NONE',  ( -10.37757302488624411, 54.72500000273117138, -31.93888565452638417 ) ) ;
#27526 = CARTESIAN_POINT ( 'NONE',  ( -7.236395654485763274, 18.52499999726881086, 22.27133577429736633 ) ) ;
#27527 = ORIENTED_EDGE ( 'NONE', *, *, #25377, .T. ) ;
#27528 = CARTESIAN_POINT ( 'NONE',  ( -20.75514604977248112, 63.67500000273116711, 28.56700777964554661 ) ) ;
#27529 = DIRECTION ( 'NONE',  ( -1.000000000000000000, 0.000000000000000000, 0.000000000000000000 ) ) ;
#27530 = AXIS2_PLACEMENT_3D ( 'NONE', #9753, #1510, #14910 ) ;
#27531 = CARTESIAN_POINT ( 'NONE',  ( -14.47279130897151589, 11.32499999726881157, -19.92008829642072598 ) ) ;
#27532 = CARTESIAN_POINT ( 'NONE',  ( -26.09010956794232428, 30.05246500092397000, 6.950374756619732253 ) ) ;
#27533 = ORIENTED_EDGE ( 'NONE', *, *, #24344, .T. ) ;
#27534 = CARTESIAN_POINT ( 'NONE',  ( 33.58253175000000823, 28.02500000273119340, 10.91162601494192863 ) ) ;
#27535 = AXIS2_PLACEMENT_3D ( 'NONE', #3366, #6098, #13836 ) ;
#27536 = CARTESIAN_POINT ( 'NONE',  ( 1.555960095263670572E-15, 6.499999999999994671, -24.50000000000000000 ) ) ;
#27537 = ORIENTED_EDGE ( 'NONE', *, *, #24981, .F. ) ;
#27538 = CARTESIAN_POINT ( 'NONE',  ( 7.505752307973351023, 62.13020833333334281, 28.01184896238290278 ) ) ;
#27539 = CARTESIAN_POINT ( 'NONE',  ( 20.75514604977249178, 62.07500000273118701, 28.56700777964553950 ) ) ;
#27540 = CARTESIAN_POINT ( 'NONE',  ( 10.04305231718579705, 69.10000000546237686, 30.90933677959248982 ) ) ;
#27541 = CARTESIAN_POINT ( 'NONE',  ( -10.37757302488624411, 64.72500000273117848, -31.93888565452638417 ) ) ;
#27542 = CARTESIAN_POINT ( 'NONE',  ( -28.01184896238304134, 28.90104166666666785, -7.505752307972844761 ) ) ;
#27543 = CARTESIAN_POINT ( 'NONE',  ( -19.82091636218621034, 8.800000000000002487, -14.40073868116559552 ) ) ;
#27544 = CARTESIAN_POINT ( 'NONE',  ( 6.486482029760649416E-15, 3.875000002731201931, 35.31076352940723240 ) ) ;
#27545 = CARTESIAN_POINT ( 'NONE',  ( 20.75514604977249178, 13.82500000273117813, 28.56700777964553950 ) ) ;
#27546 = CARTESIAN_POINT ( 'NONE',  ( -8.601468415847515203, 75.17500000273118133, 11.83890561707634959 ) ) ;
#27547 = CARTESIAN_POINT ( 'NONE',  ( 28.02196122052058413, 46.36940999907602645, 7.468012846824272799 ) ) ;
#27548 = CARTESIAN_POINT ( 'NONE',  ( 15.00000000000000355, 80.89999999999997726, 4.873795443493592394 ) ) ;
#27549 = CARTESIAN_POINT ( 'NONE',  ( 20.50609665440969565, 60.98437499999999289, -20.50609665441004736 ) ) ;
#27550 = CARTESIAN_POINT ( 'NONE',  ( -2.375766604868045029, 73.80125428700922896, -14.99999999999999822 ) ) ;
#27551 = CARTESIAN_POINT ( 'NONE',  ( -24.50000000000000355, 4.649999994537640902, -7.960532557706207157 ) ) ;
#27552 = CARTESIAN_POINT ( 'NONE',  ( 12.13525491562420910, 75.45000000546237118, -8.816778784387098611 ) ) ;
#27553 = CARTESIAN_POINT ( 'NONE',  ( -24.20753774853730889, 14.72135416666666607, 13.97622843553633842 ) ) ;
#27554 = CARTESIAN_POINT ( 'NONE',  ( 33.58253175000000823, 40.02500000273119696, 10.91162601494192863 ) ) ;
#27555 = CARTESIAN_POINT ( 'NONE',  ( 13.91746825000000065, 75.77500000273117564, 4.522059556121114987 ) ) ;
#27556 = CARTESIAN_POINT ( 'NONE',  ( 10.37757302488624767, 51.97500000273118559, 31.93888565452638417 ) ) ;
#27557 = CARTESIAN_POINT ( 'NONE',  ( 10.37757302488624056, 30.77500000273120051, -31.93888565452638417 ) ) ;
#27558 = CARTESIAN_POINT ( 'NONE',  ( 5.779280353836490358E-15, 40.49999999999999289, 32.49999999999999289 ) ) ;
#27559 = CIRCLE ( 'NONE', #22636, 27.00000000000000000 ) ;
#27560 = CARTESIAN_POINT ( 'NONE',  ( 19.09188309203661049, 33.48437500000000000, -19.09188309203694445 ) ) ;
#27561 = CARTESIAN_POINT ( 'NONE',  ( -31.91025403784435710, -18.96891108675448123, 0.000000000000000000 ) ) ;
#27562 = CARTESIAN_POINT ( 'NONE',  ( 0.000000000000000000, 74.00000000000001421, 15.00000000000000000 ) ) ;
#27563 = CARTESIAN_POINT ( 'NONE',  ( -32.50000000000000000, 68.09999999999995168, 10.55989012756946366 ) ) ;
#27564 = CARTESIAN_POINT ( 'NONE',  ( -4.523095164977117273E-15, 8.124999997268826490, 24.62258325217400312 ) ) ;
#27565 = CARTESIAN_POINT ( 'NONE',  ( -30.02300923189239867, 27.31993083240935505, 0.04044903255044988294 ) ) ;
#27566 = CARTESIAN_POINT ( 'NONE',  ( -23.41746825000000598, 2.224999997268808816, 7.608796670333726198 ) ) ;
#27567 = CARTESIAN_POINT ( 'NONE',  ( -26.06988505166722803, 37.48920166574269075, 7.025853678916877953 ) ) ;
#27568 = CARTESIAN_POINT ( 'NONE',  ( -33.58253175000000113, 77.47500000273120691, 10.91162601494193929 ) ) ;
#27569 = CARTESIAN_POINT ( 'NONE',  ( 20.75514604977248467, 10.42500000273119909, -28.56700777964554305 ) ) ;
#27570 = CARTESIAN_POINT ( 'NONE',  ( -14.47279130897152122, 14.42499999726880056, 19.92008829642072243 ) ) ;
#27571 = CARTESIAN_POINT ( 'NONE',  ( 13.97622843553589966, 60.84114583333332860, -24.20753774853756113 ) ) ;
#27572 = VERTEX_POINT ( 'NONE', #23930 ) ;
#27573 = CARTESIAN_POINT ( 'NONE',  ( -33.58253175000000113, 47.02500000273116854, -10.91162601494193218 ) ) ;
#27574 = CARTESIAN_POINT ( 'NONE',  ( -10.37757302488624411, 24.97500000273118914, -31.93888565452638417 ) ) ;
#27575 = ORIENTED_EDGE ( 'NONE', *, *, #28553, .T. ) ;
#27576 = CARTESIAN_POINT ( 'NONE',  ( 28.01184896238290278, 37.20833333333332860, -7.505752307973347470 ) ) ;
#27577 = CARTESIAN_POINT ( 'NONE',  ( -20.47846945139902175, 34.06288166759063785, -20.53372385742072481 ) ) ;
#27578 = CARTESIAN_POINT ( 'NONE',  ( -20.08610463437157989, 9.700000000000013500, -27.64615127144129758 ) ) ;
#27579 = CARTESIAN_POINT ( 'NONE',  ( 7.570916362186213000, 18.14999999453761959, -23.30088464923126423 ) ) ;
#27580 = CARTESIAN_POINT ( 'NONE',  ( 14.47279130897151767, 2.924999997268815655, -19.92008829642072598 ) ) ;
#27581 = CARTESIAN_POINT ( 'NONE',  ( -20.75514604977248112, 23.67500000273118843, 28.56700777964554661 ) ) ;
#27582 = CARTESIAN_POINT ( 'NONE',  ( 26.29305231718579350, 25.30000000546236905, 19.10302069950537529 ) ) ;
#27583 = CARTESIAN_POINT ( 'NONE',  ( 26.29305231718578995, 73.19999999999998863, -19.10302069950538240 ) ) ;
#27584 = DIRECTION ( 'NONE',  ( -0.000000000000000000, -1.000000000000000000, -0.000000000000000000 ) ) ;
#27585 = CARTESIAN_POINT ( 'NONE',  ( 32.49999999999965183, 66.90000000000001990, 10.55989012756993795 ) ) ;
#27586 = CARTESIAN_POINT ( 'NONE',  ( -0.04044903254990864921, 56.83631916759064495, 30.02300923189239867 ) ) ;
#27587 = CARTESIAN_POINT ( 'NONE',  ( -33.58253175000000113, 39.47500000273117848, 10.91162601494193929 ) ) ;
#27588 = CARTESIAN_POINT ( 'NONE',  ( -33.58253175000000113, 57.22500000273117848, 10.91162601494193929 ) ) ;
#27589 = CARTESIAN_POINT ( 'NONE',  ( 26.00068869287341045, 33.62760416666666430, -15.01150461594642493 ) ) ;
#27590 = CARTESIAN_POINT ( 'NONE',  ( -18.94512977948575738, 9.924999997268812990, -13.76444248337723231 ) ) ;
#27591 = CARTESIAN_POINT ( 'NONE',  ( -10.04305231718578462, 14.39999999999999680, 30.90933677959249337 ) ) ;
#27592 = CARTESIAN_POINT ( 'NONE',  ( -15.14183272437242600, 17.30000000000000782, 20.84094480462497856 ) ) ;
#27593 = CARTESIAN_POINT ( 'NONE',  ( -6.950374756619247307, 40.35378499907601935, 26.09010956794245217 ) ) ;
#27594 = CARTESIAN_POINT ( 'NONE',  ( -33.58253175000000113, 55.22500000273117848, 10.91162601494193929 ) ) ;
#27595 = CARTESIAN_POINT ( 'NONE',  ( -27.16883889988623935, 49.57500000273118701, 19.73931689729374739 ) ) ;
#27596 = CARTESIAN_POINT ( 'NONE',  ( -18.94512977948575738, 11.42499999726881477, -13.76444248337723231 ) ) ;
#27597 = EDGE_CURVE ( 'NONE', #5367, #4913, #32122, .T. ) ;
#27598 = LINE ( 'NONE', #14563, #14479 ) ;
#27599 = CARTESIAN_POINT ( 'NONE',  ( -13.94119854578936923, 51.39361083425730925, -24.22776226481241224 ) ) ;
#27600 = CARTESIAN_POINT ( 'NONE',  ( -21.69117583031640351, 16.99999999999999289, -10.83878137934375374 ) ) ;
#27601 = CARTESIAN_POINT ( 'NONE',  ( -31.92269207768538308, 51.99999999999999289, 6.710300343870669870 ) ) ;
#27602 = CARTESIAN_POINT ( 'NONE',  ( 20.75514604977249178, 19.82500000273119412, 28.56700777964553950 ) ) ;
#27603 = FACE_OUTER_BOUND ( 'NONE', #30785, .T. ) ;
#27604 = CARTESIAN_POINT ( 'NONE',  ( 10.04305231718579705, 52.60000000000002274, 30.90933677959248982 ) ) ;
#27605 = CONICAL_SURFACE ( 'NONE', #2408, 24.49999999999999645, 1.047197551196593412 ) ;
#27606 = AXIS2_PLACEMENT_3D ( 'NONE', #22743, #22566, #4548 ) ;
#27607 = EDGE_CURVE ( 'NONE', #25303, #6411, #5563, .T. ) ;
#27608 = CARTESIAN_POINT ( 'NONE',  ( 32.50000000000000000, 41.50000000546238965, -3.980102097228898626E-15 ) ) ;
#27609 = ADVANCED_FACE ( 'NONE', ( #3651 ), #31802, .T. ) ;
#27610 = CARTESIAN_POINT ( 'NONE',  ( 0.04044903255045854962, 67.71055583240935505, 30.02300923189239867 ) ) ;
#27611 = CARTESIAN_POINT ( 'NONE',  ( -20.08610463437157989, 44.20000000546238539, -27.64615127144129758 ) ) ;
#27612 =( BOUNDED_CURVE ( )  B_SPLINE_CURVE ( 2, ( #31620, #23576, #385, #8118, #29044, #10870, #31786, #29213, #26651, #3146, #23238, #31119, #16360 ),
 .UNSPECIFIED., .F., .T. ) 
 B_SPLINE_CURVE_WITH_KNOTS ( ( 3, 2, 2, 2, 2, 2, 3 ),
 ( 0.2756410256410256610, 0.2769230769230769384, 0.2794871794871794934, 0.2820512820512820484, 0.2846153846153846034, 0.2871794871794871584, 0.2884615384615384914 ),
 .UNSPECIFIED. ) 
 CURVE ( )  GEOMETRIC_REPRESENTATION_ITEM ( )  RATIONAL_B_SPLINE_CURVE ( ( 0.9755282581475768211, 0.9755282581475768211, 1.000000000000000000, 0.9510565162951535312, 1.000000000000000000, 0.9510565162951535312, 1.000000000000000000, 0.9510565162951535312, 1.000000000000000000, 0.9510565162951535312, 1.000000000000000000, 0.9755282581475762660, 0.9755282581475768211 ) ) 
 REPRESENTATION_ITEM ( '' )  );
#27613 = CARTESIAN_POINT ( 'NONE',  ( 26.29305231718578995, 35.20000000000000995, -19.10302069950538240 ) ) ;
#27614 = CARTESIAN_POINT ( 'NONE',  ( 33.58253175000000823, 32.02500000273118985, 10.91162601494192685 ) ) ;
#27615 = CARTESIAN_POINT ( 'NONE',  ( 19.09188309203661049, 36.92187499999999289, -19.09188309203694445 ) ) ;
#27616 = ORIENTED_EDGE ( 'NONE', *, *, #29497, .T. ) ;
#27617 = EDGE_CURVE ( 'NONE', #12770, #22201, #27516, .T. ) ;
#27618 = CARTESIAN_POINT ( 'NONE',  ( 33.58253175000000113, 78.12500000273118417, -4.112674001490185761E-15 ) ) ;
#27619 = CARTESIAN_POINT ( 'NONE',  ( 20.50609665441005092, 37.78124999999999289, 20.50609665440969209 ) ) ;
#27620 = DIRECTION ( 'NONE',  ( -0.000000000000000000, 1.000000000000000000, -0.000000000000000000 ) ) ;
#27621 = ORIENTED_EDGE ( 'NONE', *, *, #10902, .F. ) ;
#27622 = CARTESIAN_POINT ( 'NONE',  ( 15.04653450569292872, 48.52902750092398065, -25.98046417659857710 ) ) ;
#27623 = CARTESIAN_POINT ( 'NONE',  ( -26.29305231718579350, 10.30000000546237082, -19.10302069950537884 ) ) ;
#27624 = CARTESIAN_POINT ( 'NONE',  ( 15.01150461594643204, 65.42447916666667140, 26.00068869287340334 ) ) ;
#27625 = LINE ( 'NONE', #32920, #5901 ) ;
#27626 = CARTESIAN_POINT ( 'NONE',  ( 27.16883889988623935, 40.57500000273117280, -19.73931689729374384 ) ) ;
#27627 = CARTESIAN_POINT ( 'NONE',  ( -20.08610463437157989, 44.20000000546238539, -27.64615127144129758 ) ) ;
#27628 = CARTESIAN_POINT ( 'NONE',  ( 2.688165632520823219E-15, 71.87500000273116996, 14.63369212191046387 ) ) ;
#27629 = CARTESIAN_POINT ( 'NONE',  ( 10.37757302488624767, 27.72500000273120335, 31.93888565452638417 ) ) ;
#27630 = CARTESIAN_POINT ( 'NONE',  ( 1.555960095263670572E-15, 14.24999999453762278, -24.50000000000000000 ) ) ;
#27631 = VECTOR ( 'NONE', #23412, 1000.000000000000227 ) ;
#27632 = CARTESIAN_POINT ( 'NONE',  ( 6.486482029760649416E-15, 55.87500000273118417, 35.31076352940723240 ) ) ;
#27633 = CARTESIAN_POINT ( 'NONE',  ( -26.29305231718578995, 34.19999999999999574, 19.10302069950538595 ) ) ;
#27634 = CARTESIAN_POINT ( 'NONE',  ( 32.50000000000000000, 37.00000000000000711, -3.980102097228898626E-15 ) ) ;
#27635 = CARTESIAN_POINT ( 'NONE',  ( -18.94512977948576093, 9.824999997268824004, 13.76444248337722698 ) ) ;
#27636 = CARTESIAN_POINT ( 'NONE',  ( 33.58253175000000113, 78.12500000273119838, -4.112674001490185761E-15 ) ) ;
#27637 = DIRECTION ( 'NONE',  ( 0.000000000000000000, 0.000000000000000000, -1.000000000000000000 ) ) ;
#27638 = CARTESIAN_POINT ( 'NONE',  ( -8.960552108402744065E-16, 78.87500000273118417, -14.63369212191046209 ) ) ;
#27639 = CARTESIAN_POINT ( 'NONE',  ( -20.75514604977248823, 69.07500000273117280, -28.56700777964554305 ) ) ;
#27640 = CARTESIAN_POINT ( 'NONE',  ( -12.13525491562420910, 74.45000000546237118, 8.816778784387098611 ) ) ;
#27641 = ORIENTED_EDGE ( 'NONE', *, *, #23201, .F. ) ;
#27642 = PRODUCT ( 'plain washer hardened_iso_Washer ISO 7415 - 30', 'plain washer hardened_iso_Washer ISO 7415 - 30', '', ( #7717 ) ) ;
#27643 = CARTESIAN_POINT ( 'NONE',  ( -15.14183272437241889, 6.449999994537612302, -20.84094480462497856 ) ) ;
#27644 = CARTESIAN_POINT ( 'NONE',  ( 26.09010956794232428, 21.45871500092397355, -6.950374756619718042 ) ) ;
#27645 = CARTESIAN_POINT ( 'NONE',  ( -2.375766604868041476, 74.69874572391553613, 14.99999999999999822 ) ) ;
#27646 = CARTESIAN_POINT ( 'NONE',  ( 20.75514604977248467, 40.42500000273117422, -28.56700777964554305 ) ) ;
#27647 = CARTESIAN_POINT ( 'NONE',  ( -33.58253175000000113, 5.375000002731181503, 0.000000000000000000 ) ) ;
#27648 = CARTESIAN_POINT ( 'NONE',  ( 10.37757302488624056, 58.77500000273121117, -31.93888565452638417 ) ) ;
#27649 = CARTESIAN_POINT ( 'NONE',  ( -26.07999730980477437, 56.11458333333332860, 6.988114217768305103 ) ) ;
#27650 = CARTESIAN_POINT ( 'NONE',  ( -7.468012846824771955, 41.22434000092397355, -28.02196122052045624 ) ) ;
#27651 = CARTESIAN_POINT ( 'NONE',  ( -28.02196122052058413, 34.33815999907601224, -7.468012846824272799 ) ) ;
#27652 = CARTESIAN_POINT ( 'NONE',  ( -26.29305231718579350, 64.30000000546236549, -19.10302069950537884 ) ) ;
#27653 = CARTESIAN_POINT ( 'NONE',  ( 11.25946833292375793, 75.67500000273119554, 8.180482586598731842 ) ) ;
#27654 = CARTESIAN_POINT ( 'NONE',  ( -7.025853678916861966, 52.09857666574269075, -26.06988505166722803 ) ) ;
#27655 = CARTESIAN_POINT ( 'NONE',  ( 5.779280353836490358E-15, 58.49999999999999289, 32.49999999999999289 ) ) ;
#27656 = CARTESIAN_POINT ( 'NONE',  ( -7.505752307973343918, 12.28645833333333037, -28.01184896238290989 ) ) ;
#27657 = EDGE_CURVE ( 'NONE', #27368, #22684, #25357, .T. ) ;
#27658 = CARTESIAN_POINT ( 'NONE',  ( -33.58253175000000113, 43.37500000273118417, 0.000000000000000000 ) ) ;
#27659 = CARTESIAN_POINT ( 'NONE',  ( 18.94512977948576093, 1.324999997268816454, -13.76444248337722875 ) ) ;
#27660 = EDGE_LOOP ( 'NONE', ( #25166, #3794 ) ) ;
#27661 = CARTESIAN_POINT ( 'NONE',  ( -20.08610463437157989, 30.20000000546236407, -27.64615127144129758 ) ) ;
#27662 = ORIENTED_EDGE ( 'NONE', *, *, #30013, .T. ) ;
#27663 = CARTESIAN_POINT ( 'NONE',  ( 2.740863092043355209E-13, 34.77343750000000000, 30.02300923189239512 ) ) ;
#27664 = ORIENTED_EDGE ( 'NONE', *, *, #33257, .F. ) ;
#27665 = CARTESIAN_POINT ( 'NONE',  ( 5.147494310547643614, 27.44874571845315714, -32.49999999999992895 ) ) ;
#27666 = CARTESIAN_POINT ( 'NONE',  ( 33.58253175000000823, 50.02500000273118985, 10.91162601494192863 ) ) ;
#27667 = CARTESIAN_POINT ( 'NONE',  ( 32.50000000000000000, 55.50000000546237544, -3.980102097228898626E-15 ) ) ;
#27668 = CARTESIAN_POINT ( 'NONE',  ( -20.50609665440969209, 66.14062500000000000, 20.50609665441005092 ) ) ;
#27669 = CARTESIAN_POINT ( 'NONE',  ( -10.04305231718579172, 14.10000000546238219, -30.90933677959248982 ) ) ;
#27670 = CARTESIAN_POINT ( 'NONE',  ( -20.75514604977248112, 65.42500000273116711, 28.56700777964554661 ) ) ;
#27671 = CARTESIAN_POINT ( 'NONE',  ( 14.47279130897151767, 16.82499999726881157, 19.92008829642072953 ) ) ;
#27672 = MECHANICAL_DESIGN_GEOMETRIC_PRESENTATION_REPRESENTATION (  '', ( #18367 ), #7940 ) ;
#27673 = CARTESIAN_POINT ( 'NONE',  ( 32.50000000000000711, 50.89999999999999858, 10.55989012756945122 ) ) ;
#27674 = DIRECTION ( 'NONE',  ( -1.224646799147353454E-16, 1.000000000000000000, -0.000000000000000000 ) ) ;
#27675 = CARTESIAN_POINT ( 'NONE',  ( 27.16883889988624290, 14.17500000273119731, 19.73931689729373673 ) ) ;
#27676 =( NAMED_UNIT ( * ) SI_UNIT ( $, .STERADIAN. ) SOLID_ANGLE_UNIT ( ) );
#27677 = CARTESIAN_POINT ( 'NONE',  ( -26.06988505166722803, 23.73920166574268364, 7.025853678916877953 ) ) ;
#27678 = CARTESIAN_POINT ( 'NONE',  ( -8.601468415847515203, 73.17500000273119554, 11.83890561707634959 ) ) ;
#27679 = CARTESIAN_POINT ( 'NONE',  ( -4.223320258572819786E-15, 13.50000000000000355, 24.50000000000000000 ) ) ;
#27680 = CYLINDRICAL_SURFACE ( 'NONE', #5152, 32.50000000000000000 ) ;
#27681 = CARTESIAN_POINT ( 'NONE',  ( 26.29305231718579350, 6.800000000000000711, 19.10302069950537529 ) ) ;
#27682 = ORIENTED_EDGE ( 'NONE', *, *, #4526, .T. ) ;
#27683 = CARTESIAN_POINT ( 'NONE',  ( 23.41746824999999887, 5.124999997268814056, 0.000000000000000000 ) ) ;
#27684 = CARTESIAN_POINT ( 'NONE',  ( 11.25946833292375793, 72.07500000273120122, -8.180482586598735395 ) ) ;
#27685 = CARTESIAN_POINT ( 'NONE',  ( -19.09188309203660694, 45.51562500000000000, 19.09188309203694800 ) ) ;
#27686 = CARTESIAN_POINT ( 'NONE',  ( -33.58253175000000113, 65.22500000273117848, 10.91162601494193929 ) ) ;
#27687 = CARTESIAN_POINT ( 'NONE',  ( -2.162160676586881955E-15, 24.87500000273117351, -35.31076352940723240 ) ) ;
#27688 = CARTESIAN_POINT ( 'NONE',  ( -33.58253175000000113, 7.275000002731196957, -10.91162601494193218 ) ) ;
#27689 = CARTESIAN_POINT ( 'NONE',  ( -33.58253175000000113, 11.27500000273117209, -10.91162601494193041 ) ) ;
#27690 = CARTESIAN_POINT ( 'NONE',  ( 7.468012846824777284, 15.44309000092397355, 28.02196122052045268 ) ) ;
#27691 = CARTESIAN_POINT ( 'NONE',  ( 7.505752307972854531, 53.82291666666666430, -28.01184896238303423 ) ) ;
#27692 = CARTESIAN_POINT ( 'NONE',  ( 13.91746824999999887, 72.37500000273119838, -1.704398294459741270E-15 ) ) ;
#27693 = CARTESIAN_POINT ( 'NONE',  ( -10.04305231718579172, 45.60000000000001563, -30.90933677959248982 ) ) ;
#27694 = VECTOR ( 'NONE', #8355, 1000.000000000000000 ) ;
#27695 = CARTESIAN_POINT ( 'NONE',  ( 6.486482029760648627E-15, 53.62500000273120548, 35.31076352940722529 ) ) ;
#27696 = CARTESIAN_POINT ( 'NONE',  ( -23.41746825000000598, 5.724999997268815477, 7.608796670333726198 ) ) ;
#27697 = CONICAL_SURFACE ( 'NONE', #26609, 13.32050807568876927, 0.2617993877991500740 ) ;
#27698 = EDGE_LOOP ( 'NONE', ( #13956, #16127, #11783, #5844 ) ) ;
#27699 = CARTESIAN_POINT ( 'NONE',  ( 33.58253175000000113, 58.37500000273119838, -4.112674001490185761E-15 ) ) ;
#27700 = DIRECTION ( 'NONE',  ( -0.000000000000000000, -1.000000000000000000, -0.000000000000000000 ) ) ;
#27701 = CARTESIAN_POINT ( 'NONE',  ( -7.236395654485757944, 13.22499999726881015, -22.27133577429736988 ) ) ;
#27702 = CARTESIAN_POINT ( 'NONE',  ( -6.950374756619716266, 30.91184000092396644, -26.09010956794232428 ) ) ;
#27703 = EDGE_CURVE ( 'NONE', #7457, #7617, #6724, .T. ) ;
#27704 = ORIENTED_EDGE ( 'NONE', *, *, #12358, .T. ) ;
#27705 = CARTESIAN_POINT ( 'NONE',  ( -33.58253175000000113, 33.12500000273120548, 0.000000000000000000 ) ) ;
#27706 = FACE_OUTER_BOUND ( 'NONE', #24614, .T. ) ;
#27707 = ORIENTED_EDGE ( 'NONE', *, *, #25513, .F. ) ;
#27708 = CARTESIAN_POINT ( 'NONE',  ( -7.505752307972844761, 62.41666666666666430, 28.01184896238304134 ) ) ;
#27709 = CARTESIAN_POINT ( 'NONE',  ( -33.58253175000000113, 57.27500000273120406, -10.91162601494193218 ) ) ;
#27710 = CARTESIAN_POINT ( 'NONE',  ( 8.305033359366087120E-16, -29.78157438140398483, 0.000000000000000000 ) ) ;
#27711 = CARTESIAN_POINT ( 'NONE',  ( -27.16883889988624290, 68.92500000273119554, -19.73931689729374028 ) ) ;
#27712 = CARTESIAN_POINT ( 'NONE',  ( -7.505752307973343918, 32.91145833333332860, -28.01184896238290989 ) ) ;
#27713 =( BOUNDED_CURVE ( )  B_SPLINE_CURVE ( 2, ( #7402, #7055, #9632, #17199, #20457, #30908, #33309, #30384, #14961, #25601, #12032, #17888, #15137 ),
 .UNSPECIFIED., .F., .T. ) 
 B_SPLINE_CURVE_WITH_KNOTS ( ( 3, 2, 2, 2, 2, 2, 3 ),
 ( 0.2500000000000000000, 0.2600000000000000089, 0.2800000000000000266, 0.2999999999999999889, 0.3200000000000000067, 0.3400000000000000244, 0.3500000000000000333 ),
 .UNSPECIFIED. ) 
 CURVE ( )  GEOMETRIC_REPRESENTATION_ITEM ( )  RATIONAL_B_SPLINE_CURVE ( ( 0.9755282581475768211, 0.9755282581475768211, 1.000000000000000000, 0.9510565162951535312, 1.000000000000000000, 0.9510565162951535312, 1.000000000000000000, 0.9510565162951535312, 1.000000000000000000, 0.9510565162951535312, 1.000000000000000000, 0.9755282581475767101, 0.9755282581475768211 ) ) 
 REPRESENTATION_ITEM ( '' )  );
#27714 = CARTESIAN_POINT ( 'NONE',  ( -7.570916362186215665, 15.39999999999999680, 23.30088464923126423 ) ) ;
#27715 = CARTESIAN_POINT ( 'NONE',  ( 10.37757302488624056, 2.775000002731176085, -31.93888565452638417 ) ) ;
#27716 = CARTESIAN_POINT ( 'NONE',  ( 27.16883889988624290, 11.92500000273116711, 19.73931689729373673 ) ) ;
#27717 = CARTESIAN_POINT ( 'NONE',  ( 13.91746824999999887, 71.87500000273119838, -1.704398294459741270E-15 ) ) ;
#27718 = CARTESIAN_POINT ( 'NONE',  ( 28.02196122052058413, 53.24440999907603356, 7.468012846824272799 ) ) ;
#27719 = CARTESIAN_POINT ( 'NONE',  ( -12.13525491562421088, 75.80000000000001137, -8.816778784387096835 ) ) ;
#27720 = CARTESIAN_POINT ( 'NONE',  ( 28.01184896238290278, 54.39583333333332860, -7.505752307973347470 ) ) ;
#27721 = CARTESIAN_POINT ( 'NONE',  ( 5.147494310547426899, 55.44874571845314648, -32.50000000000000000 ) ) ;
#27722 = CARTESIAN_POINT ( 'NONE',  ( 32.50000000000000000, 22.99999999999999289, -3.980102097228898626E-15 ) ) ;
#27723 = CARTESIAN_POINT ( 'NONE',  ( -15.14183272437242600, 7.049999994537622605, 20.84094480462497856 ) ) ;
#27724 = CARTESIAN_POINT ( 'NONE',  ( 12.13525491562420910, 79.45000000546237118, -8.816778784387098611 ) ) ;
#27725 = CARTESIAN_POINT ( 'NONE',  ( -26.07999730980477437, 14.86458333333333037, 6.988114217768305103 ) ) ;
#27726 = CARTESIAN_POINT ( 'NONE',  ( -33.58253175000000113, 39.22500000273119269, 10.91162601494193929 ) ) ;
#27727 = CARTESIAN_POINT ( 'NONE',  ( -13.91746824999999887, 72.87500000273122680, 0.000000000000000000 ) ) ;
#27728 = CARTESIAN_POINT ( 'NONE',  ( -2.162160676586881955E-15, 40.87500000273119838, -35.31076352940723240 ) ) ;
#27729 = CARTESIAN_POINT ( 'NONE',  ( 33.58253175000000113, 26.47500000273118559, -10.91162601494193574 ) ) ;
#27730 = CARTESIAN_POINT ( 'NONE',  ( -3.880418787951136483, 16.30125427608446742, -24.50000000000000000 ) ) ;
#27731 = CARTESIAN_POINT ( 'NONE',  ( 7.570916362186213000, 2.400000000000013234, -23.30088464923126423 ) ) ;
#27732 = CARTESIAN_POINT ( 'NONE',  ( 32.50000000000000711, 32.89999999999997726, 10.55989012756945122 ) ) ;
#27733 = CARTESIAN_POINT ( 'NONE',  ( 10.04305231718579705, 66.60000000000000853, 30.90933677959248982 ) ) ;
#27734 = AXIS2_PLACEMENT_3D ( 'NONE', #18077, #13089, #18423 ) ;
#27735 = CARTESIAN_POINT ( 'NONE',  ( -18.94512977948576093, 7.824999997268822227, 13.76444248337722698 ) ) ;
#27736 = CARTESIAN_POINT ( 'NONE',  ( -30.02300923189239867, 23.88243083240935505, 0.04044903255044988294 ) ) ;
#27737 = CARTESIAN_POINT ( 'NONE',  ( -26.09010956794245217, 34.33815999907601224, -6.950374756619243755 ) ) ;
#27738 = CARTESIAN_POINT ( 'NONE',  ( 33.58253175000000113, 14.22500000273119447, -10.91162601494193574 ) ) ;
#27739 = CARTESIAN_POINT ( 'NONE',  ( 1.507698388325705758E-15, 9.624999997268808727, -24.62258325217400312 ) ) ;
#27740 = CARTESIAN_POINT ( 'NONE',  ( 6.988114217767829928, 64.13541666666667140, -26.07999730980489872 ) ) ;
#27741 = ORIENTED_EDGE ( 'NONE', *, *, #28451, .F. ) ;
#27742 = CARTESIAN_POINT ( 'NONE',  ( -33.58253175000000113, 49.12500000273119127, 0.000000000000000000 ) ) ;
#27743 = CARTESIAN_POINT ( 'NONE',  ( 27.16883889988624290, 22.17500000273119198, 19.73931689729373673 ) ) ;
#27744 = EDGE_CURVE ( 'NONE', #24826, #6976, #10573, .T. ) ;
#27745 = EDGE_CURVE ( 'NONE', #15993, #18611, #23620, .T. ) ;
#27746 = ORIENTED_EDGE ( 'NONE', *, *, #6975, .T. ) ;
#27747 = CARTESIAN_POINT ( 'NONE',  ( 7.505752307972854531, 33.19791666666665719, -28.01184896238303423 ) ) ;
#27748 = CARTESIAN_POINT ( 'NONE',  ( -0.04044903254990864921, 32.77381916759064495, 30.02300923189239867 ) ) ;
#27749 = CARTESIAN_POINT ( 'NONE',  ( -7.570916362186215665, 3.399999999999986144, 23.30088464923126423 ) ) ;
#27750 = CARTESIAN_POINT ( 'NONE',  ( -24.50000000000000355, 14.64999999453761603, -7.960532557706207157 ) ) ;
#27751 = CARTESIAN_POINT ( 'NONE',  ( -14.47279130897151589, 11.32499999726881157, -19.92008829642072598 ) ) ;
#27752 = CARTESIAN_POINT ( 'NONE',  ( -10.37757302488623701, 21.77500000273119340, 31.93888565452638417 ) ) ;
#27753 = CARTESIAN_POINT ( 'NONE',  ( -20.08610463437156923, 22.80000000546236194, 27.64615127144130113 ) ) ;
#27754 = CARTESIAN_POINT ( 'NONE',  ( -26.29305231718579350, 69.79999999999999716, -19.10302069950537884 ) ) ;
#27755 = CARTESIAN_POINT ( 'NONE',  ( 0.000000000000000000, 80.00000000000001421, 0.000000000000000000 ) ) ;
#27756 = CARTESIAN_POINT ( 'NONE',  ( 10.04305231718579705, 66.60000000000000853, 30.90933677959248982 ) ) ;
#27757 = CARTESIAN_POINT ( 'NONE',  ( -20.53372385742071771, 53.82850666759064495, 20.47846945139902530 ) ) ;
#27758 = CARTESIAN_POINT ( 'NONE',  ( -33.58253175000000113, 35.37500000273119127, 0.000000000000000000 ) ) ;
#27759 = CARTESIAN_POINT ( 'NONE',  ( -10.37757302488624411, 56.72500000273118559, -31.93888565452638417 ) ) ;
#27760 = CARTESIAN_POINT ( 'NONE',  ( 15.01150461594596486, 29.90364583333332860, -26.00068869287367690 ) ) ;
#27761 = CARTESIAN_POINT ( 'NONE',  ( 0.000000000000000000, 0.000000000000000000, 0.000000000000000000 ) ) ;
#27762 = CIRCLE ( 'NONE', #16274, 15.31642273298461276 ) ;
#27763 = CARTESIAN_POINT ( 'NONE',  ( -14.47279130897151589, 7.824999997268807128, -19.92008829642072598 ) ) ;
#27764 = CARTESIAN_POINT ( 'NONE',  ( 20.08610463437158344, 16.69999999999999574, 27.64615127144129403 ) ) ;
#27765 = CARTESIAN_POINT ( 'NONE',  ( 19.82091636218621389, 16.19999999999999218, -14.40073868116559197 ) ) ;
#27766 = EDGE_CURVE ( 'NONE', #7617, #11830, #29723, .T. ) ;
#27767 = CARTESIAN_POINT ( 'NONE',  ( 7.025853678916867295, 40.06732666574268364, 26.06988505166722803 ) ) ;
#27768 = CARTESIAN_POINT ( 'NONE',  ( 33.58253175000000113, 58.12500000273118417, -4.112674001490185761E-15 ) ) ;
#27769 = CARTESIAN_POINT ( 'NONE',  ( -10.37757302488623701, 49.77500000273118985, 31.93888565452638417 ) ) ;
#27770 = CARTESIAN_POINT ( 'NONE',  ( 20.08610463437157279, 45.29999999999999005, -27.64615127144129758 ) ) ;
#27771 = CARTESIAN_POINT ( 'NONE',  ( 5.779280353836490358E-15, 56.49999999999998579, 32.49999999999999289 ) ) ;
#27772 = CARTESIAN_POINT ( 'NONE',  ( -30.91025403784432513, -20.70096189432334910, 3.785414366827760066E-15 ) ) ;
#27773 = CARTESIAN_POINT ( 'NONE',  ( 6.950374756619721595, 49.81809000092397355, 26.09010956794232428 ) ) ;
#27774 = CARTESIAN_POINT ( 'NONE',  ( 26.29305231718579350, 63.30000000546235839, 19.10302069950537529 ) ) ;
#27775 = CARTESIAN_POINT ( 'NONE',  ( 0.000000000000000000, 80.00000000000001421, 0.000000000000000000 ) ) ;
#27776 = CARTESIAN_POINT ( 'NONE',  ( -33.58253175000000113, 23.02500000273117919, -10.91162601494193218 ) ) ;
#27777 = PLANE ( 'NONE',  #2350 ) ;
#27778 = CARTESIAN_POINT ( 'NONE',  ( 32.50000000000000711, 52.89999999999999147, 10.55989012756945122 ) ) ;
#27779 = DIRECTION ( 'NONE',  ( -0.000000000000000000, -1.000000000000000000, -0.000000000000000000 ) ) ;
#27780 = CARTESIAN_POINT ( 'NONE',  ( -7.468012846824272799, 60.97878499907603356, 28.02196122052058413 ) ) ;
#27781 = CARTESIAN_POINT ( 'NONE',  ( -20.08610463437156923, 42.80000000546236549, 27.64615127144130113 ) ) ;
#27782 = CARTESIAN_POINT ( 'NONE',  ( 4.635254915624209993, 71.65000000546240244, -14.26584774442730463 ) ) ;
#27783 = CARTESIAN_POINT ( 'NONE',  ( 10.37757302488624767, 31.72500000273117848, 31.93888565452638417 ) ) ;
#27784 = CARTESIAN_POINT ( 'NONE',  ( 27.16883889988624290, 64.17500000273118133, 19.73931689729373673 ) ) ;
#27785 = CARTESIAN_POINT ( 'NONE',  ( 19.09188309203694800, 30.90624999999999645, 19.09188309203660694 ) ) ;
#27786 = ORIENTED_EDGE ( 'NONE', *, *, #1803, .F. ) ;
#27787 = CARTESIAN_POINT ( 'NONE',  ( 20.75514604977249178, 67.82500000273120122, 28.56700777964553950 ) ) ;
#27788 = VECTOR ( 'NONE', #27015, 999.9999999999998863 ) ;
#27789 = CARTESIAN_POINT ( 'NONE',  ( 30.02300923189239512, 44.22656249999997868, -2.619432448724977703E-13 ) ) ;
#27790 = CARTESIAN_POINT ( 'NONE',  ( -26.50000000000000000, -15.84529946162075653, 3.576596532241492659E-15 ) ) ;
#27791 = EDGE_LOOP ( 'NONE', ( #10247, #9638 ) ) ;
#27792 = CARTESIAN_POINT ( 'NONE',  ( 20.47846945139902530, 59.84413166759065206, 20.53372385742071771 ) ) ;
#27793 = CARTESIAN_POINT ( 'NONE',  ( 26.06988505166735592, 59.55767333425731636, 7.025853678916393896 ) ) ;
#27794 = CARTESIAN_POINT ( 'NONE',  ( 33.58253175000000113, 8.225000002731182036, -10.91162601494193751 ) ) ;
#27795 = VECTOR ( 'NONE', #2734, 1000.000000000000000 ) ;
#27796 = CARTESIAN_POINT ( 'NONE',  ( -20.50609665441004736, 60.12500000000000000, -20.50609665440969565 ) ) ;
#27797 = CARTESIAN_POINT ( 'NONE',  ( 10.04305231718578817, 21.40000000000000213, -30.90933677959249337 ) ) ;
#27798 = CARTESIAN_POINT ( 'NONE',  ( 20.75514604977248467, 40.67500000273116711, -28.56700777964554305 ) ) ;
#27799 = CARTESIAN_POINT ( 'NONE',  ( -26.29305231718578995, 46.70000000546237118, 19.10302069950538595 ) ) ;
#27800 = CARTESIAN_POINT ( 'NONE',  ( 13.91746825000000065, 74.27500000273120406, 4.522059556121114987 ) ) ;
#27801 = CARTESIAN_POINT ( 'NONE',  ( 20.75514604977248467, 30.42500000273117777, -28.56700777964554305 ) ) ;
#27802 = CARTESIAN_POINT ( 'NONE',  ( 24.50000000000000000, 13.84999999453764197, -7.960532557706203605 ) ) ;
#27803 = CARTESIAN_POINT ( 'NONE',  ( 27.16883889988624290, 58.17500000273118133, 19.73931689729373673 ) ) ;
#27804 = CARTESIAN_POINT ( 'NONE',  ( 6.277390505771533514E-15, 38.50000000000000711, 34.17252228774368916 ) ) ;
#27805 = CARTESIAN_POINT ( 'NONE',  ( 32.50000000000000000, 35.00000000000000000, -3.980102097228898626E-15 ) ) ;
#27806 = CARTESIAN_POINT ( 'NONE',  ( 7.570916362186213000, 0.4000000000000114575, -23.30088464923126423 ) ) ;
#27807 = CARTESIAN_POINT ( 'NONE',  ( 33.58253175000000113, 74.22500000273119269, -10.91162601494193751 ) ) ;
#27808 = LINE ( 'NONE', #22655, #3061 ) ;
#27809 = CARTESIAN_POINT ( 'NONE',  ( 2.688165632520823219E-15, 75.87500000273115575, 14.63369212191046209 ) ) ;
#27810 = CARTESIAN_POINT ( 'NONE',  ( 20.75514604977248467, 66.67500000273119554, -28.56700777964554305 ) ) ;
#27811 = CARTESIAN_POINT ( 'NONE',  ( 4.635254915624212657, 76.85000000546237686, 14.26584774442730286 ) ) ;
#27812 = EDGE_CURVE ( 'NONE', #15526, #31469, #30815, .T. ) ;
#27813 = ORIENTED_EDGE ( 'NONE', *, *, #16089, .T. ) ;
#27814 = CARTESIAN_POINT ( 'NONE',  ( 19.82091636218621389, 11.94999999453763628, -14.40073868116559197 ) ) ;
#27815 = CARTESIAN_POINT ( 'NONE',  ( 0.04044903254993986036, 24.18006916759064140, -27.95245687107223986 ) ) ;
#27816 =( BOUNDED_CURVE ( )  B_SPLINE_CURVE ( 2, ( #23657, #28285, #4772, #5458, #15939, #26395, #23135, #2888, #15600, #25877, #10274, #15250, #18006 ),
 .UNSPECIFIED., .F., .T. ) 
 B_SPLINE_CURVE_WITH_KNOTS ( ( 3, 2, 2, 2, 2, 2, 3 ),
 ( 0.3397435897435897578, 0.3410256410256410353, 0.3435897435897435903, 0.3461538461538461453, 0.3487179487179487003, 0.3512820512820512553, 0.3525641025641025883 ),
 .UNSPECIFIED. ) 
 CURVE ( )  GEOMETRIC_REPRESENTATION_ITEM ( )  RATIONAL_B_SPLINE_CURVE ( ( 0.9755282581475768211, 0.9755282581475768211, 1.000000000000000000, 0.9510565162951535312, 1.000000000000000000, 0.9510565162951535312, 1.000000000000000000, 0.9510565162951535312, 1.000000000000000000, 0.9510565162951535312, 1.000000000000000000, 0.9755282581475762660, 0.9755282581475768211 ) ) 
 REPRESENTATION_ITEM ( '' )  );
#27817 = CARTESIAN_POINT ( 'NONE',  ( 0.000000000000000000, 70.00000000000000000, -30.50000000000000000 ) ) ;
#27818 = CARTESIAN_POINT ( 'NONE',  ( 20.75514604977249178, 43.82500000273119412, 28.56700777964553950 ) ) ;
#27819 = CARTESIAN_POINT ( 'NONE',  ( 33.58253175000000113, 4.475000002731183812, -10.91162601494193751 ) ) ;
#27820 = CARTESIAN_POINT ( 'NONE',  ( -27.16883889988623935, 57.57500000273117990, 19.73931689729374739 ) ) ;
#27821 = CARTESIAN_POINT ( 'NONE',  ( -20.47846945139902175, 44.37538166759063785, -20.53372385742072481 ) ) ;
#27822 = VECTOR ( 'NONE', #32306, 1000.000000000000114 ) ;
#27823 = CARTESIAN_POINT ( 'NONE',  ( 7.468012846824281681, 38.63503499907601224, -28.02196122052058058 ) ) ;
#27824 = CARTESIAN_POINT ( 'NONE',  ( 6.277390505771533514E-15, 61.00000000546237544, 34.17252228774368916 ) ) ;
#27825 = CARTESIAN_POINT ( 'NONE',  ( 11.25946833292375793, 71.67500000273119554, 8.180482586598731842 ) ) ;
#27826 = CARTESIAN_POINT ( 'NONE',  ( -19.09188309203694445, 11.99999999999999645, -19.09188309203661049 ) ) ;
#27827 = CARTESIAN_POINT ( 'NONE',  ( -1.778240108872766143E-15, 53.50000000000000000, -32.49999999999999289 ) ) ;
#27828 = CARTESIAN_POINT ( 'NONE',  ( -26.29305231718579350, 78.30000000546239391, -19.10302069950537884 ) ) ;
#27829 = CARTESIAN_POINT ( 'NONE',  ( 26.00068869287340334, 13.00260416666666430, -15.01150461594642316 ) ) ;
#27830 = CARTESIAN_POINT ( 'NONE',  ( -27.16883889988623935, 43.57500000273119412, 19.73931689729374739 ) ) ;
#27831 = CARTESIAN_POINT ( 'NONE',  ( -32.50000000000000000, 76.00000000000001421, 0.000000000000000000 ) ) ;
#27832 = ORIENTED_EDGE ( 'NONE', *, *, #26431, .T. ) ;
#27833 = CARTESIAN_POINT ( 'NONE',  ( 33.58253175000000113, 72.37500000273116996, -4.112674001490185761E-15 ) ) ;
#27834 = CARTESIAN_POINT ( 'NONE',  ( -10.04305231718578462, 28.90000000546237402, 30.90933677959249337 ) ) ;
#27835 = ORIENTED_EDGE ( 'NONE', *, *, #28647, .T. ) ;
#27836 = CARTESIAN_POINT ( 'NONE',  ( 28.01184896238290278, 37.20833333333332860, -7.505752307973347470 ) ) ;
#27837 = CARTESIAN_POINT ( 'NONE',  ( 10.04305231718578817, 59.90000000546235981, -30.90933677959249337 ) ) ;
#27838 = ORIENTED_EDGE ( 'NONE', *, *, #29363, .F. ) ;
#27839 = CARTESIAN_POINT ( 'NONE',  ( -26.29305231718579350, 55.80000000000001847, -19.10302069950537884 ) ) ;
#27840 = CARTESIAN_POINT ( 'NONE',  ( -10.37757302488624411, 46.72500000273119269, -31.93888565452638417 ) ) ;
#27841 = CARTESIAN_POINT ( 'NONE',  ( 26.29305231718579350, 55.30000000546236549, 19.10302069950537529 ) ) ;
#27842 = CARTESIAN_POINT ( 'NONE',  ( 8.327598234202002696E-15, -91.00000000000000000, 0.000000000000000000 ) ) ;
#27843 = APPLICATION_CONTEXT ( 'automotive_design' ) ;
#27844 = CARTESIAN_POINT ( 'NONE',  ( 20.08610463437157279, 3.800000005462383257, -27.64615127144129758 ) ) ;
#27845 = CARTESIAN_POINT ( 'NONE',  ( -33.58253175000000113, 65.02500000273118985, -10.91162601494193041 ) ) ;
#27846 = CARTESIAN_POINT ( 'NONE',  ( -26.00068869287368756, 15.29427083333332860, -15.01150461594595775 ) ) ;
#27847 = AXIS2_PLACEMENT_3D ( 'NONE', #17827, #12843, #10609 ) ;
#27848 = CARTESIAN_POINT ( 'NONE',  ( -26.29305231718578995, 52.19999999999999574, 19.10302069950538595 ) ) ;
#27849 = CARTESIAN_POINT ( 'NONE',  ( -8.891200544363830713E-16, 79.49999999999998579, -15.00000000000000000 ) ) ;
#27850 = CARTESIAN_POINT ( 'NONE',  ( -20.75514604977248823, 17.07500000273119056, -28.56700777964554305 ) ) ;
#27851 = FACE_OUTER_BOUND ( 'NONE', #30, .T. ) ;
#27852 = CARTESIAN_POINT ( 'NONE',  ( 13.94119854578893580, 28.46576416574268720, -24.22776226481265383 ) ) ;
#27853 = CARTESIAN_POINT ( 'NONE',  ( -4.300734207923755825, 73.27500000273118985, 13.23629886949340673 ) ) ;
#27854 = CARTESIAN_POINT ( 'NONE',  ( -1.778240108872766143E-15, 55.49999999999999289, -32.49999999999999289 ) ) ;
#27855 = CARTESIAN_POINT ( 'NONE',  ( -40.00000000000000711, 52.00000000000000711, 23.09401076758504345 ) ) ;
#27856 = CARTESIAN_POINT ( 'NONE',  ( 33.58253175000000823, 78.27500000273116143, 10.91162601494192863 ) ) ;
#27857 = VERTEX_POINT ( 'NONE', #6895 ) ;
#27858 = CARTESIAN_POINT ( 'NONE',  ( 14.47279130897151589, 4.824999997268814234, 19.92008829642072953 ) ) ;
#27859 = CARTESIAN_POINT ( 'NONE',  ( 0.000000000000000000, 74.00000000000001421, 15.00000000000000000 ) ) ;
#27860 = CARTESIAN_POINT ( 'NONE',  ( -13.97622843553632421, 46.51822916666666430, -24.20753774853731599 ) ) ;
#27861 = CARTESIAN_POINT ( 'NONE',  ( -20.75514604977248112, 59.42500000273118843, 28.56700777964554661 ) ) ;
#27862 = CARTESIAN_POINT ( 'NONE',  ( -33.58253175000000113, 21.47500000273119980, 10.91162601494193929 ) ) ;
#27863 = CARTESIAN_POINT ( 'NONE',  ( -33.58253175000000113, 13.37500000273118772, 0.000000000000000000 ) ) ;
#27864 = CARTESIAN_POINT ( 'NONE',  ( -20.08610463437156923, 20.29999999999999716, 27.64615127144130113 ) ) ;
#27865 = CARTESIAN_POINT ( 'NONE',  ( -20.47846945139902175, 16.87538166759064140, -20.53372385742072481 ) ) ;
#27866 = CARTESIAN_POINT ( 'NONE',  ( 28.01184896238290278, 61.27083333333332860, -7.505752307973347470 ) ) ;
#27867 = CARTESIAN_POINT ( 'NONE',  ( -33.58253175000000113, 1.125000002731191273, 0.000000000000000000 ) ) ;
#27868 = CARTESIAN_POINT ( 'NONE',  ( 0.000000000000000000, 80.00000000000001421, -32.50000000000000000 ) ) ;
#27869 = CARTESIAN_POINT ( 'NONE',  ( 26.29305231718578995, 41.20000000000000284, -19.10302069950538240 ) ) ;
#27870 = CARTESIAN_POINT ( 'NONE',  ( -33.58253175000000113, 51.02500000273119696, -10.91162601494193041 ) ) ;
#27871 = CARTESIAN_POINT ( 'NONE',  ( 23.41746825000000243, 19.02499999726880375, 7.608796670333735079 ) ) ;
#27872 = CARTESIAN_POINT ( 'NONE',  ( 32.50000000000000711, 21.40000000546237757, 10.55989012756945122 ) ) ;
#27873 = ORIENTED_EDGE ( 'NONE', *, *, #12800, .F. ) ;
#27874 = CARTESIAN_POINT ( 'NONE',  ( -33.58253175000000113, 59.47500000273118559, 10.91162601494193929 ) ) ;
#27875 = CARTESIAN_POINT ( 'NONE',  ( 5.779280353836490358E-15, 4.500000000000003553, 32.49999999999999289 ) ) ;
#27876 = CARTESIAN_POINT ( 'NONE',  ( -23.41746824999999887, 11.62499999726881938, -2.867812753649727150E-15 ) ) ;
#27877 = CARTESIAN_POINT ( 'NONE',  ( -0.04044903254992426173, 29.33631916759064850, 27.95245687107223276 ) ) ;
#27878 = VERTEX_POINT ( 'NONE', #25086 ) ;
#27879 = CARTESIAN_POINT ( 'NONE',  ( 33.58253175000000113, 30.12500000273120193, -4.112674001490185761E-15 ) ) ;
#27880 = CARTESIAN_POINT ( 'NONE',  ( 5.779280353836490358E-15, 56.49999999999998579, 32.49999999999999289 ) ) ;
#27881 = ORIENTED_EDGE ( 'NONE', *, *, #29583, .T. ) ;
#27882 = CARTESIAN_POINT ( 'NONE',  ( -28.01184896238290278, 59.55208333333332149, 7.505752307973363457 ) ) ;
#27883 = CYLINDRICAL_SURFACE ( 'NONE', #15507, 32.50000000000000000 ) ;
#27884 = CARTESIAN_POINT ( 'NONE',  ( -20.75514604977248112, 69.42500000273116711, 28.56700777964554661 ) ) ;
#27885 = CARTESIAN_POINT ( 'NONE',  ( 28.01184896238304134, 40.93229166666666430, 7.505752307972846538 ) ) ;
#27886 = CARTESIAN_POINT ( 'NONE',  ( 24.50000000000000355, 10.10000000000000142, -7.960532557706203605 ) ) ;
#27887 = CARTESIAN_POINT ( 'NONE',  ( -10.37757302488623701, 3.775000002731176973, 31.93888565452638417 ) ) ;
#27888 = CARTESIAN_POINT ( 'NONE',  ( 6.486482029760649416E-15, 9.625000002731196602, 35.31076352940723240 ) ) ;
#27889 = CARTESIAN_POINT ( 'NONE',  ( 2.521031746877078694E-15, -43.58578643762690064, 0.000000000000000000 ) ) ;
#27890 = CARTESIAN_POINT ( 'NONE',  ( -7.468012846824272799, 50.66628499907601935, 28.02196122052058413 ) ) ;
#27891 = CARTESIAN_POINT ( 'NONE',  ( 9.270509831248423538, 77.30000000000001137, -12.75976212528059861 ) ) ;
#27892 = CARTESIAN_POINT ( 'NONE',  ( -26.00068869287368756, 59.98177083333332860, -15.01150461594595775 ) ) ;
#27893 = CARTESIAN_POINT ( 'NONE',  ( 20.08610463437157279, 55.29999999999999716, -27.64615127144129758 ) ) ;
#27894 = CARTESIAN_POINT ( 'NONE',  ( -10.04305231718578462, 52.39999999999999147, 30.90933677959249337 ) ) ;
#27895 = CARTESIAN_POINT ( 'NONE',  ( -19.82091636218621389, 6.949999994537630954, 14.40073868116558842 ) ) ;
#27896 = CARTESIAN_POINT ( 'NONE',  ( 15.00000000000000000, 75.25000000546239676, -1.836970198721029589E-15 ) ) ;
#27897 = CARTESIAN_POINT ( 'NONE',  ( -13.97622843553632421, 25.89322916666666430, -24.20753774853731599 ) ) ;
#27898 = EDGE_CURVE ( 'NONE', #7938, #7704, #15513, .T. ) ;
#27899 = CARTESIAN_POINT ( 'NONE',  ( -33.58253175000000113, 35.02500000273118275, -10.91162601494193218 ) ) ;
#27900 = CARTESIAN_POINT ( 'NONE',  ( -20.75514604977248823, 78.82500000273120122, -28.56700777964554305 ) ) ;
#27901 = CARTESIAN_POINT ( 'NONE',  ( 6.486482029760649416E-15, 39.87500000273119127, 35.31076352940723240 ) ) ;
#27902 = CARTESIAN_POINT ( 'NONE',  ( -27.16883889988624290, 19.17500000273120264, -19.73931689729374028 ) ) ;
#27903 = CARTESIAN_POINT ( 'NONE',  ( -24.50000000000000711, 16.84999999453763309, 7.960532557706201828 ) ) ;
#27904 = EDGE_CURVE ( 'NONE', #3815, #25643, #11093, .T. ) ;
#27905 = CARTESIAN_POINT ( 'NONE',  ( -24.50000000000000711, 14.84999999453763841, 7.960532557706201828 ) ) ;
#27906 = CARTESIAN_POINT ( 'NONE',  ( 10.04305231718578817, 79.39999999999999147, -30.90933677959249337 ) ) ;
#27907 = CARTESIAN_POINT ( 'NONE',  ( -32.50000000000000000, 63.99999999999998579, 0.000000000000000000 ) ) ;
#27908 = CARTESIAN_POINT ( 'NONE',  ( -23.41746824999999887, 11.62499999726881938, -2.867812753649727150E-15 ) ) ;
#27909 = CARTESIAN_POINT ( 'NONE',  ( -0.04044903255044120238, 28.17930583240935860, -30.02300923189239867 ) ) ;
#27910 = CARTESIAN_POINT ( 'NONE',  ( -15.00000000000000000, 78.09999999999998010, 4.873795443493597723 ) ) ;
#27911 = CARTESIAN_POINT ( 'NONE',  ( -19.06425588902558133, 40.64024333240936215, 19.11951029504797006 ) ) ;
#27912 = CARTESIAN_POINT ( 'NONE',  ( 10.37757302488624767, 77.97500000273120691, 31.93888565452638417 ) ) ;
#27913 = CARTESIAN_POINT ( 'NONE',  ( -27.16883889988624290, 14.92500000273117067, -19.73931689729374028 ) ) ;
#27914 = CARTESIAN_POINT ( 'NONE',  ( 14.47279130897151767, 9.424999997268814766, -19.92008829642072598 ) ) ;
#27915 = CARTESIAN_POINT ( 'NONE',  ( 13.97622843553589966, 64.27864583333332860, -24.20753774853756113 ) ) ;
#27916 = ORIENTED_EDGE ( 'NONE', *, *, #21266, .T. ) ;
#27917 = CARTESIAN_POINT ( 'NONE',  ( 27.16883889988624290, 51.92500000273118843, 19.73931689729373673 ) ) ;
#27918 = CARTESIAN_POINT ( 'NONE',  ( 33.58253175000000113, 22.47500000273119625, -10.91162601494193751 ) ) ;
#27919 = EDGE_LOOP ( 'NONE', ( #24207, #30759, #5199, #94 ) ) ;
#27920 = CARTESIAN_POINT ( 'NONE',  ( -20.50609665441004736, 32.62500000000000000, -20.50609665440969565 ) ) ;
#27921 = CARTESIAN_POINT ( 'NONE',  ( -7.543491769121417612, 32.91704833425729504, 28.00173670424549499 ) ) ;
#27922 = LINE ( 'NONE', #17804, #4672 ) ;
#27923 = CARTESIAN_POINT ( 'NONE',  ( -23.41746825000000243, 4.024999997268810858, -7.608796670333730638 ) ) ;
#27924 = CARTESIAN_POINT ( 'NONE',  ( -14.47279130897152122, 11.92499999726882010, 19.92008829642072243 ) ) ;
#27925 = CARTESIAN_POINT ( 'NONE',  ( -33.58253175000000113, 23.47500000273119269, 10.91162601494193929 ) ) ;
#27926 = CARTESIAN_POINT ( 'NONE',  ( 32.50000000000000000, 21.60000000546237331, -10.55989012756945833 ) ) ;
#27927 = CARTESIAN_POINT ( 'NONE',  ( 10.04305231718579705, 68.59999999999999432, 30.90933677959248982 ) ) ;
#27928 = CARTESIAN_POINT ( 'NONE',  ( -20.08610463437157989, 6.200000005462364960, -27.64615127144129758 ) ) ;
#27929 = CARTESIAN_POINT ( 'NONE',  ( 32.50000000000000000, 66.99999999999998579, -3.980102097228898626E-15 ) ) ;
#27930 = CARTESIAN_POINT ( 'NONE',  ( 15.04653450569292872, 62.27902750092396644, -25.98046417659857710 ) ) ;
#27931 = CARTESIAN_POINT ( 'NONE',  ( 27.16883889988623935, 34.57500000273120122, -19.73931689729374384 ) ) ;
#27932 = CARTESIAN_POINT ( 'NONE',  ( 4.300734207923761154, 79.97500000273119269, 13.23629886949340495 ) ) ;
#27933 = CARTESIAN_POINT ( 'NONE',  ( 26.00068869287341045, 30.19010416666665719, -15.01150461594642493 ) ) ;
#27934 = APPLICATION_PROTOCOL_DEFINITION ( 'draft international standard', 'automotive_design', 1998, #12045 ) ;
#27935 = CARTESIAN_POINT ( 'NONE',  ( -18.94512977948575738, 15.92499999726881832, -13.76444248337723231 ) ) ;
#27936 = CARTESIAN_POINT ( 'NONE',  ( 6.277390505771533514E-15, 14.50000000000000888, 34.17252228774368916 ) ) ;
#27937 = CARTESIAN_POINT ( 'NONE',  ( 19.82091636218621034, 15.80000000000000782, 14.40073868116559730 ) ) ;
#27938 = ADVANCED_FACE ( 'NONE', ( #2438 ), #15832, .T. ) ;
#27939 = CARTESIAN_POINT ( 'NONE',  ( 24.22776226481265383, 46.51263916574269786, 13.94119854578893580 ) ) ;
#27940 = CARTESIAN_POINT ( 'NONE',  ( -27.16883889988624290, 58.92500000273118133, -19.73931689729374028 ) ) ;
#27941 = CARTESIAN_POINT ( 'NONE',  ( 33.58253175000000823, 64.27500000273118985, 10.91162601494192863 ) ) ;
#27942 = CARTESIAN_POINT ( 'NONE',  ( 27.16883889988623935, 50.57500000273118701, -19.73931689729374384 ) ) ;
#27943 = CARTESIAN_POINT ( 'NONE',  ( 23.41746824999999887, 14.52499999726882685, 7.608796670333735079 ) ) ;
#27944 = LINE ( 'NONE', #32734, #31988 ) ;
#27945 = CARTESIAN_POINT ( 'NONE',  ( -32.50000000000000000, 5.899999999999987921, -10.55989012756945300 ) ) ;
#27946 = CARTESIAN_POINT ( 'NONE',  ( -14.01125832528285109, 50.24777750092398065, 24.18731323226248264 ) ) ;
#27947 = CARTESIAN_POINT ( 'NONE',  ( 21.93819159779297223, 16.99999999999998934, 8.226848600189008209 ) ) ;
#27948 = CARTESIAN_POINT ( 'NONE',  ( 24.50000000000000000, 3.899999999999992806, 7.960532557706212486 ) ) ;
#27949 = CARTESIAN_POINT ( 'NONE',  ( 27.16883889988623935, 20.32500000273117280, -19.73931689729374384 ) ) ;
#27950 = DIRECTION ( 'NONE',  ( -0.000000000000000000, -1.000000000000000000, -0.000000000000000000 ) ) ;
#27951 = LINE ( 'NONE', #12331, #21576 ) ;
#27952 = LINE ( 'NONE', #9929, #4503 ) ;
#27953 = CARTESIAN_POINT ( 'NONE',  ( 7.468012846824281681, 62.69753499907601224, -28.02196122052058058 ) ) ;
#27954 = CARTESIAN_POINT ( 'NONE',  ( 20.08610463437158344, 41.20000000546236407, 27.64615127144129403 ) ) ;
#27955 = CARTESIAN_POINT ( 'NONE',  ( 10.04305231718579705, 34.59999999999999432, 30.90933677959248982 ) ) ;
#27956 = CARTESIAN_POINT ( 'NONE',  ( 6.486482029760648627E-15, 33.62500000273119127, 35.31076352940722529 ) ) ;
#27957 = CARTESIAN_POINT ( 'NONE',  ( -13.97622843553632421, 39.64322916666667140, -24.20753774853731599 ) ) ;
#27958 = VERTEX_POINT ( 'NONE', #15318 ) ;
#27959 = CARTESIAN_POINT ( 'NONE',  ( 33.58253175000000113, 70.12500000273118417, -4.112674001490185761E-15 ) ) ;
#27960 = CARTESIAN_POINT ( 'NONE',  ( -28.01184896238290278, 38.92708333333333570, 7.505752307973363457 ) ) ;
#27961 = DIRECTION ( 'NONE',  ( 1.224646799147353454E-16, -1.000000000000000000, 0.000000000000000000 ) ) ;
#27962 = VERTEX_POINT ( 'NONE', #33319 ) ;
#27963 = CARTESIAN_POINT ( 'NONE',  ( 7.468012846824777284, 60.13059000092398065, 28.02196122052045268 ) ) ;
#27964 = CARTESIAN_POINT ( 'NONE',  ( 27.95245687107223986, 59.41444416759064495, 0.04044903254993640479 ) ) ;
#27965 = CARTESIAN_POINT ( 'NONE',  ( 27.16883889988623935, 14.32500000273119412, -19.73931689729374384 ) ) ;
#27966 = CARTESIAN_POINT ( 'NONE',  ( 28.02196122052058413, 18.86940999907601935, 7.468012846824272799 ) ) ;
#27967 = DIRECTION ( 'NONE',  ( -0.000000000000000000, -1.000000000000000000, -0.000000000000000000 ) ) ;
#27968 = CARTESIAN_POINT ( 'NONE',  ( 33.58253175000000113, 38.47500000273118559, -10.91162601494193751 ) ) ;
#27969 = CARTESIAN_POINT ( 'NONE',  ( 32.50000000000000711, 43.40000000546238113, 10.55989012756945122 ) ) ;
#27970 = CARTESIAN_POINT ( 'NONE',  ( -12.13525491562421088, 73.80000000000002558, -8.816778784387096835 ) ) ;
#27971 = CARTESIAN_POINT ( 'NONE',  ( 20.75514604977248467, 32.42500000273116711, -28.56700777964554305 ) ) ;
#27972 = CARTESIAN_POINT ( 'NONE',  ( -32.50000000000000000, 24.09999999999999787, 10.55989012756946366 ) ) ;
#27973 = CARTESIAN_POINT ( 'NONE',  ( -10.37757302488624411, 56.97500000273119980, -31.93888565452638417 ) ) ;
#27974 = CARTESIAN_POINT ( 'NONE',  ( 10.04305231718578817, 27.39999999999999503, -30.90933677959249337 ) ) ;
#27975 = CARTESIAN_POINT ( 'NONE',  ( 26.29305231718579350, 36.79999999999999716, 19.10302069950537529 ) ) ;
#27976 = CARTESIAN_POINT ( 'NONE',  ( 7.236395654485755280, 18.22499999726881370, 22.27133577429736988 ) ) ;
#27977 = CARTESIAN_POINT ( 'NONE',  ( -10.37757302488624411, 74.72500000273119269, -31.93888565452638417 ) ) ;
#27978 = CARTESIAN_POINT ( 'NONE',  ( -17.97732221215932569, 66.99999999999998579, 27.49025280458516463 ) ) ;
#27979 = CARTESIAN_POINT ( 'NONE',  ( 13.91746824999999887, 74.37500000273116996, -1.704398294459741270E-15 ) ) ;
#27980 = CARTESIAN_POINT ( 'NONE',  ( -2.162160676586882350E-15, 68.87500000273118417, -35.31076352940722529 ) ) ;
#27981 = CARTESIAN_POINT ( 'NONE',  ( 9.270509831248425314, 78.95000000546235697, 12.75976212528059683 ) ) ;
#27982 = ORIENTED_EDGE ( 'NONE', *, *, #480, .T. ) ;
#27983 = CARTESIAN_POINT ( 'NONE',  ( 10.37757302488624056, 18.52500000273118985, -31.93888565452638417 ) ) ;
#27984 = CARTESIAN_POINT ( 'NONE',  ( -4.732186688966233175E-15, 11.24999999453763699, 25.76082449383753925 ) ) ;
#27985 = CARTESIAN_POINT ( 'NONE',  ( 24.18731323226247554, 21.88840250092397710, 14.01125832528285997 ) ) ;
#27986 = CARTESIAN_POINT ( 'NONE',  ( -20.08610463437157989, 25.69999999999999929, -27.64615127144129758 ) ) ;
#27987 = CARTESIAN_POINT ( 'NONE',  ( -10.37757302488623701, 39.52500000273119696, 31.93888565452638417 ) ) ;
#27988 = CARTESIAN_POINT ( 'NONE',  ( -27.16883889988624290, 7.175000002731176885, -19.73931689729374028 ) ) ;
#27989 = CARTESIAN_POINT ( 'NONE',  ( -2.162160676586882350E-15, 56.87500000273117706, -35.31076352940722529 ) ) ;
#27990 = CARTESIAN_POINT ( 'NONE',  ( 26.02091320914851025, 45.37798583425732346, -14.97647472619946463 ) ) ;
#27991 = CARTESIAN_POINT ( 'NONE',  ( 15.14183272437242422, 6.300000000000004263, -20.84094480462497856 ) ) ;
#27992 = CARTESIAN_POINT ( 'NONE',  ( 28.02196122052058413, 36.05690999907600514, 7.468012846824272799 ) ) ;
#27993 = CARTESIAN_POINT ( 'NONE',  ( 26.29305231718578995, 63.70000000546237118, -19.10302069950538240 ) ) ;
#27994 = CARTESIAN_POINT ( 'NONE',  ( 8.601468415847520532, 73.57500000273117280, 11.83890561707634781 ) ) ;
#27995 = CARTESIAN_POINT ( 'NONE',  ( -24.18731323226221974, 68.28347249907602645, 14.01125832528330406 ) ) ;
#27996 = LINE ( 'NONE', #9630, #26918 ) ;
#27997 = CARTESIAN_POINT ( 'NONE',  ( 32.50000000000000711, 75.40000000546240244, 10.55989012756945122 ) ) ;
#27998 = CARTESIAN_POINT ( 'NONE',  ( -26.00068869287368756, 15.29427083333332504, -15.01150461594595775 ) ) ;
#27999 = CARTESIAN_POINT ( 'NONE',  ( -27.16883889988624290, 33.17500000273120264, -19.73931689729374028 ) ) ;
#28000 = CARTESIAN_POINT ( 'NONE',  ( 23.41746824999999887, 7.124999997268815832, 0.000000000000000000 ) ) ;
#28001 = VERTEX_POINT ( 'NONE', #15666 ) ;
#28002 = CARTESIAN_POINT ( 'NONE',  ( -27.16883889988623935, 75.57500000273120122, 19.73931689729374739 ) ) ;
#28003 = CARTESIAN_POINT ( 'NONE',  ( -10.04305231718578462, 24.90000000546237047, 30.90933677959249337 ) ) ;
#28004 = VERTEX_POINT ( 'NONE', #15146 ) ;
#28005 = CARTESIAN_POINT ( 'NONE',  ( 28.01184896238290278, 47.52083333333332860, -7.505752307973347470 ) ) ;
#28006 = CARTESIAN_POINT ( 'NONE',  ( -10.04305231718578462, 62.90000000546236691, 30.90933677959249337 ) ) ;
#28007 = ORIENTED_EDGE ( 'NONE', *, *, #11255, .F. ) ;
#28008 = CIRCLE ( 'NONE', #1136, 12.11000150615021909 ) ;
#28009 = CARTESIAN_POINT ( 'NONE',  ( -33.58253175000000113, 49.02500000273116854, -10.91162601494193218 ) ) ;
#28010 = CARTESIAN_POINT ( 'NONE',  ( -23.41746825000000243, 15.52499999726882507, -7.608796670333730638 ) ) ;
#28011 = CARTESIAN_POINT ( 'NONE',  ( -10.04305231718579172, 8.100000005462376862, -30.90933677959248982 ) ) ;
#28012 = CARTESIAN_POINT ( 'NONE',  ( -7.236395654485763274, 18.52499999726881086, 22.27133577429736633 ) ) ;
#28013 = CARTESIAN_POINT ( 'NONE',  ( -20.08610463437157989, 53.69999999999999574, -27.64615127144129758 ) ) ;
#28014 = CARTESIAN_POINT ( 'NONE',  ( 0.000000000000000000, 82.00000000000001421, 0.000000000000000000 ) ) ;
#28015 = CARTESIAN_POINT ( 'NONE',  ( -33.58253175000000113, 15.47500000273118381, 10.91162601494193929 ) ) ;
#28016 = FACE_OUTER_BOUND ( 'NONE', #3817, .T. ) ;
#28017 = CARTESIAN_POINT ( 'NONE',  ( 24.22776226481265383, 29.32513916574269075, 13.94119854578893580 ) ) ;
#28018 = CARTESIAN_POINT ( 'NONE',  ( 4.300734207923761154, 75.97500000273119269, 13.23629886949340495 ) ) ;
#28019 = CARTESIAN_POINT ( 'NONE',  ( 15.14183272437242067, 7.699999999999988631, 20.84094480462498211 ) ) ;
#28020 = CARTESIAN_POINT ( 'NONE',  ( -26.29305231718578995, 44.20000000000001705, 19.10302069950538595 ) ) ;
#28021 = CARTESIAN_POINT ( 'NONE',  ( -10.04305231718579172, 5.599999999999994316, -30.90933677959248982 ) ) ;
#28022 = ORIENTED_EDGE ( 'NONE', *, *, #1847, .T. ) ;
#28023 = CARTESIAN_POINT ( 'NONE',  ( -14.47279130897152122, 16.42499999726882365, 19.92008829642072243 ) ) ;
#28024 = CARTESIAN_POINT ( 'NONE',  ( 5.147494310547408247, 71.05125428700921475, 32.50000000000000711 ) ) ;
#28025 = AXIS2_PLACEMENT_3D ( 'NONE', #10340, #2949, #13421 ) ;
#28026 = CARTESIAN_POINT ( 'NONE',  ( 13.97622843553633665, 55.11197916666664298, 24.20753774853730889 ) ) ;
#28027 = CARTESIAN_POINT ( 'NONE',  ( 10.37757302488624767, 57.72500000273118559, 31.93888565452638417 ) ) ;
#28028 = CARTESIAN_POINT ( 'NONE',  ( 27.16883889988623935, 22.57500000273120122, -19.73931689729374384 ) ) ;
#28029 = CARTESIAN_POINT ( 'NONE',  ( -10.37757302488623701, 9.775000002731168536, 31.93888565452638417 ) ) ;
#28030 = CARTESIAN_POINT ( 'NONE',  ( 0.000000000000000000, 16.99999999999998579, -24.50000000000000000 ) ) ;
#28031 = CARTESIAN_POINT ( 'NONE',  ( -26.02091320914849959, 23.03423583425731280, 14.97647472619947528 ) ) ;
#28032 = EDGE_CURVE ( 'NONE', #16083, #22660, #28420, .T. ) ;
#28033 = CARTESIAN_POINT ( 'NONE',  ( -28.01184896238290278, 62.98958333333332149, 7.505752307973363457 ) ) ;
#28034 = CARTESIAN_POINT ( 'NONE',  ( 10.37757302488624767, 5.725000002731183812, 31.93888565452638417 ) ) ;
#28035 = CARTESIAN_POINT ( 'NONE',  ( 32.50000000000000000, 3.000000000000002665, -3.980102097228898626E-15 ) ) ;
#28036 = CARTESIAN_POINT ( 'NONE',  ( 20.08610463437157279, 43.30000000000000426, -27.64615127144129758 ) ) ;
#28037 = AXIS2_PLACEMENT_3D ( 'NONE', #27842, #143, #28476 ) ;
#28038 = CARTESIAN_POINT ( 'NONE',  ( -2.162160676586882350E-15, 42.62500000273119838, -35.31076352940722529 ) ) ;
#28039 = CARTESIAN_POINT ( 'NONE',  ( -18.94512977948575738, 3.424999997268807217, -13.76444248337723231 ) ) ;
#28040 = ADVANCED_FACE ( 'NONE', ( #2262 ), #17136, .F. ) ;
#28041 = CARTESIAN_POINT ( 'NONE',  ( 15.00000000000000355, 78.89999999999997726, 4.873795443493592394 ) ) ;
#28042 = VERTEX_POINT ( 'NONE', #5183 ) ;
#28043 = CARTESIAN_POINT ( 'NONE',  ( 20.75514604977249178, 60.07500000273119412, 28.56700777964553950 ) ) ;
#28044 = CARTESIAN_POINT ( 'NONE',  ( 26.29305231718579350, 59.30000000546238681, 19.10302069950537529 ) ) ;
#28045 = CARTESIAN_POINT ( 'NONE',  ( -23.41746824999999887, 13.62499999726882116, -2.867812753649727150E-15 ) ) ;
#28046 = CARTESIAN_POINT ( 'NONE',  ( -24.18731323226248264, 37.35715250092397355, -14.01125832528284931 ) ) ;
#28047 = ORIENTED_EDGE ( 'NONE', *, *, #32489, .F. ) ;
#28048 = CARTESIAN_POINT ( 'NONE',  ( 33.58253175000000113, 30.22500000273118559, -10.91162601494193751 ) ) ;
#28049 = CARTESIAN_POINT ( 'NONE',  ( -1.778240108872766143E-15, 34.00000000546236834, -32.49999999999999289 ) ) ;
#28050 = EDGE_LOOP ( 'NONE', ( #12117, #8668 ) ) ;
#28051 = CARTESIAN_POINT ( 'NONE',  ( -1.778240108872766143E-15, 19.50000000000000000, -32.49999999999999289 ) ) ;
#28052 = CARTESIAN_POINT ( 'NONE',  ( 10.37757302488624056, 66.52500000273120406, -31.93888565452638417 ) ) ;
#28053 = CARTESIAN_POINT ( 'NONE',  ( 7.505752307972854531, 43.51041666666666430, -28.01184896238303423 ) ) ;
#28054 = CARTESIAN_POINT ( 'NONE',  ( 19.82091636218621034, 9.800000000000002487, 14.40073868116559730 ) ) ;
#28055 = CARTESIAN_POINT ( 'NONE',  ( 18.94512977948576093, 1.324999997268816454, -13.76444248337722875 ) ) ;
#28056 = CARTESIAN_POINT ( 'NONE',  ( -27.16883889988623935, 7.325000002731174575, 19.73931689729374739 ) ) ;
#28057 = CARTESIAN_POINT ( 'NONE',  ( -3.880418787951124493, 7.198745712990782586, 24.50000000000000355 ) ) ;
#28058 = CARTESIAN_POINT ( 'NONE',  ( -30.02300923189239867, 51.38243083240936215, 0.04044903255044988294 ) ) ;
#28059 = CARTESIAN_POINT ( 'NONE',  ( 4.635254915624209993, 73.40000000000001990, -14.26584774442730463 ) ) ;
#28060 = CARTESIAN_POINT ( 'NONE',  ( -15.01150461594642316, 60.26822916666665719, -26.00068869287341045 ) ) ;
#28061 = CARTESIAN_POINT ( 'NONE',  ( 32.50000000000000000, 55.00000000000000711, -3.980102097228898626E-15 ) ) ;
#28062 = CARTESIAN_POINT ( 'NONE',  ( 5.147494310547434893, 22.55125428154684286, 32.49999999999999289 ) ) ;
#28063 = CARTESIAN_POINT ( 'NONE',  ( -24.50000000000000000, 10.74999999453762811, -3.000384657911015469E-15 ) ) ;
#28064 = DIRECTION ( 'NONE',  ( 0.000000000000000000, 0.000000000000000000, 1.000000000000000000 ) ) ;
#28065 = CARTESIAN_POINT ( 'NONE',  ( -27.95245687107222921, 21.88281249999999645, 2.498001805406602216E-13 ) ) ;
#28066 = CARTESIAN_POINT ( 'NONE',  ( -20.75514604977248112, 31.42500000273120619, 28.56700777964554661 ) ) ;
#28067 = CARTESIAN_POINT ( 'NONE',  ( 7.313012447739250820E-14, 11.49999999999999112, 24.50000000000000000 ) ) ;
#28068 = CARTESIAN_POINT ( 'NONE',  ( -20.75514604977248823, 45.07500000273117990, -28.56700777964554305 ) ) ;
#28069 = CARTESIAN_POINT ( 'NONE',  ( -20.75514604977248823, 23.07500000273117990, -28.56700777964554305 ) ) ;
#28070 = CARTESIAN_POINT ( 'NONE',  ( -32.50000000000000000, 12.60000000546236620, 10.55989012756946366 ) ) ;
#28071 = CARTESIAN_POINT ( 'NONE',  ( 0.000000000000000000, -20.99999999999998934, 0.000000000000000000 ) ) ;
#28072 = CARTESIAN_POINT ( 'NONE',  ( -8.891200544363830713E-16, 75.75000000546238255, -15.00000000000000000 ) ) ;
#28073 = CARTESIAN_POINT ( 'NONE',  ( 10.04305231718579705, 62.60000000000000142, 30.90933677959248982 ) ) ;
#28074 = CARTESIAN_POINT ( 'NONE',  ( 23.41746824999999887, 10.52499999726880731, 7.608796670333735079 ) ) ;
#28075 = CARTESIAN_POINT ( 'NONE',  ( -33.58253175000000113, 65.02500000273118985, -10.91162601494193041 ) ) ;
#28076 = CARTESIAN_POINT ( 'NONE',  ( -15.00000000000000000, 78.00000000000001421, 0.000000000000000000 ) ) ;
#28077 = CARTESIAN_POINT ( 'NONE',  ( -27.95245687107223986, 37.63243083240935505, 0.04044903255043252877 ) ) ;
#28078 = CARTESIAN_POINT ( 'NONE',  ( 33.58253175000000113, 78.47500000273116427, -10.91162601494193751 ) ) ;
#28079 = CARTESIAN_POINT ( 'NONE',  ( 20.75514604977249178, 11.82500000273118346, 28.56700777964553950 ) ) ;
#28080 = CARTESIAN_POINT ( 'NONE',  ( -7.236395654485763274, 12.52499999726880375, 22.27133577429736633 ) ) ;
#28081 = CARTESIAN_POINT ( 'NONE',  ( -2.428612866367529427E-13, 60.55468749999999289, -27.95245687107222921 ) ) ;
#28082 = ORIENTED_EDGE ( 'NONE', *, *, #6975, .F. ) ;
#28083 = CARTESIAN_POINT ( 'NONE',  ( -27.16883889988623935, 49.32500000273120122, 19.73931689729374739 ) ) ;
#28084 = CARTESIAN_POINT ( 'NONE',  ( 20.75514604977249178, 22.07500000273117990, 28.56700777964553950 ) ) ;
#28085 = EDGE_CURVE ( 'NONE', #23226, #7457, #4536, .T. ) ;
#28086 = ORIENTED_EDGE ( 'NONE', *, *, #33257, .T. ) ;
#28087 = CARTESIAN_POINT ( 'NONE',  ( -15.01150461594595775, 35.05989583333332860, 26.00068869287368756 ) ) ;
#28088 = CARTESIAN_POINT ( 'NONE',  ( 20.47846945139902530, 35.78163166759063074, 20.53372385742071771 ) ) ;
#28089 = CARTESIAN_POINT ( 'NONE',  ( 0.000000000000000000, 52.00000000000000711, 0.000000000000000000 ) ) ;
#28090 = DIRECTION ( 'NONE',  ( 1.000000000000000000, 0.000000000000000000, 1.224646799147352714E-16 ) ) ;
#28091 = CARTESIAN_POINT ( 'NONE',  ( -23.41746825000000598, 6.224999997268827023, 7.608796670333726198 ) ) ;
#28092 = CARTESIAN_POINT ( 'NONE',  ( -23.41746825000000243, 11.52499999726880553, -7.608796670333730638 ) ) ;
#28093 = CARTESIAN_POINT ( 'NONE',  ( -27.16883889988623935, 17.57500000273118346, 19.73931689729374739 ) ) ;
#28094 = CARTESIAN_POINT ( 'NONE',  ( -2.092463501923844636E-15, 26.00000000546237899, -34.17252228774368916 ) ) ;
#28095 = AXIS2_PLACEMENT_3D ( 'NONE', #19053, #21299, #29492 ) ;
#28096 = CARTESIAN_POINT ( 'NONE',  ( 20.08610463437157279, 67.30000000000001137, -27.64615127144129758 ) ) ;
#28097 = CARTESIAN_POINT ( 'NONE',  ( -19.82091636218621389, 5.200000000000009948, 14.40073868116558842 ) ) ;
#28098 = CARTESIAN_POINT ( 'NONE',  ( -7.239203213863182995, 74.00000000000001421, 12.48853769527896951 ) ) ;
#28099 = CARTESIAN_POINT ( 'NONE',  ( 25.98046417659858420, 63.13840250092397355, 15.04653450569292872 ) ) ;
#28100 = CARTESIAN_POINT ( 'NONE',  ( -10.37757302488623701, 27.77500000273119696, 31.93888565452638417 ) ) ;
#28101 = CARTESIAN_POINT ( 'NONE',  ( -8.601468415847515203, 79.67500000273118133, 11.83890561707634959 ) ) ;
#28102 = CARTESIAN_POINT ( 'NONE',  ( -26.00068869287368756, 29.04427083333332860, -15.01150461594595775 ) ) ;
#28103 = AXIS2_PLACEMENT_3D ( 'NONE', #18784, #26829, #8631 ) ;
#28104 = CARTESIAN_POINT ( 'NONE',  ( 18.94512977948575738, 14.92499999726881654, 13.76444248337723408 ) ) ;
#28105 = CARTESIAN_POINT ( 'NONE',  ( 10.04305231718578817, 7.400000000000018119, -30.90933677959249337 ) ) ;
#28106 = CARTESIAN_POINT ( 'NONE',  ( -20.08610463437157989, 51.69999999999999574, -27.64615127144129758 ) ) ;
#28107 = CARTESIAN_POINT ( 'NONE',  ( 24.18731323226221974, 52.81472249907603356, -14.01125832528328985 ) ) ;
#28108 = CARTESIAN_POINT ( 'NONE',  ( 27.16883889988624290, 55.92500000273120975, 19.73931689729373673 ) ) ;
#28109 = CARTESIAN_POINT ( 'NONE',  ( 6.486482029760649416E-15, 63.87500000273119127, 35.31076352940723240 ) ) ;
#28110 = CARTESIAN_POINT ( 'NONE',  ( -10.37757302488624411, 40.97500000273118559, -31.93888565452638417 ) ) ;
#28111 = CARTESIAN_POINT ( 'NONE',  ( -18.94512977948576093, 13.82499999726879913, 13.76444248337722698 ) ) ;
#28112 = CARTESIAN_POINT ( 'NONE',  ( 10.04305231718578817, 67.90000000546237402, -30.90933677959249337 ) ) ;
#28113 = CARTESIAN_POINT ( 'NONE',  ( -10.37757302488623701, 1.525000002731202731, 31.93888565452638417 ) ) ;
#28114 = CARTESIAN_POINT ( 'NONE',  ( -24.50000000000000000, 4.749999994537623671, -3.000384657911015469E-15 ) ) ;
#28115 = CARTESIAN_POINT ( 'NONE',  ( -32.50000000000000000, 78.00000000000000000, 0.000000000000000000 ) ) ;
#28116 = CARTESIAN_POINT ( 'NONE',  ( -27.16883889988624290, 20.92500000273118843, -19.73931689729374028 ) ) ;
#28117 = CARTESIAN_POINT ( 'NONE',  ( -8.960552108402744065E-16, 80.87500000273118417, -14.63369212191046209 ) ) ;
#28118 = CARTESIAN_POINT ( 'NONE',  ( 0.000000000000000000, -10.99999999999999645, 0.000000000000000000 ) ) ;
#28119 = DIRECTION ( 'NONE',  ( -0.000000000000000000, -1.000000000000000000, -0.000000000000000000 ) ) ;
#28120 = CARTESIAN_POINT ( 'NONE',  ( -28.02196122052058413, 65.27565999907601224, -7.468012846824272799 ) ) ;
#28121 = CARTESIAN_POINT ( 'NONE',  ( -2.092463501923844636E-15, 40.00000000546237544, -34.17252228774368916 ) ) ;
#28122 = CARTESIAN_POINT ( 'NONE',  ( 24.50000000000000000, 0.8749999972688105032, 0.000000000000000000 ) ) ;
#28123 = CARTESIAN_POINT ( 'NONE',  ( 20.75514604977249178, 33.82500000273118701, 28.56700777964553950 ) ) ;
#28124 = CARTESIAN_POINT ( 'NONE',  ( 2.584737979205441561E-13, 31.33593749999999289, 27.95245687107222921 ) ) ;
#28125 = EDGE_LOOP ( 'NONE', ( #33793, #21191, #3650, #6934 ) ) ;
#28126 = ORIENTED_EDGE ( 'NONE', *, *, #132, .T. ) ;
#28127 = CARTESIAN_POINT ( 'NONE',  ( -27.16883889988623935, 69.32500000273118701, 19.73931689729374739 ) ) ;
#28128 = CARTESIAN_POINT ( 'NONE',  ( 30.02300923189239512, 40.78906249999998579, -2.619432448724977703E-13 ) ) ;
#28129 = EDGE_CURVE ( 'NONE', #6559, #11786, #348, .T. ) ;
#28130 = CARTESIAN_POINT ( 'NONE',  ( -32.50000000000000000, 16.60000000546238752, 10.55989012756946366 ) ) ;
#28131 = ORIENTED_EDGE ( 'NONE', *, *, #31174, .F. ) ;
#28132 = CARTESIAN_POINT ( 'NONE',  ( -26.02091320914849959, 60.84673583425731636, 14.97647472619947528 ) ) ;
#28133 = CARTESIAN_POINT ( 'NONE',  ( -26.06988505166735237, 57.83892333425730214, -7.025853678916388567 ) ) ;
#28134 = CARTESIAN_POINT ( 'NONE',  ( 20.75514604977248467, 10.42500000273120087, -28.56700777964554305 ) ) ;
#28135 = EDGE_CURVE ( 'NONE', #33921, #19806, #8911, .T. ) ;
#28136 = CARTESIAN_POINT ( 'NONE',  ( -7.543491769121917656, 17.72357666574268720, -28.00173670424536354 ) ) ;
#28137 = CARTESIAN_POINT ( 'NONE',  ( 0.000000000000000000, 0.000000000000000000, 24.50000000000000000 ) ) ;
#28138 = CARTESIAN_POINT ( 'NONE',  ( 33.58253175000000823, 38.27500000273118985, 10.91162601494192863 ) ) ;
#28139 = CARTESIAN_POINT ( 'NONE',  ( 32.50000000000000000, 43.50000000546238965, -3.980102097228898626E-15 ) ) ;
#28140 = CARTESIAN_POINT ( 'NONE',  ( -15.00000000000000000, 78.00000000000001421, 0.000000000000000000 ) ) ;
#28141 = CARTESIAN_POINT ( 'NONE',  ( 20.75514604977249178, 25.82500000273117280, 28.56700777964553950 ) ) ;
#28142 = CARTESIAN_POINT ( 'NONE',  ( -13.91746824999999887, 80.87500000273118417, 0.000000000000000000 ) ) ;
#28143 = CARTESIAN_POINT ( 'NONE',  ( -27.16883889988623935, 53.57500000273118701, 19.73931689729374739 ) ) ;
#28144 = FILL_AREA_STYLE_COLOUR ( '', #21157 ) ;
#28145 = CARTESIAN_POINT ( 'NONE',  ( -26.29305231718579350, 29.80000000000000782, -19.10302069950537884 ) ) ;
#28146 = CARTESIAN_POINT ( 'NONE',  ( 32.50000000000000000, 29.10000000000000853, -10.55989012756945833 ) ) ;
#28147 = CARTESIAN_POINT ( 'NONE',  ( -14.47279130897152122, 17.92499999726880588, 19.92008829642072243 ) ) ;
#28148 = CARTESIAN_POINT ( 'NONE',  ( -27.16883889988624290, 78.92500000273116711, -19.73931689729374028 ) ) ;
#28149 = DIRECTION ( 'NONE',  ( 0.000000000000000000, -1.000000000000000000, 0.000000000000000000 ) ) ;
#28150 = CARTESIAN_POINT ( 'NONE',  ( -32.50000000000000000, 20.50000000546237189, 0.000000000000000000 ) ) ;
#28151 = CARTESIAN_POINT ( 'NONE',  ( 20.75514604977248467, 62.67500000273117422, -28.56700777964554305 ) ) ;
#28152 = CARTESIAN_POINT ( 'NONE',  ( -15.00000000000000000, 76.25000000546239676, 0.000000000000000000 ) ) ;
#28153 = EDGE_LOOP ( 'NONE', ( #3202, #31671, #1175, #26241 ) ) ;
#28154 = CARTESIAN_POINT ( 'NONE',  ( -20.75514604977248112, 17.42500000273117777, 28.56700777964554661 ) ) ;
#28155 = CARTESIAN_POINT ( 'NONE',  ( 19.82091636218621389, 9.949999994537634507, -14.40073868116559197 ) ) ;
#28156 = CARTESIAN_POINT ( 'NONE',  ( 7.025853678916403666, 20.88579833425730925, -26.06988505166735237 ) ) ;
#28157 = CARTESIAN_POINT ( 'NONE',  ( 15.14183272437242067, 7.449999994537640724, 20.84094480462498211 ) ) ;
#28158 = CARTESIAN_POINT ( 'NONE',  ( 33.58253175000000113, 38.12500000273118417, -4.112674001490185761E-15 ) ) ;
#28159 = CARTESIAN_POINT ( 'NONE',  ( 33.58253175000000113, 4.375000002731193938, -4.112674001490185761E-15 ) ) ;
#28160 = CARTESIAN_POINT ( 'NONE',  ( 33.58253175000000113, 54.47500000273117138, -10.91162601494193574 ) ) ;
#28161 = CARTESIAN_POINT ( 'NONE',  ( 25.98046417659858420, 49.38840250092398776, 15.04653450569292872 ) ) ;
#28162 = CARTESIAN_POINT ( 'NONE',  ( 1.555960095263670572E-15, 6.499999999999994671, -24.50000000000000000 ) ) ;
#28163 = CARTESIAN_POINT ( 'NONE',  ( 7.543491769121922985, 36.62982666574267654, 28.00173670424535644 ) ) ;
#28164 = CARTESIAN_POINT ( 'NONE',  ( 20.08610463437158344, 59.20000000546237828, 27.64615127144129403 ) ) ;
#28165 = CARTESIAN_POINT ( 'NONE',  ( 2.688165632520823219E-15, 73.37500000273118417, 14.63369212191046387 ) ) ;
#28166 = CARTESIAN_POINT ( 'NONE',  ( -7.570916362186215665, 3.149999994537633352, 23.30088464923126423 ) ) ;
#28167 = CARTESIAN_POINT ( 'NONE',  ( -24.18731323226221974, 64.84597249907602645, 14.01125832528330406 ) ) ;
#28168 = CARTESIAN_POINT ( 'NONE',  ( -20.08610463437156923, 72.80000000546239391, 27.64615127144130113 ) ) ;
#28169 = LINE ( 'NONE', #20284, #33857 ) ;
#28170 = CARTESIAN_POINT ( 'NONE',  ( 10.37757302488624056, 32.77500000273118985, -31.93888565452638417 ) ) ;
#28171 = CARTESIAN_POINT ( 'NONE',  ( 23.41746824999999887, 11.02499999726882152, 7.608796670333735079 ) ) ;
#28172 = ORIENTED_EDGE ( 'NONE', *, *, #24060, .F. ) ;
#28173 = CARTESIAN_POINT ( 'NONE',  ( 10.37757302488624056, 74.77500000273118985, -31.93888565452638417 ) ) ;
#28174 = AXIS2_PLACEMENT_3D ( 'NONE', #33981, #12707, #21122 ) ;
#28175 = CARTESIAN_POINT ( 'NONE',  ( 32.50000000000000711, 23.40000000546237047, 10.55989012756945122 ) ) ;
#28176 = CARTESIAN_POINT ( 'NONE',  ( 26.00068869287340334, 40.50260416666666430, -15.01150461594642316 ) ) ;
#28177 = CARTESIAN_POINT ( 'NONE',  ( -26.29305231718578995, 64.70000000546238539, 19.10302069950538595 ) ) ;
#28178 = ORIENTED_EDGE ( 'NONE', *, *, #33712, .T. ) ;
#28179 = CARTESIAN_POINT ( 'NONE',  ( 19.82091636218621034, 5.549999994537619052, 14.40073868116559730 ) ) ;
#28180 = CARTESIAN_POINT ( 'NONE',  ( 10.37757302488624767, 51.72500000273119980, 31.93888565452638417 ) ) ;
#28181 = CARTESIAN_POINT ( 'NONE',  ( 14.47279130897151589, 18.32499999726882578, 19.92008829642072953 ) ) ;
#28182 = CARTESIAN_POINT ( 'NONE',  ( 32.50000000000000711, 3.400000005462366914, 10.55989012756945122 ) ) ;
#28183 = CARTESIAN_POINT ( 'NONE',  ( 3.000384657911015469E-15, 0.000000000000000000, -24.50000000000000000 ) ) ;
#28184 = CARTESIAN_POINT ( 'NONE',  ( 28.01184896238290278, 16.58333333333333215, -7.505752307973347470 ) ) ;
#28185 = CARTESIAN_POINT ( 'NONE',  ( -2.092463501923844636E-15, 47.49999999999997868, -34.17252228774368916 ) ) ;
#28186 = CARTESIAN_POINT ( 'NONE',  ( -23.41746824999999887, 1.624999997268811169, -2.867812753649727150E-15 ) ) ;
#28187 = CARTESIAN_POINT ( 'NONE',  ( -33.58253175000000113, 19.37500000273118062, 0.000000000000000000 ) ) ;
#28188 = CARTESIAN_POINT ( 'NONE',  ( 15.14183272437242422, 0.2999999999999904965, -20.84094480462497856 ) ) ;
#28189 = CARTESIAN_POINT ( 'NONE',  ( 6.950374756619257965, 21.44753499907601579, -26.09010956794244507 ) ) ;
#28190 = CARTESIAN_POINT ( 'NONE',  ( 2.688165632520823219E-15, 75.87500000273119838, 14.63369212191046387 ) ) ;
#28191 = CARTESIAN_POINT ( 'NONE',  ( -10.69578794377713926, -43.58578643762690064, 0.000000000000000000 ) ) ;
#28192 = CARTESIAN_POINT ( 'NONE',  ( -1.778240108872766143E-15, 54.00000000546237544, -32.49999999999999289 ) ) ;
#28193 = CARTESIAN_POINT ( 'NONE',  ( -33.58253175000000113, 79.37500000273119838, 0.000000000000000000 ) ) ;
#28194 = ORIENTED_EDGE ( 'NONE', *, *, #16639, .T. ) ;
#28195 = CARTESIAN_POINT ( 'NONE',  ( 18.94512977948575738, 12.92499999726881654, 13.76444248337723408 ) ) ;
#28196 = CARTESIAN_POINT ( 'NONE',  ( -14.47279130897152299, 5.924999997268808549, 19.92008829642072243 ) ) ;
#28197 = STYLED_ITEM ( 'NONE', ( #7332 ), #18129 ) ;
#28198 = CARTESIAN_POINT ( 'NONE',  ( -24.20753774853730889, 49.09635416666665719, 13.97622843553633842 ) ) ;
#28199 = ADVANCED_FACE ( 'NONE', ( #7412 ), #30919, .F. ) ;
#28200 = CARTESIAN_POINT ( 'NONE',  ( -27.16883889988623935, 59.32500000273120833, 19.73931689729374739 ) ) ;
#28201 = CARTESIAN_POINT ( 'NONE',  ( 33.58253175000000113, 22.37500000273119483, -4.112674001490185761E-15 ) ) ;
#28202 = CARTESIAN_POINT ( 'NONE',  ( 33.58253175000000113, 8.475000002731185589, -10.91162601494193751 ) ) ;
#28203 = CARTESIAN_POINT ( 'NONE',  ( -13.97622843553632777, 29.33072916666665719, -24.20753774853731599 ) ) ;
#28204 = CARTESIAN_POINT ( 'NONE',  ( -0.04044903254990864921, 19.02381916759064495, 30.02300923189239867 ) ) ;
#28205 = CARTESIAN_POINT ( 'NONE',  ( -30.02300923189239512, 59.69531250000000711, 2.654126918244515359E-13 ) ) ;
#28206 = CARTESIAN_POINT ( 'NONE',  ( -33.58253175000000113, 3.025000002731184967, -10.91162601494193218 ) ) ;
#28207 = CARTESIAN_POINT ( 'NONE',  ( 20.08610463437158344, 68.70000000000001705, 27.64615127144129403 ) ) ;
#28208 = CARTESIAN_POINT ( 'NONE',  ( -10.04305231718578462, 44.40000000000000568, 30.90933677959249337 ) ) ;
#28209 = CARTESIAN_POINT ( 'NONE',  ( -10.37757302488623701, 45.52500000273118985, 31.93888565452638417 ) ) ;
#28210 = CARTESIAN_POINT ( 'NONE',  ( 7.236395654485755280, 12.22499999726881015, 22.27133577429736988 ) ) ;
#28211 = ORIENTED_EDGE ( 'NONE', *, *, #33703, .T. ) ;
#28212 = CARTESIAN_POINT ( 'NONE',  ( 27.16883889988623935, 52.57500000273117280, -19.73931689729374384 ) ) ;
#28213 = CARTESIAN_POINT ( 'NONE',  ( 10.04305231718579705, 42.60000000000000142, 30.90933677959248982 ) ) ;
#28214 = CARTESIAN_POINT ( 'NONE',  ( 7.025853678916403666, 44.94829833425730925, -26.06988505166735237 ) ) ;
#28215 = CARTESIAN_POINT ( 'NONE',  ( 27.16883889988624290, 74.17500000273119554, 19.73931689729373673 ) ) ;
#28216 = VERTEX_POINT ( 'NONE', #12906 ) ;
#28217 = CARTESIAN_POINT ( 'NONE',  ( -20.75514604977248823, 28.82500000273116569, -28.56700777964554305 ) ) ;
#28218 = CARTESIAN_POINT ( 'NONE',  ( -26.00068869287368756, 18.73177083333332149, -15.01150461594595775 ) ) ;
#28219 = ORIENTED_EDGE ( 'NONE', *, *, #26732, .F. ) ;
#28220 =( BOUNDED_CURVE ( )  B_SPLINE_CURVE ( 2, ( #29807, #6308, #27074, #1308, #13876, #8711, #19194, #17120, #3737, #645, #1138, #3568, #30137 ),
 .UNSPECIFIED., .F., .T. ) 
 B_SPLINE_CURVE_WITH_KNOTS ( ( 3, 2, 2, 2, 2, 2, 3 ),
 ( 0.5192307692307692735, 0.5205128205128205510, 0.5230769230769231060, 0.5256410256410256610, 0.5282051282051282159, 0.5307692307692307709, 0.5320512820512820484 ),
 .UNSPECIFIED. ) 
 CURVE ( )  GEOMETRIC_REPRESENTATION_ITEM ( )  RATIONAL_B_SPLINE_CURVE ( ( 0.9755282581475768211, 0.9755282581475768211, 1.000000000000000000, 0.9510565162951535312, 1.000000000000000000, 0.9510565162951535312, 1.000000000000000000, 0.9510565162951535312, 1.000000000000000000, 0.9510565162951535312, 1.000000000000000000, 0.9755282581475768211, 0.9755282581475768211 ) ) 
 REPRESENTATION_ITEM ( '' )  );
#28221 = CARTESIAN_POINT ( 'NONE',  ( 10.04305231718579705, 29.10000000546236620, 30.90933677959248982 ) ) ;
#28222 = CARTESIAN_POINT ( 'NONE',  ( -27.16883889988624290, 66.92500000273119554, -19.73931689729374028 ) ) ;
#28223 = CARTESIAN_POINT ( 'NONE',  ( 20.50609665440969565, 43.79687500000000000, -20.50609665441004736 ) ) ;
#28224 = EDGE_CURVE ( 'NONE', #20971, #8792, #23380, .T. ) ;
#28225 = CARTESIAN_POINT ( 'NONE',  ( 7.570916362186207671, 9.599999999999997868, 23.30088464923126779 ) ) ;
#28226 = DIRECTION ( 'NONE',  ( -0.000000000000000000, -1.000000000000000000, -0.000000000000000000 ) ) ;
#28227 = CARTESIAN_POINT ( 'NONE',  ( -20.75514604977248823, 10.82500000273118701, -28.56700777964554305 ) ) ;
#28228 = CARTESIAN_POINT ( 'NONE',  ( 15.31593959127081739, -56.96472381958990638, 1.875691223536068310E-15 ) ) ;
#28229 = CARTESIAN_POINT ( 'NONE',  ( -7.543491769121917656, 52.09857666574269075, -28.00173670424536354 ) ) ;
#28230 = CARTESIAN_POINT ( 'NONE',  ( 2.897257156509938333E-15, 76.50000000000001421, 15.77193336357400710 ) ) ;
#28231 = DIRECTION ( 'NONE',  ( -0.000000000000000000, -1.000000000000000000, -0.000000000000000000 ) ) ;
#28232 = CARTESIAN_POINT ( 'NONE',  ( -4.934616302121927505E-14, 70.50000000000000000, 32.50000000000000000 ) ) ;
#28233 = EDGE_CURVE ( 'NONE', #32300, #21391, #31410, .T. ) ;
#28234 = CARTESIAN_POINT ( 'NONE',  ( 19.82091636218621389, 15.94999999453763984, -14.40073868116559197 ) ) ;
#28235 = CARTESIAN_POINT ( 'NONE',  ( -15.00000000000000000, 76.25000000546239676, 0.000000000000000000 ) ) ;
#28236 = CARTESIAN_POINT ( 'NONE',  ( -26.07999730980490583, 25.46354166666666430, -6.988114217767815717 ) ) ;
#28237 = CARTESIAN_POINT ( 'NONE',  ( 10.37757302488624056, 32.52500000273117564, -31.93888565452638417 ) ) ;
#28238 = CARTESIAN_POINT ( 'NONE',  ( -15.00000000000000000, 82.00000000000001421, 0.000000000000000000 ) ) ;
#28239 = CARTESIAN_POINT ( 'NONE',  ( 33.58253175000000113, 42.47500000273119980, -10.91162601494193751 ) ) ;
#28240 = CARTESIAN_POINT ( 'NONE',  ( 10.37757302488624056, 22.77500000273119340, -31.93888565452638417 ) ) ;
#28241 = CARTESIAN_POINT ( 'NONE',  ( 0.000000000000000000, -21.99999999999999645, 0.000000000000000000 ) ) ;
#28242 = EDGE_CURVE ( 'NONE', #12293, #5896, #8419, .T. ) ;
#28243 = CARTESIAN_POINT ( 'NONE',  ( -2.162160676586882350E-15, 74.62500000273116996, -35.31076352940722529 ) ) ;
#28244 =( GEOMETRIC_REPRESENTATION_CONTEXT ( 3 ) GLOBAL_UNCERTAINTY_ASSIGNED_CONTEXT ( ( #31115 ) ) GLOBAL_UNIT_ASSIGNED_CONTEXT ( ( #33213, #22585, #14529 ) ) REPRESENTATION_CONTEXT ( 'NONE', 'WORKASPACE' ) );
#28245 = CARTESIAN_POINT ( 'NONE',  ( 4.445600272181915325E-13, 26.00000000546237189, -32.50000000000000000 ) ) ;
#28246 = CARTESIAN_POINT ( 'NONE',  ( 20.08610463437157279, 63.30000000000001137, -27.64615127144129758 ) ) ;
#28247 = CARTESIAN_POINT ( 'NONE',  ( 23.41746824999999887, 16.72499999726881725, -7.608796670333727974 ) ) ;
#28248 = CARTESIAN_POINT ( 'NONE',  ( 6.486482029760648627E-15, 65.62500000273116996, 35.31076352940722529 ) ) ;
#28249 = CARTESIAN_POINT ( 'NONE',  ( -3.880418787951142701, 11.19874571299077637, 24.49999999999999645 ) ) ;
#28250 = CARTESIAN_POINT ( 'NONE',  ( -19.11951029504797006, 48.37461833240936215, -19.06425588902558133 ) ) ;
#28251 = CARTESIAN_POINT ( 'NONE',  ( 33.58253175000000823, 70.27500000273118985, 10.91162601494192863 ) ) ;
#28252 = CARTESIAN_POINT ( 'NONE',  ( 10.37757302488624767, 3.725000002731182480, 31.93888565452638417 ) ) ;
#28253 = CARTESIAN_POINT ( 'NONE',  ( 23.41746825000000243, 9.224999997268820806, -7.608796670333727974 ) ) ;
#28254 = CARTESIAN_POINT ( 'NONE',  ( -19.09188309203660694, 62.70312500000000000, 19.09188309203694800 ) ) ;
#28255 = ORIENTED_EDGE ( 'NONE', *, *, #15561, .F. ) ;
#28256 = CARTESIAN_POINT ( 'NONE',  ( 27.16883889988623935, 50.32500000273120122, -19.73931689729374384 ) ) ;
#28257 = ORIENTED_EDGE ( 'NONE', *, *, #27172, .F. ) ;
#28258 = CARTESIAN_POINT ( 'NONE',  ( 20.50609665441005092, 30.90624999999999645, 20.50609665440969209 ) ) ;
#28259 = CARTESIAN_POINT ( 'NONE',  ( 14.97647472619947351, 35.92486083425730214, 26.02091320914850314 ) ) ;
#28260 = LINE ( 'NONE', #20891, #8377 ) ;
#28261 = CARTESIAN_POINT ( 'NONE',  ( 10.04305231718578817, 7.900000005462357144, -30.90933677959249337 ) ) ;
#28262 = DIRECTION ( 'NONE',  ( -0.000000000000000000, -1.000000000000000000, -0.000000000000000000 ) ) ;
#28263 = CARTESIAN_POINT ( 'NONE',  ( -7.236395654485757944, 5.724999997268803931, -22.27133577429736988 ) ) ;
#28264 = CARTESIAN_POINT ( 'NONE',  ( -18.94512977948576093, 9.824999997268824004, 13.76444248337722698 ) ) ;
#28265 = CARTESIAN_POINT ( 'NONE',  ( 20.75514604977249178, 14.07500000273119944, 28.56700777964553950 ) ) ;
#28266 = CARTESIAN_POINT ( 'NONE',  ( -20.08610463437157989, 26.20000000546237828, -27.64615127144129758 ) ) ;
#28267 = CARTESIAN_POINT ( 'NONE',  ( 10.04305231718578817, 67.40000000000001990, -30.90933677959249337 ) ) ;
#28268 = CARTESIAN_POINT ( 'NONE',  ( 9.270509831248421762, 77.55000000546237970, -12.75976212528059861 ) ) ;
#28269 = CARTESIAN_POINT ( 'NONE',  ( -5.147494310547430452, 29.55125428154684997, -32.49999999999999289 ) ) ;
#28270 = CARTESIAN_POINT ( 'NONE',  ( -28.02196122052045268, 64.42746500092397355, 7.468012846824790607 ) ) ;
#28271 = CARTESIAN_POINT ( 'NONE',  ( 33.58253175000000113, 32.37500000273119127, -4.112674001490185761E-15 ) ) ;
#28272 = CARTESIAN_POINT ( 'NONE',  ( 26.29305231718578995, 43.70000000546237118, -19.10302069950538240 ) ) ;
#28273 = CARTESIAN_POINT ( 'NONE',  ( -7.505752307973343918, 36.34895833333333570, -28.01184896238290989 ) ) ;
#28274 = CARTESIAN_POINT ( 'NONE',  ( -23.41746824999999887, 18.12499999726882649, -2.867812753649727150E-15 ) ) ;
#28275 = CARTESIAN_POINT ( 'NONE',  ( 20.08610463437157279, 7.300000000000001599, -27.64615127144129758 ) ) ;
#28276 = CARTESIAN_POINT ( 'NONE',  ( -26.29305231718579350, 51.80000000000001137, -19.10302069950537884 ) ) ;
#28277 = CARTESIAN_POINT ( 'NONE',  ( -26.06988505166722803, 51.23920166574269786, 7.025853678916877953 ) ) ;
#28278 = CARTESIAN_POINT ( 'NONE',  ( -20.75514604977248112, 47.42500000273118843, 28.56700777964554661 ) ) ;
#28279 = AXIS2_PLACEMENT_3D ( 'NONE', #22324, #24718, #1195 ) ;
#28280 = CARTESIAN_POINT ( 'NONE',  ( 6.486482029760649416E-15, 61.87500000273117706, 35.31076352940723240 ) ) ;
#28281 = CARTESIAN_POINT ( 'NONE',  ( 20.75514604977249178, 38.07500000273115859, 28.56700777964553950 ) ) ;
#28282 = CYLINDRICAL_SURFACE ( 'NONE', #3039, 24.50000000000000000 ) ;
#28283 = CARTESIAN_POINT ( 'NONE',  ( -24.20753774853730889, 14.72135416666666607, 13.97622843553634020 ) ) ;
#28284 = CARTESIAN_POINT ( 'NONE',  ( 32.50000000000000000, 15.50000000546236656, -3.980102097228898626E-15 ) ) ;
#28285 = CARTESIAN_POINT ( 'NONE',  ( 5.147494310547426899, 51.94874572391552903, -32.50000000000000000 ) ) ;
#28286 = FACE_OUTER_BOUND ( 'NONE', #18489, .T. ) ;
#28287 = CARTESIAN_POINT ( 'NONE',  ( -33.58253175000000113, 19.22500000273118204, 10.91162601494193929 ) ) ;
#28288 = CARTESIAN_POINT ( 'NONE',  ( -1.778240108872766143E-15, 7.500000000000001776, -32.49999999999999289 ) ) ;
#28289 = CARTESIAN_POINT ( 'NONE',  ( 7.313012447739250820E-14, 13.24999999453762456, 24.50000000000000000 ) ) ;
#28290 = CARTESIAN_POINT ( 'NONE',  ( -19.11951029504797006, 13.99961833240935327, -19.06425588902558133 ) ) ;
#28291 = CARTESIAN_POINT ( 'NONE',  ( -2.092463501923844636E-15, 44.00000000546238965, -34.17252228774368916 ) ) ;
#28292 = CARTESIAN_POINT ( 'NONE',  ( 15.00000000000000000, 71.35000000546237686, -4.873795443493596835 ) ) ;
#28293 = CARTESIAN_POINT ( 'NONE',  ( -2.162160676586882350E-15, 26.62500000273118417, -35.31076352940722529 ) ) ;
#28294 = CARTESIAN_POINT ( 'NONE',  ( -6.988114217767819270, 34.91666666666666430, 26.07999730980490583 ) ) ;
#28295 =( REPRESENTATION_RELATIONSHIP ('NONE','NONE', #5873, #3268 ) REPRESENTATION_RELATIONSHIP_WITH_TRANSFORMATION ( #2873 )SHAPE_REPRESENTATION_RELATIONSHIP( ) );
#28296 = VERTEX_POINT ( 'NONE', #21648 ) ;
#28297 = CARTESIAN_POINT ( 'NONE',  ( -10.37757302488623701, 67.52500000273118985, 31.93888565452638417 ) ) ;
#28298 = CARTESIAN_POINT ( 'NONE',  ( -20.50609665441004736, 42.93750000000000000, -20.50609665440969565 ) ) ;
#28299 = DIRECTION ( 'NONE',  ( 0.000000000000000000, 0.000000000000000000, 1.000000000000000000 ) ) ;
#28300 = ORIENTED_EDGE ( 'NONE', *, *, #10286, .T. ) ;
#28301 = CARTESIAN_POINT ( 'NONE',  ( -14.97647472619946285, 54.83111083425730214, -26.02091320914851025 ) ) ;
#28302 = CARTESIAN_POINT ( 'NONE',  ( 19.11951029504763611, 62.42225666759065206, -19.06425588902591173 ) ) ;
#28303 = CARTESIAN_POINT ( 'NONE',  ( -10.37757302488624411, 10.72500000273117493, -31.93888565452638417 ) ) ;
#28304 = CARTESIAN_POINT ( 'NONE',  ( -28.01184896238290278, 66.42708333333332860, 7.505752307973363457 ) ) ;
#28305 = CARTESIAN_POINT ( 'NONE',  ( -26.29305231718579350, 45.80000000000000426, -19.10302069950537884 ) ) ;
#28306 = CARTESIAN_POINT ( 'NONE',  ( -20.75514604977248112, 37.67500000273118133, 28.56700777964554661 ) ) ;
#28307 = CARTESIAN_POINT ( 'NONE',  ( 10.04305231718578817, 45.90000000546237402, -30.90933677959249337 ) ) ;
#28308 = CARTESIAN_POINT ( 'NONE',  ( 15.00000000000000000, 75.00000000000001421, -1.836970198721029589E-15 ) ) ;
#28309 = CARTESIAN_POINT ( 'NONE',  ( 27.16883889988624290, 23.92500000273117777, 19.73931689729373673 ) ) ;
#28310 = CARTESIAN_POINT ( 'NONE',  ( 19.82091636218621034, 13.54999999453762527, 14.40073868116559730 ) ) ;
#28311 = CARTESIAN_POINT ( 'NONE',  ( -10.37757302488623701, 47.77500000273118985, 31.93888565452638417 ) ) ;
#28312 = CARTESIAN_POINT ( 'NONE',  ( 26.29305231718579350, 26.80000000000000426, 19.10302069950537529 ) ) ;
#28313 = CARTESIAN_POINT ( 'NONE',  ( -20.08610463437157989, 29.69999999999999574, -27.64615127144129758 ) ) ;
#28314 = CARTESIAN_POINT ( 'NONE',  ( -23.41746825000000243, 17.52499999726881796, -7.608796670333730638 ) ) ;
#28315 =( BOUNDED_CURVE ( )  B_SPLINE_CURVE ( 2, ( #33148, #28359, #9652, #12913, #33500, #20132, #30751, #4846, #10003, #7073, #20301, #9475, #15327 ),
 .UNSPECIFIED., .F., .T. ) 
 B_SPLINE_CURVE_WITH_KNOTS ( ( 3, 2, 2, 2, 2, 2, 3 ),
 ( 0.8397435897435897578, 0.8410256410256410353, 0.8435897435897435903, 0.8461538461538461453, 0.8487179487179487003, 0.8512820512820512553, 0.8525641025641025328 ),
 .UNSPECIFIED. ) 
 CURVE ( )  GEOMETRIC_REPRESENTATION_ITEM ( )  RATIONAL_B_SPLINE_CURVE ( ( 0.9755282581475768211, 0.9755282581475768211, 1.000000000000000000, 0.9510565162951535312, 1.000000000000000000, 0.9510565162951535312, 1.000000000000000000, 0.9510565162951535312, 1.000000000000000000, 0.9510565162951535312, 1.000000000000000000, 0.9755282581475768211, 0.9755282581475768211 ) ) 
 REPRESENTATION_ITEM ( '' )  );
#28316 = CARTESIAN_POINT ( 'NONE',  ( -33.58253175000000113, 71.12500000273119838, 0.000000000000000000 ) ) ;
#28317 = DIRECTION ( 'NONE',  ( 0.000000000000000000, 1.000000000000000000, 0.000000000000000000 ) ) ;
#28318 = CARTESIAN_POINT ( 'NONE',  ( 3.306546357697853733E-15, -12.99999999999999822, -27.00000000000000000 ) ) ;
#28319 = CARTESIAN_POINT ( 'NONE',  ( -33.58253175000000113, 57.47500000273118559, 10.91162601494193929 ) ) ;
#28320 = CARTESIAN_POINT ( 'NONE',  ( -12.13525491562420910, 70.45000000546237118, 8.816778784387098611 ) ) ;
#28321 = CARTESIAN_POINT ( 'NONE',  ( -27.16883889988624290, 18.92500000273117422, -19.73931689729374028 ) ) ;
#28322 = CARTESIAN_POINT ( 'NONE',  ( 15.14183272437241889, 9.449999994537636283, 20.84094480462498211 ) ) ;
#28323 = CARTESIAN_POINT ( 'NONE',  ( -24.18731323226248264, 20.16965250092397355, -14.01125832528284931 ) ) ;
#28324 = ADVANCED_FACE ( 'NONE', ( #6018 ), #31918, .T. ) ;
#28325 = CARTESIAN_POINT ( 'NONE',  ( -32.50000000000000000, 26.09999999999999076, 10.55989012756946366 ) ) ;
#28326 = CARTESIAN_POINT ( 'NONE',  ( 27.16883889988623935, 42.32500000273119412, -19.73931689729374384 ) ) ;
#28327 = CARTESIAN_POINT ( 'NONE',  ( 11.54700538379251107, 86.00000000000001421, -19.99999999999999645 ) ) ;
#28328 = CARTESIAN_POINT ( 'NONE',  ( 10.37757302488624767, 57.97500000273118559, 31.93888565452638417 ) ) ;
#28329 = CARTESIAN_POINT ( 'NONE',  ( 15.04653450569292872, 48.52902750092398065, -25.98046417659857710 ) ) ;
#28330 = ADVANCED_FACE ( 'NONE', ( #5311 ), #1440, .F. ) ;
#28331 = CARTESIAN_POINT ( 'NONE',  ( 19.82091636218621389, 6.200000000000010836, -14.40073868116559197 ) ) ;
#28332 = VECTOR ( 'NONE', #29872, 1000.000000000000000 ) ;
#28333 = CARTESIAN_POINT ( 'NONE',  ( 15.04653450569339945, 36.48659749907601935, 25.98046417659831775 ) ) ;
#28334 = CARTESIAN_POINT ( 'NONE',  ( 10.04305231718579705, 59.10000000546237686, 30.90933677959248982 ) ) ;
#28335 = CARTESIAN_POINT ( 'NONE',  ( -8.960552108402742093E-16, 76.87500000273118417, -14.63369212191046387 ) ) ;
#28336 = CARTESIAN_POINT ( 'NONE',  ( 20.08610463437158344, 62.69999999999998863, 27.64615127144129403 ) ) ;
#28337 = CARTESIAN_POINT ( 'NONE',  ( 26.06988505166722803, 63.27045166574269075, -7.025853678916862854 ) ) ;
#28338 = CARTESIAN_POINT ( 'NONE',  ( 3.880418787951139148, 0.4487457184531665200, -24.50000000000000000 ) ) ;
#28339 = CIRCLE ( 'NONE', #382, 26.50000000000000355 ) ;
#28340 = CARTESIAN_POINT ( 'NONE',  ( 32.50000000000000000, 77.60000000546239107, -10.55989012756945833 ) ) ;
#28341 = CARTESIAN_POINT ( 'NONE',  ( 15.01150461594596308, 12.71614583333333037, -26.00068869287367335 ) ) ;
#28342 = CARTESIAN_POINT ( 'NONE',  ( -33.58253175000000113, 33.27500000273120406, -10.91162601494193218 ) ) ;
#28343 = CARTESIAN_POINT ( 'NONE',  ( -14.47279130897151767, 9.824999997268800911, -19.92008829642072598 ) ) ;
#28344 = ORIENTED_EDGE ( 'NONE', *, *, #18507, .T. ) ;
#28345 = CARTESIAN_POINT ( 'NONE',  ( 6.486482029760649416E-15, 77.87500000273118417, 35.31076352940723240 ) ) ;
#28346 = CARTESIAN_POINT ( 'NONE',  ( 20.08610463437158344, 23.20000000546238539, 27.64615127144129403 ) ) ;
#28347 = CARTESIAN_POINT ( 'NONE',  ( 7.505752307973351023, 44.94270833333332860, 28.01184896238290278 ) ) ;
#28348 = CARTESIAN_POINT ( 'NONE',  ( 6.486482029760649416E-15, 55.87500000273118417, 35.31076352940723240 ) ) ;
#28349 = CARTESIAN_POINT ( 'NONE',  ( -32.50000000000000000, 60.60000000546239107, 10.55989012756946366 ) ) ;
#28350 = ORIENTED_EDGE ( 'NONE', *, *, #17349, .T. ) ;
#28351 = DIRECTION ( 'NONE',  ( -1.224646799147353454E-16, 1.000000000000000000, -0.000000000000000000 ) ) ;
#28352 = CARTESIAN_POINT ( 'NONE',  ( 33.58253175000000113, 42.12500000273116996, -4.112674001490185761E-15 ) ) ;
#28353 = LINE ( 'NONE', #2092, #17616 ) ;
#28354 = CARTESIAN_POINT ( 'NONE',  ( 33.58253175000000823, 66.27500000273118985, 10.91162601494192863 ) ) ;
#28355 = CARTESIAN_POINT ( 'NONE',  ( -26.29305231718578995, 2.700000005462388497, 19.10302069950538595 ) ) ;
#28356 = CARTESIAN_POINT ( 'NONE',  ( -27.16883889988624290, 60.92500000273119554, -19.73931689729374028 ) ) ;
#28357 = DIRECTION ( 'NONE',  ( -0.000000000000000000, -1.000000000000000000, -0.000000000000000000 ) ) ;
#28358 = CARTESIAN_POINT ( 'NONE',  ( -2.092463501923844636E-15, 45.49999999999998579, -34.17252228774368916 ) ) ;
#28359 = CARTESIAN_POINT ( 'NONE',  ( -5.147494310547423346, 14.44874571845315536, 32.50000000000000000 ) ) ;
#28360 = CARTESIAN_POINT ( 'NONE',  ( 10.37757302488624056, 14.77500000273118630, -31.93888565452638417 ) ) ;
#28361 = CARTESIAN_POINT ( 'NONE',  ( -20.08610463437157989, 73.70000000000000284, -27.64615127144129758 ) ) ;
#28362 = CARTESIAN_POINT ( 'NONE',  ( -19.06425588902558133, 26.89024333240934439, 19.11951029504797006 ) ) ;
#28363 = CARTESIAN_POINT ( 'NONE',  ( -13.91746824999999887, 70.87500000273119838, 0.000000000000000000 ) ) ;
#28364 = CARTESIAN_POINT ( 'NONE',  ( -1.778240108872766143E-15, 68.00000000546238255, -32.49999999999999289 ) ) ;
#28365 = CARTESIAN_POINT ( 'NONE',  ( 32.50000000000000711, 53.40000000546238113, 10.55989012756945122 ) ) ;
#28366 = CARTESIAN_POINT ( 'NONE',  ( 10.37757302488624767, 77.97500000273120691, 31.93888565452638417 ) ) ;
#28367 = ORIENTED_EDGE ( 'NONE', *, *, #7482, .T. ) ;
#28368 = CARTESIAN_POINT ( 'NONE',  ( -14.47279130897152122, 10.42499999726881299, 19.92008829642072243 ) ) ;
#28369 = CARTESIAN_POINT ( 'NONE',  ( -23.41746825000000243, 3.724999997268820362, 7.608796670333725309 ) ) ;
#28370 = CARTESIAN_POINT ( 'NONE',  ( -13.97622843553588901, 48.80989583333332860, 24.20753774853756823 ) ) ;
#28371 = CARTESIAN_POINT ( 'NONE',  ( -33.58253175000000113, 63.02500000273118985, -10.91162601494193218 ) ) ;
#28372 = CARTESIAN_POINT ( 'NONE',  ( -10.37757302488624411, 16.97500000273118204, -31.93888565452638417 ) ) ;
#28373 = CARTESIAN_POINT ( 'NONE',  ( 6.486482029760649416E-15, 7.875000002731177950, 35.31076352940723240 ) ) ;
#28374 = CARTESIAN_POINT ( 'NONE',  ( 26.07999730980477437, 30.33333333333332860, -6.988114217768290004 ) ) ;
#28375 = CARTESIAN_POINT ( 'NONE',  ( 20.53372385742072481, 17.73475666759064140, -20.47846945139902175 ) ) ;
#28376 = CARTESIAN_POINT ( 'NONE',  ( 15.01150461594643204, 61.98697916666665009, 26.00068869287340334 ) ) ;
#28377 = CARTESIAN_POINT ( 'NONE',  ( -10.37757302488623701, 5.525000002731192517, 31.93888565452638417 ) ) ;
#28378 = CARTESIAN_POINT ( 'NONE',  ( 11.25946833292375793, 74.17500000273119554, 8.180482586598731842 ) ) ;
#28379 = CARTESIAN_POINT ( 'NONE',  ( -26.29305231718579350, 43.79999999999999005, -19.10302069950537884 ) ) ;
#28380 = CARTESIAN_POINT ( 'NONE',  ( -10.37757302488624411, 46.72500000273119269, -31.93888565452638417 ) ) ;
#28381 = CARTESIAN_POINT ( 'NONE',  ( -23.41746825000000598, 9.724999997268804819, 7.608796670333726198 ) ) ;
#28382 = CARTESIAN_POINT ( 'NONE',  ( 20.08610463437157279, 21.80000000546236549, -27.64615127144129758 ) ) ;
#28383 = EDGE_LOOP ( 'NONE', ( #8872, #4916, #21183, #21434 ) ) ;
#28384 = CARTESIAN_POINT ( 'NONE',  ( -20.75514604977248823, 57.07500000273117280, -28.56700777964554305 ) ) ;
#28385 = CARTESIAN_POINT ( 'NONE',  ( 20.08610463437158344, 42.69999999999998153, 27.64615127144129403 ) ) ;
#28386 = CARTESIAN_POINT ( 'NONE',  ( 19.06425588902592239, 39.21913166759063785, 19.11951029504763611 ) ) ;
#28387 = CARTESIAN_POINT ( 'NONE',  ( -33.58253175000000113, 73.27500000273118985, -10.91162601494193218 ) ) ;
#28388 = ORIENTED_EDGE ( 'NONE', *, *, #12946, .T. ) ;
#28389 = CARTESIAN_POINT ( 'NONE',  ( -33.58253175000000113, 25.02500000273117209, -10.91162601494193218 ) ) ;
#28390 = DIRECTION ( 'NONE',  ( 0.000000000000000000, -1.000000000000000000, 0.000000000000000000 ) ) ;
#28391 = ORIENTED_EDGE ( 'NONE', *, *, #9780, .F. ) ;
#28392 = CARTESIAN_POINT ( 'NONE',  ( -5.147494310547423346, 58.44874571845313938, 32.50000000000000000 ) ) ;
#28393 = CARTESIAN_POINT ( 'NONE',  ( -27.16883889988623935, 59.32500000273119412, 19.73931689729374739 ) ) ;
#28394 = CARTESIAN_POINT ( 'NONE',  ( 28.01184896238290278, 44.08333333333332860, -7.505752307973347470 ) ) ;
#28395 = CARTESIAN_POINT ( 'NONE',  ( 7.570916362186213000, 12.39999999999999503, -23.30088464923126423 ) ) ;
#28396 = CARTESIAN_POINT ( 'NONE',  ( -18.94512977948575738, 1.924999997268805885, -13.76444248337723231 ) ) ;
#28397 = CARTESIAN_POINT ( 'NONE',  ( 20.75514604977248467, 8.425000002731204418, -28.56700777964554305 ) ) ;
#28398 = CARTESIAN_POINT ( 'NONE',  ( 32.50000000000000711, 28.89999999999998792, 10.55989012756945122 ) ) ;
#28399 = CARTESIAN_POINT ( 'NONE',  ( 20.47846945139867003, 56.10899333240935505, -20.53372385742107653 ) ) ;
#28400 = CARTESIAN_POINT ( 'NONE',  ( 32.50000000000000000, 37.00000000000000711, -3.980102097228898626E-15 ) ) ;
#28401 = CARTESIAN_POINT ( 'NONE',  ( -2.584737979205442066E-13, 63.99218749999997868, -30.02300923189239867 ) ) ;
#28402 = CARTESIAN_POINT ( 'NONE',  ( 32.50000000000000000, 55.09999999999997300, -10.55989012756945833 ) ) ;
#28403 = CARTESIAN_POINT ( 'NONE',  ( 20.08610463437158344, 14.70000000000000107, 27.64615127144129403 ) ) ;
#28404 = CARTESIAN_POINT ( 'NONE',  ( -24.50000000000001066, 10.84999999453761887, 7.960532557706201828 ) ) ;
#28405 = CARTESIAN_POINT ( 'NONE',  ( 2.688165632520823219E-15, 79.37500000273119838, 14.63369212191046387 ) ) ;
#28406 = CARTESIAN_POINT ( 'NONE',  ( -6.988114217768288228, 19.16145833333332860, -26.07999730980477437 ) ) ;
#28407 = CARTESIAN_POINT ( 'NONE',  ( 33.58253175000000113, 32.12500000273119127, -4.112674001490185761E-15 ) ) ;
#28408 = CARTESIAN_POINT ( 'NONE',  ( 12.13525491562421088, 74.80000000000003979, 8.816778784387095058 ) ) ;
#28409 = CARTESIAN_POINT ( 'NONE',  ( -20.75514604977248823, 41.07500000273119412, -28.56700777964554305 ) ) ;
#28410 = CARTESIAN_POINT ( 'NONE',  ( 6.486482029760648627E-15, 21.87500000273118772, 35.31076352940722529 ) ) ;
#28411 = CARTESIAN_POINT ( 'NONE',  ( -26.29305231718579350, 67.79999999999999716, -19.10302069950537884 ) ) ;
#28412 = CARTESIAN_POINT ( 'NONE',  ( -33.58253175000000113, 75.22500000273119269, 10.91162601494193929 ) ) ;
#28413 = CARTESIAN_POINT ( 'NONE',  ( 24.50000000000000000, 8.000000000000007105, 0.000000000000000000 ) ) ;
#28414 = CARTESIAN_POINT ( 'NONE',  ( 32.50000000000000000, 61.09999999999998721, -10.55989012756945833 ) ) ;
#28415 = CARTESIAN_POINT ( 'NONE',  ( 7.236395654485755280, 16.22499999726881370, 22.27133577429736988 ) ) ;
#28416 = CARTESIAN_POINT ( 'NONE',  ( -33.58253175000000113, 65.22500000273117848, 10.91162601494193929 ) ) ;
#28417 =( BOUNDED_CURVE ( )  B_SPLINE_CURVE ( 2, ( #25474, #9852, #4874, #31127, #30779, #23068, #26153, #7619, #2123, #30604, #18099, #28546, #13110 ),
 .UNSPECIFIED., .F., .T. ) 
 B_SPLINE_CURVE_WITH_KNOTS ( ( 3, 2, 2, 2, 2, 2, 3 ),
 ( 0.9423076923076922906, 0.9435897435897435681, 0.9461538461538461231, 0.9487179487179486781, 0.9512820512820512331, 0.9538461538461538991, 0.9551282051282051766 ),
 .UNSPECIFIED. ) 
 CURVE ( )  GEOMETRIC_REPRESENTATION_ITEM ( )  RATIONAL_B_SPLINE_CURVE ( ( 0.9755282581475768211, 0.9755282581475768211, 1.000000000000000000, 0.9510565162951535312, 1.000000000000000000, 0.9510565162951535312, 1.000000000000000000, 0.9510565162951535312, 1.000000000000000000, 0.9510565162951535312, 1.000000000000000000, 0.9755282581475768211, 0.9755282581475768211 ) ) 
 REPRESENTATION_ITEM ( '' )  );
#28418 = CARTESIAN_POINT ( 'NONE',  ( 18.94512977948576093, 9.324999997268824004, -13.76444248337722875 ) ) ;
#28419 = CARTESIAN_POINT ( 'NONE',  ( 33.58253175000000113, 72.37500000273118417, -4.112674001490185761E-15 ) ) ;
#28420 =( BOUNDED_CURVE ( )  B_SPLINE_CURVE ( 2, ( #23550, #17721, #33669, #12391, #9817, #33492, #23035, #7587, #22861, #20650, #25776, #10338, #10166 ),
 .UNSPECIFIED., .F., .T. ) 
 B_SPLINE_CURVE_WITH_KNOTS ( ( 3, 2, 2, 2, 2, 2, 3 ),
 ( 0.8653846153846154188, 0.8666666666666666963, 0.8692307692307692513, 0.8717948717948718063, 0.8743589743589743613, 0.8769230769230769162, 0.8782051282051281937 ),
 .UNSPECIFIED. ) 
 CURVE ( )  GEOMETRIC_REPRESENTATION_ITEM ( )  RATIONAL_B_SPLINE_CURVE ( ( 0.9755282581475768211, 0.9755282581475768211, 1.000000000000000000, 0.9510565162951535312, 1.000000000000000000, 0.9510565162951535312, 1.000000000000000000, 0.9510565162951535312, 1.000000000000000000, 0.9510565162951535312, 1.000000000000000000, 0.9755282581475768211, 0.9755282581475768211 ) ) 
 REPRESENTATION_ITEM ( '' )  );
#28421 = CARTESIAN_POINT ( 'NONE',  ( -20.75514604977248823, 8.825000002731192339, -28.56700777964554305 ) ) ;
#28422 = CARTESIAN_POINT ( 'NONE',  ( -23.41746825000000243, 16.02499999726881086, -7.608796670333730638 ) ) ;
#28423 = CARTESIAN_POINT ( 'NONE',  ( -7.025853678916393008, 15.72954833425730925, 26.06988505166735592 ) ) ;
#28424 = ORIENTED_EDGE ( 'NONE', *, *, #30398, .T. ) ;
#28425 = CARTESIAN_POINT ( 'NONE',  ( 10.37757302488624056, 46.52500000273117564, -31.93888565452638417 ) ) ;
#28426 = ORIENTED_EDGE ( 'NONE', *, *, #6322, .T. ) ;
#28427 = CARTESIAN_POINT ( 'NONE',  ( 15.01150461594596308, 43.65364583333332860, -26.00068869287367335 ) ) ;
#28428 = CARTESIAN_POINT ( 'NONE',  ( 5.779280353836490358E-15, 40.49999999999999289, 32.49999999999999289 ) ) ;
#28429 = CARTESIAN_POINT ( 'NONE',  ( -26.29305231718579350, 2.300000005462377040, -19.10302069950537884 ) ) ;
#28430 = CARTESIAN_POINT ( 'NONE',  ( -7.570916362186210335, 2.599999999999991207, -23.30088464923126779 ) ) ;
#28431 = CARTESIAN_POINT ( 'NONE',  ( -23.41746825000000243, 2.024999997268815299, -7.608796670333730638 ) ) ;
#28432 = CARTESIAN_POINT ( 'NONE',  ( -23.41746824999999887, 9.624999997268817609, -2.867812753649727150E-15 ) ) ;
#28433 = CARTESIAN_POINT ( 'NONE',  ( 10.37757302488624767, 15.97500000273119269, 31.93888565452638417 ) ) ;
#28434 = CARTESIAN_POINT ( 'NONE',  ( 32.50000000000000711, 21.40000000546237757, 10.55989012756945122 ) ) ;
#28435 = CARTESIAN_POINT ( 'NONE',  ( -26.29305231718579350, 63.79999999999999716, -19.10302069950537884 ) ) ;
#28436 = CARTESIAN_POINT ( 'NONE',  ( 0.000000000000000000, 96.00000000000002842, -12.00000000000000000 ) ) ;
#28437 = CARTESIAN_POINT ( 'NONE',  ( 26.00068869287340334, 16.44010416666666430, -15.01150461594642316 ) ) ;
#28438 = CARTESIAN_POINT ( 'NONE',  ( 0.000000000000000000, 80.00000000000001421, 0.000000000000000000 ) ) ;
#28439 = CARTESIAN_POINT ( 'NONE',  ( 26.00068869287367690, 37.63802083333331439, 15.01150461594596486 ) ) ;
#28440 = ITEM_DEFINED_TRANSFORMATION ( 'NONE', 'NONE', #798,  #1376 ) ;
#28441 = CARTESIAN_POINT ( 'NONE',  ( 23.41746825000000243, 17.02499999726880731, 7.608796670333735079 ) ) ;
#28442 = CARTESIAN_POINT ( 'NONE',  ( -20.08610463437156923, 8.300000000000000711, 27.64615127144130113 ) ) ;
#28443 = CARTESIAN_POINT ( 'NONE',  ( 2.445080149700053643E-15, 74.50000000000001421, 15.00000000000000000 ) ) ;
#28444 = CARTESIAN_POINT ( 'NONE',  ( -24.22776226481266448, 51.66888916574269075, -13.94119854578892514 ) ) ;
#28445 = CARTESIAN_POINT ( 'NONE',  ( -27.16883889988623935, 49.32500000273118701, 19.73931689729374739 ) ) ;
#28446 = CARTESIAN_POINT ( 'NONE',  ( 27.16883889988623935, 60.57500000273117990, -19.73931689729374384 ) ) ;
#28447 = CARTESIAN_POINT ( 'NONE',  ( 33.58253175000000113, 42.37500000273119838, -4.112674001490185761E-15 ) ) ;
#28448 = CARTESIAN_POINT ( 'NONE',  ( 32.50000000000000000, 45.10000000000000142, -10.55989012756945833 ) ) ;
#28449 = CARTESIAN_POINT ( 'NONE',  ( -6.988114217768288228, 15.72395833333332860, -26.07999730980477437 ) ) ;
#28450 = CARTESIAN_POINT ( 'NONE',  ( 0.000000000000000000, 52.00000000000000711, 0.000000000000000000 ) ) ;
#28451 = EDGE_CURVE ( 'NONE', #26696, #28004, #14845, .T. ) ;
#28452 = CARTESIAN_POINT ( 'NONE',  ( 0.000000000000000000, 80.00000000000001421, 0.000000000000000000 ) ) ;
#28453 = DIRECTION ( 'NONE',  ( 0.000000000000000000, 0.000000000000000000, -1.000000000000000000 ) ) ;
#28454 = CARTESIAN_POINT ( 'NONE',  ( -20.75514604977248823, 12.82500000273119589, -28.56700777964554305 ) ) ;
#28455 = CARTESIAN_POINT ( 'NONE',  ( -10.04305231718578462, 62.90000000546236691, 30.90933677959249337 ) ) ;
#28456 = LINE ( 'NONE', #23491, #10076 ) ;
#28457 = CARTESIAN_POINT ( 'NONE',  ( 15.14183272437242422, 10.04999999453761639, -20.84094480462497856 ) ) ;
#28458 = CARTESIAN_POINT ( 'NONE',  ( -26.06988505166722803, 20.30170166574269075, 7.025853678916877953 ) ) ;
#28459 = CARTESIAN_POINT ( 'NONE',  ( -10.04305231718579172, 38.10000000546236265, -30.90933677959248982 ) ) ;
#28460 = CARTESIAN_POINT ( 'NONE',  ( -10.04305231718578462, 12.39999999999999503, 30.90933677959249337 ) ) ;
#28461 = CARTESIAN_POINT ( 'NONE',  ( 33.58253175000000113, 24.12500000273118417, -4.112674001490185761E-15 ) ) ;
#28462 = CARTESIAN_POINT ( 'NONE',  ( -24.20753774853756823, 42.79427083333331439, -13.97622843553588723 ) ) ;
#28463 = VERTEX_POINT ( 'NONE', #1612 ) ;
#28464 = CARTESIAN_POINT ( 'NONE',  ( -27.16883889988623935, 63.32500000273120833, 19.73931689729374739 ) ) ;
#28465 = CARTESIAN_POINT ( 'NONE',  ( 26.00068869287340334, 47.37760416666666430, -15.01150461594642316 ) ) ;
#28466 = ORIENTED_EDGE ( 'NONE', *, *, #12398, .T. ) ;
#28467 = CARTESIAN_POINT ( 'NONE',  ( 28.02196122052045268, 59.27121500092397355, -7.468012846824774620 ) ) ;
#28468 = CARTESIAN_POINT ( 'NONE',  ( 0.04044903254993986036, 61.99256916759065206, -27.95245687107223986 ) ) ;
#28469 = ORIENTED_EDGE ( 'NONE', *, *, #13461, .F. ) ;
#28470 = CARTESIAN_POINT ( 'NONE',  ( 10.37757302488624767, 9.725000002731173154, 31.93888565452638417 ) ) ;
#28471 = CARTESIAN_POINT ( 'NONE',  ( 15.04653450569339945, 19.29909749907602290, 25.98046417659831775 ) ) ;
#28472 = CARTESIAN_POINT ( 'NONE',  ( -10.04305231718578462, 46.39999999999999858, 30.90933677959249337 ) ) ;
#28473 = CARTESIAN_POINT ( 'NONE',  ( -27.16883889988624290, 35.17500000273118843, -19.73931689729374028 ) ) ;
#28474 = CARTESIAN_POINT ( 'NONE',  ( -20.08610463437157989, 38.20000000546236407, -27.64615127144129758 ) ) ;
#28475 = CARTESIAN_POINT ( 'NONE',  ( 15.00000000000000000, 77.00000000000001421, -1.836970198721029589E-15 ) ) ;
#28476 = DIRECTION ( 'NONE',  ( -1.000000000000000000, 0.000000000000000000, 0.000000000000000000 ) ) ;
#28477 = CARTESIAN_POINT ( 'NONE',  ( -33.58253175000000113, 25.02500000273117209, -10.91162601494193218 ) ) ;
#28478 = CARTESIAN_POINT ( 'NONE',  ( 24.50000000000000000, 5.849999994537632197, -7.960532557706203605 ) ) ;
#28479 = CARTESIAN_POINT ( 'NONE',  ( 33.58253175000000823, 50.27500000273118985, 10.91162601494192863 ) ) ;
#28480 = CARTESIAN_POINT ( 'NONE',  ( -2.092463501923844636E-15, 31.49999999999999289, -34.17252228774368916 ) ) ;
#28481 = CARTESIAN_POINT ( 'NONE',  ( 10.04305231718579705, 28.60000000000001563, 30.90933677959248982 ) ) ;
#28482 = CARTESIAN_POINT ( 'NONE',  ( 7.570916362186207671, 7.599999999999996092, 23.30088464923126779 ) ) ;
#28483 = CARTESIAN_POINT ( 'NONE',  ( 20.75514604977248467, 72.42500000273119554, -28.56700777964554305 ) ) ;
#28484 = CARTESIAN_POINT ( 'NONE',  ( 1.577395562988744260E-15, 2.249999994537629444, -25.76082449383753925 ) ) ;
#28485 = CARTESIAN_POINT ( 'NONE',  ( -33.58253175000000113, 59.27500000273119696, -10.91162601494193041 ) ) ;
#28486 = CARTESIAN_POINT ( 'NONE',  ( -20.08610463437157989, 40.20000000546236407, -27.64615127144129758 ) ) ;
#28487 = CARTESIAN_POINT ( 'NONE',  ( -33.58253175000000113, 15.02500000273120051, -10.91162601494193218 ) ) ;
#28488 = CARTESIAN_POINT ( 'NONE',  ( 26.06988505166735592, 28.62017333425730925, 7.025853678916393896 ) ) ;
#28489 = CARTESIAN_POINT ( 'NONE',  ( 28.18730216971810165, 66.99999999999998579, -16.82255561448983983 ) ) ;
#28490 = CARTESIAN_POINT ( 'NONE',  ( -10.37757302488623701, 35.52500000273118985, 31.93888565452638417 ) ) ;
#28491 = CARTESIAN_POINT ( 'NONE',  ( -26.29305231718579350, 64.30000000546236549, -19.10302069950537884 ) ) ;
#28492 = CARTESIAN_POINT ( 'NONE',  ( 10.04305231718579705, 18.60000000000000497, 30.90933677959248982 ) ) ;
#28493 = CARTESIAN_POINT ( 'NONE',  ( 15.14183272437242422, 16.30000000000000782, -20.84094480462497856 ) ) ;
#28494 = CARTESIAN_POINT ( 'NONE',  ( 28.02196122052058413, 42.93190999907601935, 7.468012846824272799 ) ) ;
#28495 = CARTESIAN_POINT ( 'NONE',  ( 20.08610463437158344, 61.20000000546237118, 27.64615127144129403 ) ) ;
#28496 = CARTESIAN_POINT ( 'NONE',  ( 4.300734207923757602, 76.77500000273118985, -13.23629886949340673 ) ) ;
#28497 = CARTESIAN_POINT ( 'NONE',  ( -13.91746824999999532, 78.77500000273118985, -4.522059556121115875 ) ) ;
#28498 = CARTESIAN_POINT ( 'NONE',  ( -6.950374756619247307, 64.41628499907602645, 26.09010956794245217 ) ) ;
#28499 = CARTESIAN_POINT ( 'NONE',  ( 20.08610463437157279, 73.80000000546239391, -27.64615127144129758 ) ) ;
#28500 = CARTESIAN_POINT ( 'NONE',  ( -20.50609665440969209, 21.45312499999999645, 20.50609665441005092 ) ) ;
#28501 = CARTESIAN_POINT ( 'NONE',  ( -27.16883889988624290, 37.17500000273120264, -19.73931689729374028 ) ) ;
#28502 = CARTESIAN_POINT ( 'NONE',  ( 14.47279130897151944, 5.424999997268823648, -19.92008829642072598 ) ) ;
#28503 = EDGE_LOOP ( 'NONE', ( #29714, #11826 ) ) ;
#28504 = CARTESIAN_POINT ( 'NONE',  ( 33.58253175000000113, 74.47500000273116427, -10.91162601494193751 ) ) ;
#28505 = CARTESIAN_POINT ( 'NONE',  ( -26.29305231718579350, 24.30000000546238326, -19.10302069950537884 ) ) ;
#28506 = CARTESIAN_POINT ( 'NONE',  ( 2.740863092043355209E-13, 41.64843750000000000, 30.02300923189239512 ) ) ;
#28507 = CARTESIAN_POINT ( 'NONE',  ( 30.02300923189239512, 64.85156249999998579, -2.619432448724977703E-13 ) ) ;
#28508 = CARTESIAN_POINT ( 'NONE',  ( 27.16883889988624290, 52.17500000273117422, 19.73931689729373673 ) ) ;
#28509 = CARTESIAN_POINT ( 'NONE',  ( 20.08610463437158344, 65.20000000546235697, 27.64615127144129403 ) ) ;
#28510 = ADVANCED_FACE ( 'NONE', ( #33011 ), #32349, .T. ) ;
#28511 =( BOUNDED_CURVE ( )  B_SPLINE_CURVE ( 2, ( #21284, #18032, #15962, #12868, #15795, #26080, #10465, #28478, #2739, #28644, #20943, #7882, #28817 ),
 .UNSPECIFIED., .F., .T. ) 
 B_SPLINE_CURVE_WITH_KNOTS ( ( 3, 2, 2, 2, 2, 2, 3 ),
 ( 0.1944444444444444475, 0.2000000000000000111, 0.2111111111111111105, 0.2222222222222222099, 0.2333333333333333370, 0.2444444444444444364, 0.2499999999999999722 ),
 .UNSPECIFIED. ) 
 CURVE ( )  GEOMETRIC_REPRESENTATION_ITEM ( )  RATIONAL_B_SPLINE_CURVE ( ( 0.9755282581475768211, 0.9755282581475768211, 1.000000000000000000, 0.9510565162951535312, 1.000000000000000000, 0.9510565162951535312, 1.000000000000000000, 0.9510565162951535312, 1.000000000000000000, 0.9510565162951535312, 1.000000000000000000, 0.9755282581475768211, 0.9755282581475768211 ) ) 
 REPRESENTATION_ITEM ( '' )  );
#28512 = CARTESIAN_POINT ( 'NONE',  ( 24.50000000000000000, 5.849999994537632197, -7.960532557706203605 ) ) ;
#28513 = CARTESIAN_POINT ( 'NONE',  ( -27.16883889988623935, 41.32500000273120122, 19.73931689729374739 ) ) ;
#28514 = CARTESIAN_POINT ( 'NONE',  ( 4.635254915624212657, 72.85000000546237686, 14.26584774442730286 ) ) ;
#28515 = CARTESIAN_POINT ( 'NONE',  ( 33.58253175000000823, 70.27500000273118985, 10.91162601494192863 ) ) ;
#28516 = ADVANCED_FACE ( 'NONE', ( #32678 ), #19658, .T. ) ;
#28517 = CARTESIAN_POINT ( 'NONE',  ( 32.50000000000000711, 5.400000005462390895, 10.55989012756945122 ) ) ;
#28518 = CARTESIAN_POINT ( 'NONE',  ( 33.58253175000000113, 62.12500000273117706, -4.112674001490185761E-15 ) ) ;
#28519 = FACE_OUTER_BOUND ( 'NONE', #32648, .T. ) ;
#28520 = CARTESIAN_POINT ( 'NONE',  ( 26.29305231718578995, 47.19999999999998863, -19.10302069950538240 ) ) ;
#28521 = DIRECTION ( 'NONE',  ( 0.000000000000000000, 0.000000000000000000, -1.000000000000000000 ) ) ;
#28522 = CARTESIAN_POINT ( 'NONE',  ( -10.37757302488623701, 7.775000002731180970, 31.93888565452638417 ) ) ;
#28523 = CARTESIAN_POINT ( 'NONE',  ( -7.570916362186215665, 7.399999999999989697, 23.30088464923126423 ) ) ;
#28524 = CARTESIAN_POINT ( 'NONE',  ( -24.22776226481266448, 31.04388916574268364, -13.94119854578892514 ) ) ;
#28525 = CARTESIAN_POINT ( 'NONE',  ( 13.91746824999999887, 78.37500000273116996, -1.704398294459741270E-15 ) ) ;
#28526 = CARTESIAN_POINT ( 'NONE',  ( -1.778240108872766143E-15, 48.00000000546238255, -32.49999999999999289 ) ) ;
#28527 = FACE_OUTER_BOUND ( 'NONE', #22424, .T. ) ;
#28528 = CARTESIAN_POINT ( 'NONE',  ( -20.75514604977248823, 73.07500000273115859, -28.56700777964554305 ) ) ;
#28529 = VERTEX_POINT ( 'NONE', #29767 ) ;
#28530 = CARTESIAN_POINT ( 'NONE',  ( -7.236395654485763274, 14.52499999726880553, 22.27133577429736633 ) ) ;
#28531 = CARTESIAN_POINT ( 'NONE',  ( -14.47279130897152299, 3.924999997268813878, 19.92008829642072243 ) ) ;
#28532 = CARTESIAN_POINT ( 'NONE',  ( 13.97622843553633665, 51.67447916666665719, 24.20753774853730889 ) ) ;
#28533 = CARTESIAN_POINT ( 'NONE',  ( -33.58253175000000113, 57.12500000273116996, 0.000000000000000000 ) ) ;
#28534 = CARTESIAN_POINT ( 'NONE',  ( -33.58253175000000113, 19.27500000273117919, -10.91162601494193218 ) ) ;
#28535 = CARTESIAN_POINT ( 'NONE',  ( -27.16883889988623935, 1.575000002731183457, 19.73931689729374739 ) ) ;
#28536 = CARTESIAN_POINT ( 'NONE',  ( -6.988114217768288228, 43.22395833333332860, -26.07999730980477437 ) ) ;
#28537 = CARTESIAN_POINT ( 'NONE',  ( -20.53372385742071771, 22.89100666759064495, 20.47846945139902530 ) ) ;
#28538 = CARTESIAN_POINT ( 'NONE',  ( -0.04044903255044120238, 14.42930583240935505, -30.02300923189239867 ) ) ;
#28539 = CARTESIAN_POINT ( 'NONE',  ( 27.16883889988624290, 3.925000002731188431, 19.73931689729373673 ) ) ;
#28540 = CARTESIAN_POINT ( 'NONE',  ( 21.25115026575265631, 51.99999999999997158, -25.10892607490231043 ) ) ;
#28541 = CARTESIAN_POINT ( 'NONE',  ( 33.58253175000000113, 44.22500000273117848, -10.91162601494193574 ) ) ;
#28542 = CARTESIAN_POINT ( 'NONE',  ( 18.94512977948575738, 10.42499999726881299, 13.76444248337723408 ) ) ;
#28543 = FACE_BOUND ( 'NONE', #30199, .T. ) ;
#28544 = ORIENTED_EDGE ( 'NONE', *, *, #20704, .T. ) ;
#28545 = CARTESIAN_POINT ( 'NONE',  ( -10.37757302488623701, 55.77500000273121117, 31.93888565452638417 ) ) ;
#28546 = CARTESIAN_POINT ( 'NONE',  ( -5.147494310547430452, 4.051254287009220967, -32.49999999999999289 ) ) ;
#28547 = CIRCLE ( 'NONE', #13759, 32.50000000000000000 ) ;
#28548 = CARTESIAN_POINT ( 'NONE',  ( -7.025853678916393008, 46.66704833425730925, 26.06988505166735592 ) ) ;
#28549 = CARTESIAN_POINT ( 'NONE',  ( -33.58253175000000113, 77.37500000273116996, 0.000000000000000000 ) ) ;
#28550 = VERTEX_POINT ( 'NONE', #3701 ) ;
#28551 = CARTESIAN_POINT ( 'NONE',  ( 10.37757302488624056, 24.52500000273118275, -31.93888565452638417 ) ) ;
#28552 = CARTESIAN_POINT ( 'NONE',  ( 7.505752307972854531, 12.57291666666666252, -28.01184896238303423 ) ) ;
#28553 = EDGE_CURVE ( 'NONE', #19151, #5214, #15533, .T. ) ;
#28554 = ORIENTED_EDGE ( 'NONE', *, *, #18037, .F. ) ;
#28555 = CARTESIAN_POINT ( 'NONE',  ( 5.779280353836490358E-15, 49.00000000546238255, 32.49999999999999289 ) ) ;
#28556 = CARTESIAN_POINT ( 'NONE',  ( -33.58253175000000113, 59.22500000273119269, 10.91162601494193929 ) ) ;
#28557 = CARTESIAN_POINT ( 'NONE',  ( 15.01150461594643204, 41.36197916666666430, 26.00068869287340334 ) ) ;
#28558 = ADVANCED_FACE ( 'NONE', ( #5228 ), #10380, .T. ) ;
#28559 = CARTESIAN_POINT ( 'NONE',  ( -19.82091636218621389, 17.19999999999999218, 14.40073868116558842 ) ) ;
#28560 = VECTOR ( 'NONE', #29357, 1000.000000000000000 ) ;
#28561 = CARTESIAN_POINT ( 'NONE',  ( -27.16883889988624290, 4.925000002731189319, -19.73931689729374028 ) ) ;
#28562 = CARTESIAN_POINT ( 'NONE',  ( -7.570916362186210335, 6.349999994537613546, -23.30088464923126779 ) ) ;
#28563 = CARTESIAN_POINT ( 'NONE',  ( 20.53372385742108008, 60.40586833240935505, 20.47846945139866648 ) ) ;
#28564 = CARTESIAN_POINT ( 'NONE',  ( 12.13525491562421088, 80.79999999999998295, 8.816778784387095058 ) ) ;
#28565 = CARTESIAN_POINT ( 'NONE',  ( 5.147494310547426899, 9.448745718453144704, -32.50000000000000000 ) ) ;
#28566 = CARTESIAN_POINT ( 'NONE',  ( 26.29305231718579350, 18.79999999999999716, 19.10302069950537529 ) ) ;
#28567 = CARTESIAN_POINT ( 'NONE',  ( -24.20753774853756823, 63.41927083333333570, -13.97622843553588723 ) ) ;
#28568 = CARTESIAN_POINT ( 'NONE',  ( 24.50000000000000355, 13.64999999453761781, 7.960532557706212486 ) ) ;
#28569 = CARTESIAN_POINT ( 'NONE',  ( -4.635254915624211769, 71.85000000546237686, -14.26584774442730286 ) ) ;
#28570 = CARTESIAN_POINT ( 'NONE',  ( 6.988114217768294445, 24.31770833333332504, 26.07999730980477437 ) ) ;
#28571 = CARTESIAN_POINT ( 'NONE',  ( 20.75514604977249178, 29.82500000273119767, 28.56700777964553950 ) ) ;
#28572 = CARTESIAN_POINT ( 'NONE',  ( 20.75514604977249178, 77.82500000273120122, 28.56700777964553950 ) ) ;
#28573 = AXIS2_PLACEMENT_3D ( 'NONE', #6599, #22732, #6936 ) ;
#28574 = CARTESIAN_POINT ( 'NONE',  ( 20.75514604977249178, 34.07500000273117990, 28.56700777964553950 ) ) ;
#28575 = CARTESIAN_POINT ( 'NONE',  ( 27.16883889988624290, 24.17500000273117777, 19.73931689729373673 ) ) ;
#28576 = CARTESIAN_POINT ( 'NONE',  ( -10.04305231718579172, 67.59999999999999432, -30.90933677959248982 ) ) ;
#28577 = CARTESIAN_POINT ( 'NONE',  ( 26.09010956794232428, 45.52121500092397355, -6.950374756619718042 ) ) ;
#28578 = CARTESIAN_POINT ( 'NONE',  ( -3.880418787951142701, 15.19874571299077282, 24.49999999999999645 ) ) ;
#28579 = CARTESIAN_POINT ( 'NONE',  ( 0.000000000000000000, 80.00000000000001421, 0.000000000000000000 ) ) ;
#28580 = CARTESIAN_POINT ( 'NONE',  ( -10.04305231718579172, 63.60000000000000142, -30.90933677959248982 ) ) ;
#28581 = CARTESIAN_POINT ( 'NONE',  ( 7.236395654485760609, 17.02499999726880731, -22.27133577429736633 ) ) ;
#28582 = CARTESIAN_POINT ( 'NONE',  ( -20.75514604977248112, 63.42500000273118843, 28.56700777964554661 ) ) ;
#28583 = CARTESIAN_POINT ( 'NONE',  ( 18.94512977948575738, 6.924999997268810326, 13.76444248337723408 ) ) ;
#28584 = CARTESIAN_POINT ( 'NONE',  ( 10.37757302488624767, 75.97500000273120691, 31.93888565452638417 ) ) ;
#28585 = CARTESIAN_POINT ( 'NONE',  ( -10.37757302488623701, 7.525000002731207616, 31.93888565452638417 ) ) ;
#28586 = CARTESIAN_POINT ( 'NONE',  ( 23.41746824999999887, 19.12499999726882649, 0.000000000000000000 ) ) ;
#28587 = CARTESIAN_POINT ( 'NONE',  ( 19.11951029504763611, 10.85975666759064318, -19.06425588902591173 ) ) ;
#28588 = ORIENTED_EDGE ( 'NONE', *, *, #17135, .T. ) ;
#28589 = CARTESIAN_POINT ( 'NONE',  ( 6.486482029760649416E-15, 45.62500000273118417, 35.31076352940723240 ) ) ;
#28590 = ORIENTED_EDGE ( 'NONE', *, *, #18312, .T. ) ;
#28591 = CARTESIAN_POINT ( 'NONE',  ( -2.584737979205441561E-13, 39.92968750000000000, -30.02300923189239512 ) ) ;
#28592 = FACE_OUTER_BOUND ( 'NONE', #2655, .T. ) ;
#28593 = CARTESIAN_POINT ( 'NONE',  ( 26.29305231718579350, 5.300000005462379704, 19.10302069950537529 ) ) ;
#28594 = CARTESIAN_POINT ( 'NONE',  ( 23.41746824999999887, 3.124999997268812280, 0.000000000000000000 ) ) ;
#28595 = CARTESIAN_POINT ( 'NONE',  ( -7.236395654485763274, 18.02499999726880731, 22.27133577429736633 ) ) ;
#28596 = CARTESIAN_POINT ( 'NONE',  ( -20.75514604977248823, 17.07500000273119056, -28.56700777964554305 ) ) ;
#28597 = CARTESIAN_POINT ( 'NONE',  ( -20.08610463437157989, 20.20000000546239249, -27.64615127144129758 ) ) ;
#28598 = CARTESIAN_POINT ( 'NONE',  ( 26.29305231718578995, 65.20000000000000284, -19.10302069950538240 ) ) ;
#28599 = CARTESIAN_POINT ( 'NONE',  ( 12.13525491562421088, 77.05000000546239391, 8.816778784387095058 ) ) ;
#28600 = DIRECTION ( 'NONE',  ( -0.000000000000000000, -1.000000000000000000, -0.000000000000000000 ) ) ;
#28601 = CARTESIAN_POINT ( 'NONE',  ( -30.02300923189239867, 64.57069416759065916, -0.04044903254991731589 ) ) ;
#28602 = CARTESIAN_POINT ( 'NONE',  ( 11.25946833292375793, 80.57500000273121543, -8.180482586598735395 ) ) ;
#28603 = CARTESIAN_POINT ( 'NONE',  ( 20.50609665440969565, 36.92187499999999289, -20.50609665441004736 ) ) ;
#28604 = SHAPE_DEFINITION_REPRESENTATION ( #10448, #15301 ) ;
#28605 = CARTESIAN_POINT ( 'NONE',  ( 0.000000000000000000, 16.99999999999998579, -24.50000000000000000 ) ) ;
#28606 = CARTESIAN_POINT ( 'NONE',  ( 14.47279130897151589, 18.82499999726881157, 19.92008829642072953 ) ) ;
#28607 = CARTESIAN_POINT ( 'NONE',  ( -10.04305231718579172, 5.599999999999994316, -30.90933677959248982 ) ) ;
#28608 = DIRECTION ( 'NONE',  ( -0.000000000000000000, -1.000000000000000000, -0.000000000000000000 ) ) ;
#28609 = CARTESIAN_POINT ( 'NONE',  ( 6.950374756619257965, 52.38503499907601224, -26.09010956794244507 ) ) ;
#28610 = CARTESIAN_POINT ( 'NONE',  ( 33.58253175000000823, 50.02500000273118985, 10.91162601494192863 ) ) ;
#28611 = CARTESIAN_POINT ( 'NONE',  ( 33.58253175000000823, 58.27500000273116854, 10.91162601494192863 ) ) ;
#28612 = CARTESIAN_POINT ( 'NONE',  ( 33.58253175000000823, 44.27500000273120406, 10.91162601494192685 ) ) ;
#28613 =( BOUNDED_SURFACE ( )  B_SPLINE_SURFACE ( 1, 2, ( 
 ( #6370, #872, #13933, #11681, #26962, #6540, #19252, #32607, #17012, #1543, #27473, #29692, #1375, #11850, #22329, #9106, #29869, #6198, #32774, #17185, #4131, #11352, #3961, #9437, #19587, #24559, #32441, #21993, #16678, #3463, #14606, #12019, #9268, #21830, #22488, #14103, #27134, #27304, #22165, #30035, #1033, #3629, #19752, #16848, #30200, #6702, #32276, #27643, #32939, #8942, #29528, #8769, #6031, #16510, #11513, #19420, #3795, #14268, #24725, #1200, #7212, #22834, #4641, #25238, #30717, #20099, #17695, #20441, #6870, #25584, #4471, #20622, #10140, #30370, #7041, #15290, #9966, #28322, #30892, #12540, #15120, #14945, #28155, #25750, #2064, #23011, #33115, #7387, #2234, #30545, #14773, #17871, #9617, #17524, #33466, #27984, #25411, #1889, #1713, #12366, #4811, #12709, #27814, #23180, #17351, #33643, #31064, #33294, #19924, #4298, #22662, #9794, #12191, #20270, #22428, #27075, #14209, #30479, #6642, #9375, #24830, #1649, #6808, #11459, #16786, #12125, #19364, #17287, #27413, #27750, #1484, #19855, #6309, #11958, #20033, #29976, #19692, #30309, #9048, #4238, #24502, #17121, #16621, #22104, #32384, #3569, #6482, #22597, #14041, #25170, #976, #3738, #9208, #14543, #32876, #22270, #3902, #30138, #8879, #11791, #24664, #32712, #14712, #21933, #27579, #19527, #29808, #9554, #27245, #1139, #33049, #11621, #32549, #16954, #4068, #25002, #14372, #1309, #18152, #23114, #33577 ),
 ( #10075, #17805, #1823, #25344, #20556, #4406, #17981, #30651, #31002, #28431, #2524, #4921, #7148, #12820, #23292, #33760, #7499, #7320, #17630, #10252, #28594, #20894, #15401, #12476, #12643, #22946, #5093, #20378, #25857, #27923, #15226, #4747, #2346, #14883, #20733, #31173, #6980, #9901, #7665, #12301, #17463, #25522, #22773, #15579, #25689, #33926, #28263, #26031, #33226, #2170, #12993, #28091, #9725, #23464, #4579, #10416, #20211, #15057, #30827, #2001, #33404, #19205, #1151, #24677, #21943, #29642, #6819, #27763, #1495, #16630, #17301, #16799, #32393, #29988, #14386, #24843, #27256, #19373, #22282, #19540, #6654, #11971, #24514, #30150, #1321, #11633, #22441, #11469, #27590, #22116, #4080, #29818, #8888, #6323, #11804, #6492, #16965, #27423, #8721, #3914, #27086, #3747, #14724, #32727, #30323, #6145, #9220, #32887, #14221, #3580, #25015, #14052, #9386, #984, #4249, #25185, #19704, #17137, #1662, #12137, #19870, #14554, #32231, #32560, #9059, #25701, #2182, #33239, #20390, #12656, #9913, #20046, #20745, #20569, #25358, #30842, #5106, #23306, #28104, #17474, #7678, #1836, #33590, #12489, #4761, #33416, #15238, #7333, #27935, #6992, #23125, #30491, #10091, #12314, #31013, #7511, #18164, #17995, #22786, #28441, #4932, #15414, #25869, #22958, #9737, #2359, #10263, #2537, #12832, #4591, #28274, #15067, #31188, #2014, #33772, #9568, #17817, #28606, #15590, #4419, #26042 ) ),
 .UNSPECIFIED., .F., .F., .T. ) 
 B_SPLINE_SURFACE_WITH_KNOTS ( ( 2, 2 ),
 ( 3, 2, 2, 2, 2, 2, 2, 2, 2, 2, 2, 2, 2, 2, 2, 2, 2, 2, 2, 2, 2, 2, 2, 2, 2, 2, 2, 2, 2, 2, 2, 2, 2, 2, 2, 2, 2, 2, 2, 2, 2, 2, 2, 2, 2, 2, 2, 2, 2, 2, 2, 2, 2, 2, 2, 2, 2, 2, 2, 2, 2, 2, 2, 2, 2, 2, 2, 2, 2, 2, 2, 2, 2, 2, 2, 2, 2, 2, 2, 2, 2, 2, 2, 2, 2, 2, 2, 2, 2, 2, 3 ),
 ( 0.000000000000000000, 1.000000000000000000 ),
 ( 0.000000000000000000, 0.01111111111111111154, 0.02222222222222222307, 0.03333333333333333287, 0.04444444444444444614, 0.05555555555555555247, 0.06666666666666666574, 0.07777777777777777901, 0.08888888888888889228, 0.1000000000000000056, 0.1111111111111111049, 0.1222222222222222182, 0.1333333333333333315, 0.1444444444444444309, 0.1555555555555555580, 0.1666666666666666574, 0.1777777777777777846, 0.1888888888888888840, 0.2000000000000000111, 0.2111111111111111105, 0.2222222222222222099, 0.2333333333333333370, 0.2444444444444444364, 0.2555555555555555358, 0.2666666666666666630, 0.2777777777777777901, 0.2888888888888888618, 0.2999999999999999889, 0.3111111111111111160, 0.3222222222222222432, 0.3333333333333333148, 0.3444444444444444420, 0.3555555555555555691, 0.3666666666666666408, 0.3777777777777777679, 0.3888888888888888951, 0.4000000000000000222, 0.4111111111111110938, 0.4222222222222222210, 0.4333333333333333481, 0.4444444444444444198, 0.4555555555555555469, 0.4666666666666666741, 0.4777777777777778012, 0.4888888888888888729, 0.5000000000000000000, 0.5111111111111110716, 0.5222222222222222543, 0.5333333333333333259, 0.5444444444444443976, 0.5555555555555555802, 0.5666666666666666519, 0.5777777777777777235, 0.5888888888888889062, 0.5999999999999999778, 0.6111111111111111605, 0.6222222222222222321, 0.6333333333333333037, 0.6444444444444444864, 0.6555555555555555580, 0.6666666666666666297, 0.6777777777777778123, 0.6888888888888888840, 0.6999999999999999556, 0.7111111111111111382, 0.7222222222222222099, 0.7333333333333332815, 0.7444444444444444642, 0.7555555555555555358, 0.7666666666666667185, 0.7777777777777777901, 0.7888888888888888618, 0.8000000000000000444, 0.8111111111111111160, 0.8222222222222221877, 0.8333333333333333703, 0.8444444444444444420, 0.8555555555555555136, 0.8666666666666666963, 0.8777777777777777679, 0.8888888888888888395, 0.9000000000000000222, 0.9111111111111110938, 0.9222222222222222765, 0.9333333333333333481, 0.9444444444444444198, 0.9555555555555556024, 0.9666666666666666741, 0.9777777777777777457, 0.9888888888888889284, 1.000000000000000000 ),
 .UNSPECIFIED. ) 
 GEOMETRIC_REPRESENTATION_ITEM ( )  RATIONAL_B_SPLINE_SURFACE ( (
 ( 1.000000000000000000, 0.9510565162951535312, 1.000000000000000000, 0.9510565162951535312, 1.000000000000000000, 0.9510565162951535312, 1.000000000000000000, 0.9510565162951535312, 1.000000000000000000, 0.9510565162951535312, 1.000000000000000000, 0.9510565162951535312, 1.000000000000000000, 0.9510565162951535312, 1.000000000000000000, 0.9510565162951535312, 1.000000000000000000, 0.9510565162951535312, 1.000000000000000000, 0.9510565162951535312, 1.000000000000000000, 0.9510565162951535312, 1.000000000000000000, 0.9510565162951535312, 1.000000000000000000, 0.9510565162951535312, 1.000000000000000000, 0.9510565162951535312, 1.000000000000000000, 0.9510565162951535312, 1.000000000000000000, 0.9510565162951535312, 1.000000000000000000, 0.9510565162951535312, 1.000000000000000000, 0.9510565162951535312, 1.000000000000000000, 0.9510565162951535312, 1.000000000000000000, 0.9510565162951535312, 1.000000000000000000, 0.9510565162951535312, 1.000000000000000000, 0.9510565162951535312, 1.000000000000000000, 0.9510565162951535312, 1.000000000000000000, 0.9510565162951535312, 1.000000000000000000, 0.9510565162951535312, 1.000000000000000000, 0.9510565162951535312, 1.000000000000000000, 0.9510565162951535312, 1.000000000000000000, 0.9510565162951535312, 1.000000000000000000, 0.9510565162951535312, 1.000000000000000000, 0.9510565162951535312, 1.000000000000000000, 0.9510565162951535312, 1.000000000000000000, 0.9510565162951535312, 1.000000000000000000, 0.9510565162951535312, 1.000000000000000000, 0.9510565162951535312, 1.000000000000000000, 0.9510565162951535312, 1.000000000000000000, 0.9510565162951535312, 1.000000000000000000, 0.9510565162951535312, 1.000000000000000000, 0.9510565162951535312, 1.000000000000000000, 0.9510565162951535312, 1.000000000000000000, 0.9510565162951535312, 1.000000000000000000, 0.9510565162951535312, 1.000000000000000000, 0.9510565162951535312, 1.000000000000000000, 0.9510565162951535312, 1.000000000000000000, 0.9510565162951535312, 1.000000000000000000, 0.9510565162951535312, 1.000000000000000000, 0.9510565162951535312, 1.000000000000000000, 0.9510565162951535312, 1.000000000000000000, 0.9510565162951535312, 1.000000000000000000, 0.9510565162951535312, 1.000000000000000000, 0.9510565162951535312, 1.000000000000000000, 0.9510565162951535312, 1.000000000000000000, 0.9510565162951535312, 1.000000000000000000, 0.9510565162951535312, 1.000000000000000000, 0.9510565162951535312, 1.000000000000000000, 0.9510565162951535312, 1.000000000000000000, 0.9510565162951535312, 1.000000000000000000, 0.9510565162951535312, 1.000000000000000000, 0.9510565162951535312, 1.000000000000000000, 0.9510565162951535312, 1.000000000000000000, 0.9510565162951535312, 1.000000000000000000, 0.9510565162951535312, 1.000000000000000000, 0.9510565162951535312, 1.000000000000000000, 0.9510565162951535312, 1.000000000000000000, 0.9510565162951535312, 1.000000000000000000, 0.9510565162951535312, 1.000000000000000000, 0.9510565162951535312, 1.000000000000000000, 0.9510565162951535312, 1.000000000000000000, 0.9510565162951535312, 1.000000000000000000, 0.9510565162951535312, 1.000000000000000000, 0.9510565162951535312, 1.000000000000000000, 0.9510565162951535312, 1.000000000000000000, 0.9510565162951535312, 1.000000000000000000, 0.9510565162951535312, 1.000000000000000000, 0.9510565162951535312, 1.000000000000000000, 0.9510565162951535312, 1.000000000000000000, 0.9510565162951535312, 1.000000000000000000, 0.9510565162951535312, 1.000000000000000000, 0.9510565162951535312, 1.000000000000000000, 0.9510565162951535312, 1.000000000000000000, 0.9510565162951535312, 1.000000000000000000, 0.9510565162951535312, 1.000000000000000000, 0.9510565162951535312, 1.000000000000000000, 0.9510565162951535312, 1.000000000000000000, 0.9510565162951535312, 1.000000000000000000, 0.9510565162951535312, 1.000000000000000000, 0.9510565162951535312, 1.000000000000000000, 0.9510565162951535312, 1.000000000000000000, 0.9510565162951535312, 1.000000000000000000, 0.9510565162951535312, 1.000000000000000000, 0.9510565162951535312, 1.000000000000000000),
 ( 1.000000000000000000, 0.9510565162951535312, 1.000000000000000000, 0.9510565162951535312, 1.000000000000000000, 0.9510565162951535312, 1.000000000000000000, 0.9510565162951535312, 1.000000000000000000, 0.9510565162951535312, 1.000000000000000000, 0.9510565162951535312, 1.000000000000000000, 0.9510565162951535312, 1.000000000000000000, 0.9510565162951535312, 1.000000000000000000, 0.9510565162951535312, 1.000000000000000000, 0.9510565162951535312, 1.000000000000000000, 0.9510565162951535312, 1.000000000000000000, 0.9510565162951535312, 1.000000000000000000, 0.9510565162951535312, 1.000000000000000000, 0.9510565162951535312, 1.000000000000000000, 0.9510565162951535312, 1.000000000000000000, 0.9510565162951535312, 1.000000000000000000, 0.9510565162951535312, 1.000000000000000000, 0.9510565162951535312, 1.000000000000000000, 0.9510565162951535312, 1.000000000000000000, 0.9510565162951535312, 1.000000000000000000, 0.9510565162951535312, 1.000000000000000000, 0.9510565162951535312, 1.000000000000000000, 0.9510565162951535312, 1.000000000000000000, 0.9510565162951535312, 1.000000000000000000, 0.9510565162951535312, 1.000000000000000000, 0.9510565162951535312, 1.000000000000000000, 0.9510565162951535312, 1.000000000000000000, 0.9510565162951535312, 1.000000000000000000, 0.9510565162951535312, 1.000000000000000000, 0.9510565162951535312, 1.000000000000000000, 0.9510565162951535312, 1.000000000000000000, 0.9510565162951535312, 1.000000000000000000, 0.9510565162951535312, 1.000000000000000000, 0.9510565162951535312, 1.000000000000000000, 0.9510565162951535312, 1.000000000000000000, 0.9510565162951535312, 1.000000000000000000, 0.9510565162951535312, 1.000000000000000000, 0.9510565162951535312, 1.000000000000000000, 0.9510565162951535312, 1.000000000000000000, 0.9510565162951535312, 1.000000000000000000, 0.9510565162951535312, 1.000000000000000000, 0.9510565162951535312, 1.000000000000000000, 0.9510565162951535312, 1.000000000000000000, 0.9510565162951535312, 1.000000000000000000, 0.9510565162951535312, 1.000000000000000000, 0.9510565162951535312, 1.000000000000000000, 0.9510565162951535312, 1.000000000000000000, 0.9510565162951535312, 1.000000000000000000, 0.9510565162951535312, 1.000000000000000000, 0.9510565162951535312, 1.000000000000000000, 0.9510565162951535312, 1.000000000000000000, 0.9510565162951535312, 1.000000000000000000, 0.9510565162951535312, 1.000000000000000000, 0.9510565162951535312, 1.000000000000000000, 0.9510565162951535312, 1.000000000000000000, 0.9510565162951535312, 1.000000000000000000, 0.9510565162951535312, 1.000000000000000000, 0.9510565162951535312, 1.000000000000000000, 0.9510565162951535312, 1.000000000000000000, 0.9510565162951535312, 1.000000000000000000, 0.9510565162951535312, 1.000000000000000000, 0.9510565162951535312, 1.000000000000000000, 0.9510565162951535312, 1.000000000000000000, 0.9510565162951535312, 1.000000000000000000, 0.9510565162951535312, 1.000000000000000000, 0.9510565162951535312, 1.000000000000000000, 0.9510565162951535312, 1.000000000000000000, 0.9510565162951535312, 1.000000000000000000, 0.9510565162951535312, 1.000000000000000000, 0.9510565162951535312, 1.000000000000000000, 0.9510565162951535312, 1.000000000000000000, 0.9510565162951535312, 1.000000000000000000, 0.9510565162951535312, 1.000000000000000000, 0.9510565162951535312, 1.000000000000000000, 0.9510565162951535312, 1.000000000000000000, 0.9510565162951535312, 1.000000000000000000, 0.9510565162951535312, 1.000000000000000000, 0.9510565162951535312, 1.000000000000000000, 0.9510565162951535312, 1.000000000000000000, 0.9510565162951535312, 1.000000000000000000, 0.9510565162951535312, 1.000000000000000000, 0.9510565162951535312, 1.000000000000000000, 0.9510565162951535312, 1.000000000000000000, 0.9510565162951535312, 1.000000000000000000, 0.9510565162951535312, 1.000000000000000000, 0.9510565162951535312, 1.000000000000000000, 0.9510565162951535312, 1.000000000000000000, 0.9510565162951535312, 1.000000000000000000, 0.9510565162951535312, 1.000000000000000000, 0.9510565162951535312, 1.000000000000000000) ) ) 
 REPRESENTATION_ITEM ( '' )  SURFACE ( )  );
#28614 = CARTESIAN_POINT ( 'NONE',  ( 20.08610463437158344, 23.20000000546238539, 27.64615127144129403 ) ) ;
#28615 = CARTESIAN_POINT ( 'NONE',  ( 26.07999730980477437, 13.14583333333332860, -6.988114217768290004 ) ) ;
#28616 = CARTESIAN_POINT ( 'NONE',  ( -26.29305231718578995, 62.20000000000000284, 19.10302069950538595 ) ) ;
#28617 = DIRECTION ( 'NONE',  ( -1.000000000000000000, -1.224646799147353454E-16, 0.000000000000000000 ) ) ;
#28618 =( BOUNDED_CURVE ( )  B_SPLINE_CURVE ( 2, ( #16222, #8804, #16055, #23770, #18794, #13297, #26677, #6063, #238, #26509, #16546, #29238, #8143 ),
 .UNSPECIFIED., .F., .T. ) 
 B_SPLINE_CURVE_WITH_KNOTS ( ( 3, 2, 2, 2, 2, 2, 3 ),
 ( 0.6089743589743590313, 0.6102564102564103088, 0.6128205128205128638, 0.6153846153846154188, 0.6179487179487179738, 0.6205128205128205288, 0.6217948717948718063 ),
 .UNSPECIFIED. ) 
 CURVE ( )  GEOMETRIC_REPRESENTATION_ITEM ( )  RATIONAL_B_SPLINE_CURVE ( ( 0.9755282581475768211, 0.9755282581475778203, 1.000000000000000000, 0.9510565162951535312, 1.000000000000000000, 0.9510565162951535312, 1.000000000000000000, 0.9510565162951535312, 1.000000000000000000, 0.9510565162951535312, 1.000000000000000000, 0.9755282581475768211, 0.9755282581475768211 ) ) 
 REPRESENTATION_ITEM ( '' )  );
#28619 = CARTESIAN_POINT ( 'NONE',  ( 0.000000000000000000, -22.99999999999999289, 0.000000000000000000 ) ) ;
#28620 = CARTESIAN_POINT ( 'NONE',  ( 27.16883889988624290, 15.92500000273118488, 19.73931689729373673 ) ) ;
#28621 = CARTESIAN_POINT ( 'NONE',  ( 20.08610463437157279, 7.300000000000001599, -27.64615127144129758 ) ) ;
#28622 = CARTESIAN_POINT ( 'NONE',  ( -24.50000000000000000, 12.64999999453762136, -7.960532557706207157 ) ) ;
#28623 = DIRECTION ( 'NONE',  ( 0.000000000000000000, -1.000000000000000000, 0.000000000000000000 ) ) ;
#28624 = CARTESIAN_POINT ( 'NONE',  ( 13.94119854578893580, 14.71576416574268720, -24.22776226481265383 ) ) ;
#28625 = CARTESIAN_POINT ( 'NONE',  ( 32.50000000000000000, 37.50000000546237544, -3.980102097228898626E-15 ) ) ;
#28626 = CARTESIAN_POINT ( 'NONE',  ( 15.14183272437242067, 17.44999999453764516, 20.84094480462498211 ) ) ;
#28627 = CARTESIAN_POINT ( 'NONE',  ( -27.16883889988624290, 26.92500000273118133, -19.73931689729374028 ) ) ;
#28628 = CARTESIAN_POINT ( 'NONE',  ( 24.20753774853731244, 43.94010416666665719, -13.97622843553632599 ) ) ;
#28629 = ORIENTED_EDGE ( 'NONE', *, *, #19434, .T. ) ;
#28630 = CARTESIAN_POINT ( 'NONE',  ( 27.16883889988624290, 63.92500000273120264, 19.73931689729373673 ) ) ;
#28631 = CARTESIAN_POINT ( 'NONE',  ( -26.00068869287340334, 45.65885416666666430, 15.01150461594643382 ) ) ;
#28632 = ORIENTED_EDGE ( 'NONE', *, *, #16303, .T. ) ;
#28633 = CARTESIAN_POINT ( 'NONE',  ( 15.01150461594643204, 13.86197916666666430, 26.00068869287340334 ) ) ;
#28634 = CARTESIAN_POINT ( 'NONE',  ( 0.04044903254992426173, 17.30506916759064140, -30.02300923189239867 ) ) ;
#28635 = VECTOR ( 'NONE', #25198, 1000.000000000000000 ) ;
#28636 = VERTEX_POINT ( 'NONE', #22738 ) ;
#28637 = CARTESIAN_POINT ( 'NONE',  ( 10.37757302488624056, 4.525000002731191628, -31.93888565452638417 ) ) ;
#28638 = VECTOR ( 'NONE', #15188, 1000.000000000000000 ) ;
#28639 = CARTESIAN_POINT ( 'NONE',  ( -4.523095164977116484E-15, 2.124999997268812280, 24.62258325217400312 ) ) ;
#28640 = CARTESIAN_POINT ( 'NONE',  ( -33.58253175000000113, 35.37500000273119127, 0.000000000000000000 ) ) ;
#28641 = CARTESIAN_POINT ( 'NONE',  ( 20.08610463437158344, 37.20000000546237118, 27.64615127144129403 ) ) ;
#28642 = CARTESIAN_POINT ( 'NONE',  ( 9.270509831248425314, 74.69999999999994600, 12.75976212528059683 ) ) ;
#28643 = CARTESIAN_POINT ( 'NONE',  ( 27.16883889988624290, 25.92500000273118133, 19.73931689729373673 ) ) ;
#28644 = CARTESIAN_POINT ( 'NONE',  ( 15.14183272437242422, 6.049999994537626158, -20.84094480462497856 ) ) ;
#28645 = CARTESIAN_POINT ( 'NONE',  ( -33.58253175000000113, 51.37500000273120548, 0.000000000000000000 ) ) ;
#28646 = SURFACE_STYLE_FILL_AREA ( #10972 ) ;
#28647 = EDGE_CURVE ( 'NONE', #15956, #5936, #17766, .T. ) ;
#28648 = CARTESIAN_POINT ( 'NONE',  ( 32.50000000000000711, 30.89999999999998437, 10.55989012756945122 ) ) ;
#28649 = CARTESIAN_POINT ( 'NONE',  ( 20.08610463437158344, 28.69999999999999574, 27.64615127144129403 ) ) ;
#28650 = CARTESIAN_POINT ( 'NONE',  ( 15.14183272437242245, 8.300000000000000711, -20.84094480462497856 ) ) ;
#28651 = CARTESIAN_POINT ( 'NONE',  ( 33.58253175000000113, 70.22500000273120691, -10.91162601494193751 ) ) ;
#28652 = CARTESIAN_POINT ( 'NONE',  ( -33.36402495954516922, 67.00000000000002842, 0.4025740098929149191 ) ) ;
#28653 = CARTESIAN_POINT ( 'NONE',  ( -20.08610463437156923, 20.80000000546236905, 27.64615127144130113 ) ) ;
#28654 = CARTESIAN_POINT ( 'NONE',  ( 20.75514604977249178, 62.07500000273119412, 28.56700777964553950 ) ) ;
#28655 = EDGE_CURVE ( 'NONE', #15993, #23029, #12610, .T. ) ;
#28656 = EDGE_CURVE ( 'NONE', #871, #220, #33540, .T. ) ;
#28657 = CARTESIAN_POINT ( 'NONE',  ( -5.147494310547430452, 40.05125428700921475, -32.49999999999999289 ) ) ;
#28658 = CARTESIAN_POINT ( 'NONE',  ( 10.37757302488624056, 14.52500000273118630, -31.93888565452638417 ) ) ;
#28659 = CARTESIAN_POINT ( 'NONE',  ( -7.025853678916393008, 29.47954833425730570, 26.06988505166735592 ) ) ;
#28660 = CARTESIAN_POINT ( 'NONE',  ( -2.376701315729135899, 67.00000000000000000, -33.34874525913694754 ) ) ;
#28661 = CONICAL_SURFACE ( 'NONE', #1797, 12.11000150615021909, 0.2617993877991545149 ) ;
#28662 = CARTESIAN_POINT ( 'NONE',  ( 10.37757302488624767, 1.975000002731180926, 31.93888565452638417 ) ) ;
#28663 = CARTESIAN_POINT ( 'NONE',  ( -20.75514604977248112, 35.42500000273119554, 28.56700777964554661 ) ) ;
#28664 = CARTESIAN_POINT ( 'NONE',  ( 26.29305231718579350, 45.30000000546238681, 19.10302069950537529 ) ) ;
#28665 = DIRECTION ( 'NONE',  ( 0.000000000000000000, -1.000000000000000000, 0.000000000000000000 ) ) ;
#28666 = VECTOR ( 'NONE', #182, 1000.000000000000000 ) ;
#28667 = EDGE_CURVE ( 'NONE', #27108, #25557, #4970, .T. ) ;
#28668 = CARTESIAN_POINT ( 'NONE',  ( 2.688165632520823219E-15, 77.37500000273116996, 14.63369212191046209 ) ) ;
#28669 = CARTESIAN_POINT ( 'NONE',  ( 20.47846945139867003, 42.35899333240935505, -20.53372385742107653 ) ) ;
#28670 = CARTESIAN_POINT ( 'NONE',  ( 10.04305231718579705, 55.10000000546237686, 30.90933677959248982 ) ) ;
#28671 = CARTESIAN_POINT ( 'NONE',  ( -13.91746824999999532, 79.47500000273115006, 4.522059556121122093 ) ) ;
#28672 = CARTESIAN_POINT ( 'NONE',  ( -2.428612866367529427E-13, 19.30468749999999645, -27.95245687107222921 ) ) ;
#28673 = LINE ( 'NONE', #12722, #32395 ) ;
#28674 = CARTESIAN_POINT ( 'NONE',  ( -20.08610463437156923, 70.80000000546235128, 27.64615127144130113 ) ) ;
#28675 = CARTESIAN_POINT ( 'NONE',  ( 20.50609665440969565, 23.17187499999999289, -20.50609665441004736 ) ) ;
#28676 = CARTESIAN_POINT ( 'NONE',  ( 20.75514604977249178, 34.07500000273117990, 28.56700777964553950 ) ) ;
#28677 = CARTESIAN_POINT ( 'NONE',  ( 23.41746824999999887, 7.024999997268802865, 7.608796670333735079 ) ) ;
#28678 = ORIENTED_EDGE ( 'NONE', *, *, #3707, .F. ) ;
#28679 = CARTESIAN_POINT ( 'NONE',  ( -26.02091320914849959, 43.65923583425730925, 14.97647472619947528 ) ) ;
#28680 = CARTESIAN_POINT ( 'NONE',  ( -32.50000000000000000, 20.60000000546237686, 10.55989012756946366 ) ) ;
#28681 = CARTESIAN_POINT ( 'NONE',  ( -20.50609665440969209, 45.51562500000000000, 20.50609665441005092 ) ) ;
#28682 = CARTESIAN_POINT ( 'NONE',  ( -28.01184896238290278, 62.98958333333332149, 7.505752307973363457 ) ) ;
#28683 = CARTESIAN_POINT ( 'NONE',  ( -20.75514604977248112, 55.67500000273118843, 28.56700777964554661 ) ) ;
#28684 = CARTESIAN_POINT ( 'NONE',  ( 26.29305231718579350, 55.30000000546236549, 19.10302069950537529 ) ) ;
#28685 = CARTESIAN_POINT ( 'NONE',  ( -4.223320258572819786E-15, 5.249999994537629888, 24.50000000000000000 ) ) ;
#28686 = CARTESIAN_POINT ( 'NONE',  ( -20.75514604977248112, 41.42500000273118133, 28.56700777964554661 ) ) ;
#28687 = DIRECTION ( 'NONE',  ( -0.000000000000000000, -1.000000000000000000, -0.000000000000000000 ) ) ;
#28688 = CARTESIAN_POINT ( 'NONE',  ( -27.16883889988624290, 71.17500000273119554, -19.73931689729374028 ) ) ;
#28689 = CARTESIAN_POINT ( 'NONE',  ( 10.11000150615022619, -45.00000000000000000, 1.238118098388178925E-15 ) ) ;
#28690 = CIRCLE ( 'NONE', #2383, 15.31642273298461276 ) ;
#28691 = CARTESIAN_POINT ( 'NONE',  ( -33.58253175000000113, 63.22500000273119269, 10.91162601494193929 ) ) ;
#28692 = CARTESIAN_POINT ( 'NONE',  ( 7.505752307972854531, 19.44791666666666075, -28.01184896238303423 ) ) ;
#28693 = CARTESIAN_POINT ( 'NONE',  ( -26.29305231718578995, 46.19999999999998863, 19.10302069950538595 ) ) ;
#28694 = CARTESIAN_POINT ( 'NONE',  ( -23.41746825000000598, 3.724999997268819918, 7.608796670333726198 ) ) ;
#28695 = CARTESIAN_POINT ( 'NONE',  ( -10.37757302488624411, 10.97500000273118914, -31.93888565452638417 ) ) ;
#28696 = CARTESIAN_POINT ( 'NONE',  ( 5.147494310547434893, 35.05125428700922896, 32.49999999999999289 ) ) ;
#28697 = CARTESIAN_POINT ( 'NONE',  ( 24.22776226481265383, 36.20013916574269075, 13.94119854578893580 ) ) ;
#28698 = CARTESIAN_POINT ( 'NONE',  ( 13.91746825000000065, 80.27500000273117564, 4.522059556121114987 ) ) ;
#28699 = CARTESIAN_POINT ( 'NONE',  ( 33.58253175000000823, 78.27500000273117564, 10.91162601494192685 ) ) ;
#28700 = FACE_BOUND ( 'NONE', #1093, .T. ) ;
#28701 = CARTESIAN_POINT ( 'NONE',  ( 33.58253175000000113, 76.37500000273118417, -4.112674001490185761E-15 ) ) ;
#28702 = VERTEX_POINT ( 'NONE', #23387 ) ;
#28703 = CARTESIAN_POINT ( 'NONE',  ( -18.94512977948576093, 12.32499999726879913, 13.76444248337722698 ) ) ;
#28704 = CARTESIAN_POINT ( 'NONE',  ( 6.988114217768294445, 55.25520833333333570, 26.07999730980477437 ) ) ;
#28705 = CARTESIAN_POINT ( 'NONE',  ( 33.58253175000000113, 52.22500000273117848, -10.91162601494193751 ) ) ;
#28706 = CARTESIAN_POINT ( 'NONE',  ( 27.16883889988624290, 16.17500000273118488, 19.73931689729373673 ) ) ;
#28707 = CARTESIAN_POINT ( 'NONE',  ( -27.16883889988624290, 78.92500000273118133, -19.73931689729374028 ) ) ;
#28708 = CARTESIAN_POINT ( 'NONE',  ( -2.428612866367529427E-13, 39.92968750000000000, -27.95245687107223276 ) ) ;
#28709 = CARTESIAN_POINT ( 'NONE',  ( 28.00173670424549499, 28.62017333425730925, 7.543491769121417612 ) ) ;
#28710 = CARTESIAN_POINT ( 'NONE',  ( 28.00173670424535644, 15.14545166574268897, -7.543491769121920321 ) ) ;
#28711 = CARTESIAN_POINT ( 'NONE',  ( 26.29305231718579350, 73.30000000546236549, 19.10302069950537529 ) ) ;
#28712 = EDGE_CURVE ( 'NONE', #4197, #12209, #9650, .T. ) ;
#28713 = DIRECTION ( 'NONE',  ( 0.000000000000000000, 0.000000000000000000, -1.000000000000000000 ) ) ;
#28714 = CIRCLE ( 'NONE', #25974, 0.9999999999999988898 ) ;
#28715 = CARTESIAN_POINT ( 'NONE',  ( -20.75514604977248112, 41.42500000273118133, 28.56700777964554661 ) ) ;
#28716 = CARTESIAN_POINT ( 'NONE',  ( -4.523095164977116484E-15, 10.12499999726881938, 24.62258325217400312 ) ) ;
#28717 = CARTESIAN_POINT ( 'NONE',  ( -26.29305231718579350, 2.300000005462377040, -19.10302069950537884 ) ) ;
#28718 = VERTEX_POINT ( 'NONE', #12742 ) ;
#28719 = CARTESIAN_POINT ( 'NONE',  ( -2.162160676586881955E-15, 56.87500000273117706, -35.31076352940723240 ) ) ;
#28720 =( BOUNDED_CURVE ( )  B_SPLINE_CURVE ( 2, ( #24595, #23646, #5277, #15761, #26214, #108, #10599, #21077, #31525, #8019, #1578, #25101, #14303 ),
 .UNSPECIFIED., .F., .F. ) 
 B_SPLINE_CURVE_WITH_KNOTS ( ( 3, 2, 2, 2, 2, 2, 3 ),
 ( 0.6944444444444444198, 0.6999999999999999556, 0.7111111111111111382, 0.7222222222222222099, 0.7333333333333332815, 0.7444444444444444642, 0.7500000000000000000 ),
 .UNSPECIFIED. ) 
 CURVE ( )  GEOMETRIC_REPRESENTATION_ITEM ( )  RATIONAL_B_SPLINE_CURVE ( ( 0.9755282581475768211, 0.9755282581475768211, 1.000000000000000000, 0.9510565162951535312, 1.000000000000000000, 0.9510565162951535312, 1.000000000000000000, 0.9510565162951535312, 1.000000000000000000, 0.9510565162951535312, 1.000000000000000000, 0.9755282581475768211, 0.9755282581475768211 ) ) 
 REPRESENTATION_ITEM ( '' )  );
#28721 = CARTESIAN_POINT ( 'NONE',  ( 3.980102097228898626E-15, 80.00000000000001421, 32.50000000000000000 ) ) ;
#28722 = CARTESIAN_POINT ( 'NONE',  ( -0.04044903254992426173, 39.64881916759063074, 27.95245687107223276 ) ) ;
#28723 = CARTESIAN_POINT ( 'NONE',  ( -10.37757302488624411, 76.97500000273119269, -31.93888565452638417 ) ) ;
#28724 = ORIENTED_EDGE ( 'NONE', *, *, #15463, .T. ) ;
#28725 = CARTESIAN_POINT ( 'NONE',  ( 10.37757302488624056, 26.52500000273118275, -31.93888565452638417 ) ) ;
#28726 = CARTESIAN_POINT ( 'NONE',  ( 28.01184896238304134, 16.86979166666666075, 7.505752307972846538 ) ) ;
#28727 = ORIENTED_EDGE ( 'NONE', *, *, #2396, .T. ) ;
#28728 = CARTESIAN_POINT ( 'NONE',  ( -20.08610463437156923, 14.80000000546238503, 27.64615127144130113 ) ) ;
#28729 = CARTESIAN_POINT ( 'NONE',  ( 10.37757302488624767, 59.72500000273117848, 31.93888565452638417 ) ) ;
#28730 = CARTESIAN_POINT ( 'NONE',  ( -7.505752307972844761, 45.22916666666665719, 28.01184896238304134 ) ) ;
#28731 = CARTESIAN_POINT ( 'NONE',  ( -15.14183272437241889, 16.69999999999999574, -20.84094480462497856 ) ) ;
#28732 = CARTESIAN_POINT ( 'NONE',  ( 23.41746824999999887, 3.024999997268813079, 7.608796670333735079 ) ) ;
#28733 = CARTESIAN_POINT ( 'NONE',  ( -33.58253175000000113, 3.025000002731199622, -10.91162601494193218 ) ) ;
#28734 = CARTESIAN_POINT ( 'NONE',  ( -20.08610463437157989, 63.69999999999999574, -27.64615127144129758 ) ) ;
#28735 = CARTESIAN_POINT ( 'NONE',  ( -15.04653450569338524, 58.83034749907602645, -25.98046417659831775 ) ) ;
#28736 = CARTESIAN_POINT ( 'NONE',  ( -3.880418787951136483, 14.55125428154684997, -24.50000000000000000 ) ) ;
#28737 = CARTESIAN_POINT ( 'NONE',  ( -4.223320258572821363E-15, 80.50000000000001421, 15.00000000000000355 ) ) ;
#28738 = CARTESIAN_POINT ( 'NONE',  ( 20.08610463437158344, 75.20000000546239960, 27.64615127144129403 ) ) ;
#28739 = CARTESIAN_POINT ( 'NONE',  ( -32.50000000000000000, 16.10000000000001563, 10.55989012756946366 ) ) ;
#28740 = CARTESIAN_POINT ( 'NONE',  ( -2.428612866367529427E-13, 60.55468749999998579, -27.95245687107223276 ) ) ;
#28741 = CARTESIAN_POINT ( 'NONE',  ( 24.50000000000000355, 9.849999994537622428, -7.960532557706203605 ) ) ;
#28742 = CARTESIAN_POINT ( 'NONE',  ( 12.13525491562421088, 71.05000000546237970, 8.816778784387095058 ) ) ;
#28743 = CARTESIAN_POINT ( 'NONE',  ( -19.09188309203694445, 32.62500000000000000, -19.09188309203661049 ) ) ;
#28744 = CARTESIAN_POINT ( 'NONE',  ( -2.162160676586881955E-15, 30.62500000273119838, -35.31076352940723240 ) ) ;
#28745 = CARTESIAN_POINT ( 'NONE',  ( 27.16883889988623935, 70.32500000273118701, -19.73931689729374384 ) ) ;
#28746 = CARTESIAN_POINT ( 'NONE',  ( -33.58253175000000113, 33.47500000273119269, 10.91162601494193929 ) ) ;
#28747 = CARTESIAN_POINT ( 'NONE',  ( -27.16883889988623935, 13.57500000273120833, 19.73931689729374739 ) ) ;
#28748 = CARTESIAN_POINT ( 'NONE',  ( -15.00000000000000000, 80.00000000000001421, 0.000000000000000000 ) ) ;
#28749 = CARTESIAN_POINT ( 'NONE',  ( -19.06425588902591173, 51.25038166759065206, -19.11951029504763611 ) ) ;
#28750 = CARTESIAN_POINT ( 'NONE',  ( -33.58253175000000113, 73.12500000273119838, 0.000000000000000000 ) ) ;
#28751 = CARTESIAN_POINT ( 'NONE',  ( -26.29305231718579350, 26.30000000546236905, -19.10302069950537884 ) ) ;
#28752 = ADVANCED_FACE ( 'NONE', ( #15325 ), #17555, .T. ) ;
#28753 = CARTESIAN_POINT ( 'NONE',  ( -20.08610463437157989, 57.70000000000000284, -27.64615127144129758 ) ) ;
#28754 = DIRECTION ( 'NONE',  ( 0.8660254037844399289, -0.4999999999999977240, 0.000000000000000000 ) ) ;
#28755 = CARTESIAN_POINT ( 'NONE',  ( -20.75514604977248112, 65.42500000273116711, 28.56700777964554661 ) ) ;
#28756 = ADVANCED_FACE ( 'NONE', ( #15151 ), #17904, .T. ) ;
#28757 = CARTESIAN_POINT ( 'NONE',  ( -23.41746825000000243, 8.024999997268801977, -7.608796670333730638 ) ) ;
#28758 = STYLED_ITEM ( 'NONE', ( #22761 ), #33133 ) ;
#28759 = CARTESIAN_POINT ( 'NONE',  ( 33.58253175000000823, 72.27500000273118985, 10.91162601494192863 ) ) ;
#28760 = CARTESIAN_POINT ( 'NONE',  ( 20.75514604977248467, 6.425000002731179549, -28.56700777964554305 ) ) ;
#28761 = CARTESIAN_POINT ( 'NONE',  ( 7.236395654485755280, 2.224999997268800378, 22.27133577429736988 ) ) ;
#28762 = CARTESIAN_POINT ( 'NONE',  ( -26.06988505166735237, 13.15142333425730925, -7.025853678916388567 ) ) ;
#28763 = VERTEX_POINT ( 'NONE', #2269 ) ;
#28764 = CARTESIAN_POINT ( 'NONE',  ( -10.37757302488623701, 41.52500000273119696, 31.93888565452638417 ) ) ;
#28765 = ORIENTED_EDGE ( 'NONE', *, *, #32489, .T. ) ;
#28766 = CARTESIAN_POINT ( 'NONE',  ( -20.50609665440969209, 45.51562500000000000, 20.50609665441005092 ) ) ;
#28767 = CARTESIAN_POINT ( 'NONE',  ( 0.000000000000000000, 102.0000000000000284, -12.00000000000000178 ) ) ;
#28768 = CARTESIAN_POINT ( 'NONE',  ( 20.08610463437158344, 7.200000005462378283, 27.64615127144129403 ) ) ;
#28769 = CARTESIAN_POINT ( 'NONE',  ( 20.75514604977249178, 77.82500000273120122, 28.56700777964553950 ) ) ;
#28770 = CARTESIAN_POINT ( 'NONE',  ( -2.584737979205441561E-13, 19.30468749999999645, -30.02300923189239512 ) ) ;
#28771 = CARTESIAN_POINT ( 'NONE',  ( 24.50000000000000355, 1.899999999999998135, 7.960532557706212486 ) ) ;
#28772 = CARTESIAN_POINT ( 'NONE',  ( -2.162160676586881955E-15, 12.87500000273117884, -35.31076352940723240 ) ) ;
#28773 = CARTESIAN_POINT ( 'NONE',  ( 20.08610463437157279, 59.30000000000001847, -27.64615127144129758 ) ) ;
#28774 = CARTESIAN_POINT ( 'NONE',  ( 5.147494310547426899, 57.94874572391552192, -32.50000000000000000 ) ) ;
#28775 = CARTESIAN_POINT ( 'NONE',  ( 5.779280353836490358E-15, 50.50000000000000000, 32.49999999999999289 ) ) ;
#28776 = CARTESIAN_POINT ( 'NONE',  ( -28.00173670424535644, 37.48920166574269075, 7.543491769121936308 ) ) ;
#28777 = CARTESIAN_POINT ( 'NONE',  ( -13.91746824999999532, 73.27500000273118985, -4.522059556121115875 ) ) ;
#28778 = CARTESIAN_POINT ( 'NONE',  ( 7.505752307972854531, 43.51041666666666430, -28.01184896238303423 ) ) ;
#28779 = CONTEXT_DEPENDENT_SHAPE_REPRESENTATION ( #28948, #1888 ) ;
#28780 = DIRECTION ( 'NONE',  ( -0.000000000000000000, -1.000000000000000000, -0.000000000000000000 ) ) ;
#28781 = CARTESIAN_POINT ( 'NONE',  ( -33.58253175000000113, 79.27500000273118985, -10.91162601494193218 ) ) ;
#28782 = CARTESIAN_POINT ( 'NONE',  ( 20.08610463437158344, 17.20000000546236762, 27.64615127144129403 ) ) ;
#28783 = CARTESIAN_POINT ( 'NONE',  ( 6.950374756619257965, 66.13503499907601224, -26.09010956794244507 ) ) ;
#28784 = CARTESIAN_POINT ( 'NONE',  ( -2.162160676586881955E-15, 48.62500000273118417, -35.31076352940723240 ) ) ;
#28785 = CARTESIAN_POINT ( 'NONE',  ( -10.37757302488623701, 53.77500000273120406, 31.93888565452638417 ) ) ;
#28786 = CARTESIAN_POINT ( 'NONE',  ( -33.58253175000000113, 33.47500000273119269, 10.91162601494193929 ) ) ;
#28787 = CARTESIAN_POINT ( 'NONE',  ( 5.147494310547434893, 23.05125428700921830, 32.49999999999999289 ) ) ;
#28788 = CARTESIAN_POINT ( 'NONE',  ( 13.97622843553633842, 13.86197916666666252, 24.20753774853730889 ) ) ;
#28789 = DIRECTION ( 'NONE',  ( 0.000000000000000000, 0.000000000000000000, 1.000000000000000000 ) ) ;
#28790 = CARTESIAN_POINT ( 'NONE',  ( -10.04305231718579172, 22.10000000546236265, -30.90933677959248982 ) ) ;
#28791 = CARTESIAN_POINT ( 'NONE',  ( -10.04305231718579172, 79.59999999999999432, -30.90933677959248982 ) ) ;
#28792 = CARTESIAN_POINT ( 'NONE',  ( -20.75514604977248823, 14.82500000273117635, -28.56700777964554305 ) ) ;
#28793 = CARTESIAN_POINT ( 'NONE',  ( 32.50000000000000000, 7.000000000000006217, -3.980102097228898626E-15 ) ) ;
#28794 = LINE ( 'NONE', #25881, #19388 ) ;
#28795 = LINE ( 'NONE', #33787, #21520 ) ;
#28796 = CARTESIAN_POINT ( 'NONE',  ( -19.06425588902558133, 16.57774333240934794, 19.11951029504797006 ) ) ;
#28797 = ADVANCED_FACE ( 'NONE', ( #28519 ), #7071, .T. ) ;
#28798 = CARTESIAN_POINT ( 'NONE',  ( -10.04305231718579172, 36.10000000546239107, -30.90933677959248982 ) ) ;
#28799 = EDGE_CURVE ( 'NONE', #21772, #32341, #26021, .T. ) ;
#28800 = CARTESIAN_POINT ( 'NONE',  ( 10.04305231718579705, 10.59999999999999787, 30.90933677959248982 ) ) ;
#28801 = CARTESIAN_POINT ( 'NONE',  ( -27.16883889988624290, 24.92500000273117777, -19.73931689729374028 ) ) ;
#28802 = CARTESIAN_POINT ( 'NONE',  ( -13.97622843553632421, 46.51822916666666430, -24.20753774853731599 ) ) ;
#28803 = ORIENTED_EDGE ( 'NONE', *, *, #22998, .T. ) ;
#28804 = CARTESIAN_POINT ( 'NONE',  ( -33.58253175000000113, 61.12500000273117706, 0.000000000000000000 ) ) ;
#28805 = AXIS2_PLACEMENT_3D ( 'NONE', #14362, #9541, #32865 ) ;
#28806 = VERTEX_POINT ( 'NONE', #23263 ) ;
#28807 = CARTESIAN_POINT ( 'NONE',  ( -26.00068869287368756, 18.73177083333332149, -15.01150461594595775 ) ) ;
#28808 = CARTESIAN_POINT ( 'NONE',  ( 7.468012846824777284, 12.00559000092397532, 28.02196122052045268 ) ) ;
#28809 = CARTESIAN_POINT ( 'NONE',  ( 33.58253175000000113, 6.125000002731181503, -4.112674001490185761E-15 ) ) ;
#28810 = FACE_OUTER_BOUND ( 'NONE', #27919, .T. ) ;
#28811 = CARTESIAN_POINT ( 'NONE',  ( -33.58253175000000113, 37.47500000273118559, 10.91162601494193929 ) ) ;
#28812 = CARTESIAN_POINT ( 'NONE',  ( -20.08610463437157989, 36.20000000546237828, -27.64615127144129758 ) ) ;
#28813 = CIRCLE ( 'NONE', #7998, 30.91025403784432868 ) ;
#28814 = CARTESIAN_POINT ( 'NONE',  ( 9.270509831248425314, 72.70000000000004547, 12.75976212528059683 ) ) ;
#28815 = CARTESIAN_POINT ( 'NONE',  ( 15.31642273298461632, -59.03347138510255832, 1.875720807433735970E-15 ) ) ;
#28816 = CARTESIAN_POINT ( 'NONE',  ( -10.37757302488624411, 20.72500000273119625, -31.93888565452638417 ) ) ;
#28817 = CARTESIAN_POINT ( 'NONE',  ( 2.067204126564591252E-14, 6.249999994537623671, -24.50000000000000000 ) ) ;
#28818 = CARTESIAN_POINT ( 'NONE',  ( 27.16883889988623935, 48.57500000273118701, -19.73931689729374384 ) ) ;
#28819 = CARTESIAN_POINT ( 'NONE',  ( -10.04305231718579172, 21.59999999999999432, -30.90933677959248982 ) ) ;
#28820 = CARTESIAN_POINT ( 'NONE',  ( -32.50000000000000000, 26.09999999999999076, 10.55989012756946366 ) ) ;
#28821 = CARTESIAN_POINT ( 'NONE',  ( 7.570916362186213000, 4.399999999999987033, -23.30088464923126423 ) ) ;
#28822 = CARTESIAN_POINT ( 'NONE',  ( -2.162160676586881955E-15, 70.62500000273118417, -35.31076352940723240 ) ) ;
#28823 = CARTESIAN_POINT ( 'NONE',  ( -24.23786831611838011, 66.99999999999998579, 22.37122307655967290 ) ) ;
#28824 = CARTESIAN_POINT ( 'NONE',  ( -5.147494310547430452, 37.55125428154684641, -32.49999999999999289 ) ) ;
#28825 = CARTESIAN_POINT ( 'NONE',  ( -33.58253175000000113, 57.27500000273120406, -10.91162601494193041 ) ) ;
#28826 = CARTESIAN_POINT ( 'NONE',  ( -1.778240108872766143E-15, 8.000000005462370112, -32.49999999999999289 ) ) ;
#28827 = CARTESIAN_POINT ( 'NONE',  ( 33.58253175000000113, 12.22500000273120158, -10.91162601494193751 ) ) ;
#28828 = CARTESIAN_POINT ( 'NONE',  ( 24.22776226481241224, 28.19048583425731636, -13.94119854578936923 ) ) ;
#28829 = CARTESIAN_POINT ( 'NONE',  ( 7.570916362186213000, 10.14999999453763913, -23.30088464923126423 ) ) ;
#28830 = CARTESIAN_POINT ( 'NONE',  ( -33.58253175000000113, 1.375000002731191495, 0.000000000000000000 ) ) ;
#28831 = CARTESIAN_POINT ( 'NONE',  ( 20.75514604977249178, 35.82500000273117990, 28.56700777964553950 ) ) ;
#28832 = CARTESIAN_POINT ( 'NONE',  ( 0.000000000000000000, -22.99999999999999289, -26.50000000000000355 ) ) ;
#28833 = CARTESIAN_POINT ( 'NONE',  ( 3.000384657911015469E-15, 16.99999999999998579, 24.50000000000000000 ) ) ;
#28834 = CARTESIAN_POINT ( 'NONE',  ( -8.601468415847515203, 77.17500000273118133, 11.83890561707634959 ) ) ;
#28835 = CARTESIAN_POINT ( 'NONE',  ( -30.02300923189239867, 44.50743083240935505, 0.04044903255044988294 ) ) ;
#28836 = CARTESIAN_POINT ( 'NONE',  ( -26.29305231718579350, 54.30000000546237970, -19.10302069950537884 ) ) ;
#28837 = CARTESIAN_POINT ( 'NONE',  ( 11.25946833292375793, 78.57500000273121543, -8.180482586598735395 ) ) ;
#28838 = AXIS2_PLACEMENT_3D ( 'NONE', #21496, #16019, #16187 ) ;
#28839 = CARTESIAN_POINT ( 'NONE',  ( -19.09188309203660694, 21.45312499999999645, 19.09188309203694800 ) ) ;
#28840 = CARTESIAN_POINT ( 'NONE',  ( -32.50000000000000000, 53.99999999999999289, 0.000000000000000000 ) ) ;
#28841 = CARTESIAN_POINT ( 'NONE',  ( 32.50000000000000000, 69.60000000546236265, -10.55989012756945833 ) ) ;
#28842 = CARTESIAN_POINT ( 'NONE',  ( -15.01150461594595775, 24.74739583333332504, 26.00068869287368756 ) ) ;
#28843 = CARTESIAN_POINT ( 'NONE',  ( -33.58253175000000113, 25.37500000273119838, 0.000000000000000000 ) ) ;
#28844 = CARTESIAN_POINT ( 'NONE',  ( -18.94512977948575738, 11.92499999726881477, -13.76444248337723231 ) ) ;
#28845 = VERTEX_POINT ( 'NONE', #20863 ) ;
#28846 = CARTESIAN_POINT ( 'NONE',  ( -7.468012846824771955, 44.66184000092397355, -28.02196122052045624 ) ) ;
#28847 = CARTESIAN_POINT ( 'NONE',  ( -20.08610463437156923, 16.80000000546237970, 27.64615127144130113 ) ) ;
#28848 = CARTESIAN_POINT ( 'NONE',  ( -15.01150461594595775, 48.80989583333332860, 26.00068869287368756 ) ) ;
#28849 = CARTESIAN_POINT ( 'NONE',  ( 12.90513655866702081, 52.00000000000000711, 31.00393344628893288 ) ) ;
#28850 = CARTESIAN_POINT ( 'NONE',  ( -27.16883889988623935, 55.57500000273118701, 19.73931689729374739 ) ) ;
#28851 = CARTESIAN_POINT ( 'NONE',  ( 20.08610463437157279, 57.80000000546236549, -27.64615127144129758 ) ) ;
#28852 = CARTESIAN_POINT ( 'NONE',  ( 0.000000000000000000, -12.99999999999999822, 30.00000000000000000 ) ) ;
#28853 = AXIS2_PLACEMENT_3D ( 'NONE', #28241, #20013, #19835 ) ;
#28854 = CARTESIAN_POINT ( 'NONE',  ( 20.75514604977248467, 40.42500000273117422, -28.56700777964554305 ) ) ;
#28855 = CARTESIAN_POINT ( 'NONE',  ( 32.50000000000000000, 54.99999999999999289, -3.980102097228898626E-15 ) ) ;
#28856 = CARTESIAN_POINT ( 'NONE',  ( 27.16883889988623935, 70.57500000273120122, -19.73931689729374384 ) ) ;
#28857 = CARTESIAN_POINT ( 'NONE',  ( -20.08610463437157989, 2.200000005462375618, -27.64615127144129758 ) ) ;
#28858 = EDGE_CURVE ( 'NONE', #5592, #8282, #19017, .T. ) ;
#28859 = CARTESIAN_POINT ( 'NONE',  ( 20.75514604977249178, 61.82500000273117280, 28.56700777964553950 ) ) ;
#28860 = CARTESIAN_POINT ( 'NONE',  ( 26.00068869287367690, 17.01302083333332504, 15.01150461594596486 ) ) ;
#28861 = CARTESIAN_POINT ( 'NONE',  ( -20.08610463437156923, 48.30000000000001847, 27.64615127144130113 ) ) ;
#28862 = CARTESIAN_POINT ( 'NONE',  ( -4.523095164977116484E-15, 2.124999997268812280, 24.62258325217400312 ) ) ;
#28863 = CARTESIAN_POINT ( 'NONE',  ( -33.58253175000000113, 13.27500000273119518, -10.91162601494193218 ) ) ;
#28864 = CARTESIAN_POINT ( 'NONE',  ( 3.980102097228898626E-15, 52.00000000000000711, -32.50000000000000000 ) ) ;
#28865 = CARTESIAN_POINT ( 'NONE',  ( -0.04044903255042732459, 31.61680583240936215, -27.95245687107223986 ) ) ;
#28866 = CARTESIAN_POINT ( 'NONE',  ( -1.714505518806294835E-15, 102.0000000000000284, -14.00000000000000178 ) ) ;
#28867 = CARTESIAN_POINT ( 'NONE',  ( 20.75514604977248467, 78.67500000273116711, -28.56700777964554305 ) ) ;
#28868 = PLANE ( 'NONE',  #15580 ) ;
#28869 = CARTESIAN_POINT ( 'NONE',  ( -27.16883889988623935, 77.57500000273120122, 19.73931689729374739 ) ) ;
#28870 = ORIENTED_EDGE ( 'NONE', *, *, #4613, .T. ) ;
#28871 = CIRCLE ( 'NONE', #33802, 32.50000000000000000 ) ;
#28872 = CARTESIAN_POINT ( 'NONE',  ( -7.236395654485763274, 18.52499999726881086, 22.27133577429736633 ) ) ;
#28873 = CARTESIAN_POINT ( 'NONE',  ( -27.95245687107222921, 63.13281250000000000, 2.498001805406602216E-13 ) ) ;
#28874 = CARTESIAN_POINT ( 'NONE',  ( -27.16883889988624290, 52.92500000273118843, -19.73931689729374028 ) ) ;
#28875 = CARTESIAN_POINT ( 'NONE',  ( 27.16883889988624290, 14.17500000273118310, 19.73931689729373673 ) ) ;
#28876 = CARTESIAN_POINT ( 'NONE',  ( 33.58253175000000113, 6.375000002731182391, -4.112674001490185761E-15 ) ) ;
#28877 = CARTESIAN_POINT ( 'NONE',  ( 26.07999730980477437, 40.64583333333332860, -6.988114217768290004 ) ) ;
#28878 = CARTESIAN_POINT ( 'NONE',  ( 25.98046417659858420, 28.76340250092398065, 15.04653450569292872 ) ) ;
#28879 = CARTESIAN_POINT ( 'NONE',  ( -28.00173670424535644, 16.86420166574268720, 7.543491769121936308 ) ) ;
#28880 = CARTESIAN_POINT ( 'NONE',  ( 20.08610463437158344, 71.20000000546237118, 27.64615127144129403 ) ) ;
#28881 = CARTESIAN_POINT ( 'NONE',  ( 5.485887633599118468E-07, 52.00000000000003553, -32.49999999999999289 ) ) ;
#28882 = CARTESIAN_POINT ( 'NONE',  ( -33.58253175000000113, 37.12500000273119838, 0.000000000000000000 ) ) ;
#28883 = CARTESIAN_POINT ( 'NONE',  ( 7.025853678916867295, 50.37982666574269075, 26.06988505166722803 ) ) ;
#28884 = CARTESIAN_POINT ( 'NONE',  ( 23.41746824999999887, 6.624999997268815832, 0.000000000000000000 ) ) ;
#28885 = ORIENTED_EDGE ( 'NONE', *, *, #5798, .F. ) ;
#28886 = CARTESIAN_POINT ( 'NONE',  ( 6.486482029760649416E-15, 51.87500000273119127, 35.31076352940723240 ) ) ;
#28887 = CARTESIAN_POINT ( 'NONE',  ( 32.50000000000000000, 51.09999999999998721, -10.55989012756945833 ) ) ;
#28888 = CARTESIAN_POINT ( 'NONE',  ( 26.06988505166735592, 42.37017333425730925, 7.025853678916393896 ) ) ;
#28889 = CARTESIAN_POINT ( 'NONE',  ( -2.162160676586881955E-15, 74.87500000273116996, -35.31076352940723240 ) ) ;
#28890 = ORIENTED_EDGE ( 'NONE', *, *, #26576, .F. ) ;
#28891 = CARTESIAN_POINT ( 'NONE',  ( -33.58253175000000113, 21.22500000273117848, 10.91162601494193929 ) ) ;
#28892 = ORIENTED_EDGE ( 'NONE', *, *, #6119, .T. ) ;
#28893 = CARTESIAN_POINT ( 'NONE',  ( 26.29305231718578995, 29.70000000546238539, -19.10302069950538240 ) ) ;
#28894 = CARTESIAN_POINT ( 'NONE',  ( 20.75514604977249178, 61.82500000273116569, 28.56700777964553950 ) ) ;
#28895 = CARTESIAN_POINT ( 'NONE',  ( 7.505752307973351023, 51.81770833333332860, 28.01184896238290278 ) ) ;
#28896 = VECTOR ( 'NONE', #21278, 1000.000000000000000 ) ;
#28897 = CARTESIAN_POINT ( 'NONE',  ( -24.50000000000000000, 6.749999994537625447, -3.000384657911015469E-15 ) ) ;
#28898 = CARTESIAN_POINT ( 'NONE',  ( 7.236395654485755280, 8.724999997268806595, 22.27133577429736988 ) ) ;
#28899 = CARTESIAN_POINT ( 'NONE',  ( 20.75514604977249178, 1.825000002731179460, 28.56700777964553950 ) ) ;
#28900 = CARTESIAN_POINT ( 'NONE',  ( 33.58253175000000113, 32.47500000273117138, -10.91162601494193751 ) ) ;
#28901 = CARTESIAN_POINT ( 'NONE',  ( -1.053607264507113999E-13, 64.50000000000000000, 32.50000000000000711 ) ) ;
#28902 = CARTESIAN_POINT ( 'NONE',  ( 7.468012846824281681, 66.13503499907601224, -28.02196122052058058 ) ) ;
#28903 = CARTESIAN_POINT ( 'NONE',  ( 5.779280353836490358E-15, 36.49999999999998579, 32.49999999999999289 ) ) ;
#28904 = CARTESIAN_POINT ( 'NONE',  ( 4.300734207923757602, 78.27500000273118985, -13.23629886949340673 ) ) ;
#28905 = CARTESIAN_POINT ( 'NONE',  ( 20.08610463437157279, 17.30000000000000782, -27.64615127144129758 ) ) ;
#28906 = CARTESIAN_POINT ( 'NONE',  ( 24.20753774853731244, 57.69010416666666430, -13.97622843553633132 ) ) ;
#28907 = CARTESIAN_POINT ( 'NONE',  ( -19.82091636218621389, 16.94999999453764161, 14.40073868116558842 ) ) ;
#28908 = CARTESIAN_POINT ( 'NONE',  ( 15.00000000000000000, 73.35000000546237686, -4.873795443493596835 ) ) ;
#28909 = CARTESIAN_POINT ( 'NONE',  ( 6.988114217767829928, 33.19791666666665719, -26.07999730980489872 ) ) ;
#28910 = CARTESIAN_POINT ( 'NONE',  ( 33.58253175000000113, 22.22500000273117493, -10.91162601494193751 ) ) ;
#28911 = CARTESIAN_POINT ( 'NONE',  ( -2.162160676586881955E-15, 72.62500000273118417, -35.31076352940723240 ) ) ;
#28912 = CARTESIAN_POINT ( 'NONE',  ( 20.75514604977249178, 38.07500000273116569, 28.56700777964553950 ) ) ;
#28913 = CARTESIAN_POINT ( 'NONE',  ( 33.58253175000000823, 14.27500000273119340, 10.91162601494192685 ) ) ;
#28914 = CARTESIAN_POINT ( 'NONE',  ( -4.223320258572821363E-15, 80.49999999999998579, 15.00000000000000355 ) ) ;
#28915 = CARTESIAN_POINT ( 'NONE',  ( 26.09010956794232428, 59.27121500092397355, -6.950374756619718042 ) ) ;
#28916 = CARTESIAN_POINT ( 'NONE',  ( -4.223320258572819786E-15, 15.24999999453762278, 24.50000000000000000 ) ) ;
#28917 = CARTESIAN_POINT ( 'NONE',  ( 1.836970198721029589E-15, -22.99999999999999289, 15.00000000000000000 ) ) ;
#28918 =( BOUNDED_CURVE ( )  B_SPLINE_CURVE ( 2, ( #33559, #25840, #10059, #7484, #4903, #15384, #29252, #5587, #10738, #3186, #29745, #32327, #18645 ),
 .UNSPECIFIED., .F., .T. ) 
 B_SPLINE_CURVE_WITH_KNOTS ( ( 3, 2, 2, 2, 2, 2, 3 ),
 ( 0.2371794871794871973, 0.2384615384615384748, 0.2410256410256410298, 0.2435897435897435848, 0.2461538461538461675, 0.2487179487179487225, 0.2500000000000000000 ),
 .UNSPECIFIED. ) 
 CURVE ( )  GEOMETRIC_REPRESENTATION_ITEM ( )  RATIONAL_B_SPLINE_CURVE ( ( 0.9755282581475768211, 0.9755282581475770431, 1.000000000000000000, 0.9510565162951535312, 1.000000000000000000, 0.9510565162951535312, 1.000000000000000000, 0.9510565162951535312, 1.000000000000000000, 0.9510565162951535312, 1.000000000000000000, 0.9755282581475768211, 0.9755282581475768211 ) ) 
 REPRESENTATION_ITEM ( '' )  );
#28919 = CARTESIAN_POINT ( 'NONE',  ( -32.50000000000000000, 52.00000000000000711, 0.000000000000000000 ) ) ;
#28920 = LINE ( 'NONE', #5420, #2952 ) ;
#28921 = CARTESIAN_POINT ( 'NONE',  ( -10.37757302488624411, 58.72500000273117848, -31.93888565452638417 ) ) ;
#28922 = CARTESIAN_POINT ( 'NONE',  ( 14.47279130897151589, 6.824999997268808904, 19.92008829642072953 ) ) ;
#28923 = VECTOR ( 'NONE', #1331, 1000.000000000000000 ) ;
#28924 = EDGE_LOOP ( 'NONE', ( #30917, #7493, #10685, #24702 ) ) ;
#28925 = CARTESIAN_POINT ( 'NONE',  ( -20.75514604977248823, 71.07500000273117280, -28.56700777964554305 ) ) ;
#28926 = CARTESIAN_POINT ( 'NONE',  ( 27.16883889988623935, 4.325000002731171911, -19.73931689729374384 ) ) ;
#28927 = CARTESIAN_POINT ( 'NONE',  ( 14.47279130897151767, 17.42499999726882365, -19.92008829642072598 ) ) ;
#28928 = CARTESIAN_POINT ( 'NONE',  ( 13.94119854578937812, 18.73736083425731636, 24.22776226481240514 ) ) ;
#28929 = ORIENTED_EDGE ( 'NONE', *, *, #23684, .T. ) ;
#28930 = CARTESIAN_POINT ( 'NONE',  ( -2.162160676586881955E-15, 40.62500000273120548, -35.31076352940723240 ) ) ;
#28931 = DIRECTION ( 'NONE',  ( 0.000000000000000000, 0.000000000000000000, 1.000000000000000000 ) ) ;
#28932 = ORIENTED_EDGE ( 'NONE', *, *, #10321, .F. ) ;
#28933 = CARTESIAN_POINT ( 'NONE',  ( -28.01184896238290278, 45.80208333333333570, 7.505752307973363457 ) ) ;
#28934 = CARTESIAN_POINT ( 'NONE',  ( 26.29305231718579350, 11.30000000546238503, 19.10302069950537529 ) ) ;
#28935 = CARTESIAN_POINT ( 'NONE',  ( -2.092463501923844636E-15, 6.000000005462371888, -34.17252228774368916 ) ) ;
#28936 = CARTESIAN_POINT ( 'NONE',  ( -33.58253175000000113, 79.12500000273119838, 0.000000000000000000 ) ) ;
#28937 = CARTESIAN_POINT ( 'NONE',  ( 26.00068869287367335, 23.88802083333331794, 15.01150461594596308 ) ) ;
#28938 = CARTESIAN_POINT ( 'NONE',  ( -18.94512977948576093, 15.82499999726880091, 13.76444248337722698 ) ) ;
#28939 = CARTESIAN_POINT ( 'NONE',  ( -33.58253175000000113, 9.375000002731169957, 0.000000000000000000 ) ) ;
#28940 = ADVANCED_FACE ( 'NONE', ( #17952 ), #25997, .T. ) ;
#28941 = CARTESIAN_POINT ( 'NONE',  ( 26.29305231718578995, 61.20000000000000284, -19.10302069950538240 ) ) ;
#28942 = CARTESIAN_POINT ( 'NONE',  ( 26.29305231718578995, 57.70000000546238539, -19.10302069950538240 ) ) ;
#28943 = CARTESIAN_POINT ( 'NONE',  ( -32.50000000000000000, 30.10000000000000853, 10.55989012756946366 ) ) ;
#28944 = CARTESIAN_POINT ( 'NONE',  ( 0.04044903255045854962, 36.77305583240936215, 30.02300923189239867 ) ) ;
#28945 = CARTESIAN_POINT ( 'NONE',  ( -13.91746824999999532, 77.27500000273117564, -4.522059556121115875 ) ) ;
#28946 = CARTESIAN_POINT ( 'NONE',  ( 7.505752307972854531, 36.63541666666666430, -28.01184896238303423 ) ) ;
#28947 = EDGE_CURVE ( 'NONE', #29507, #25961, #27559, .T. ) ;
#28948 =( REPRESENTATION_RELATIONSHIP ('NONE','NONE', #5873, #31529 ) REPRESENTATION_RELATIONSHIP_WITH_TRANSFORMATION ( #31352 )SHAPE_REPRESENTATION_RELATIONSHIP( ) );
#28949 = FACE_OUTER_BOUND ( 'NONE', #23759, .T. ) ;
#28950 = CARTESIAN_POINT ( 'NONE',  ( -15.14183272437242778, 1.299999999999988054, 20.84094480462497856 ) ) ;
#28951 = CARTESIAN_POINT ( 'NONE',  ( 20.08610463437157279, 3.299999999999983391, -27.64615127144129758 ) ) ;
#28952 = CIRCLE ( 'NONE', #19616, 26.50000000000000355 ) ;
#28953 = CARTESIAN_POINT ( 'NONE',  ( 5.204170427930421283E-15, -70.99969134886156041, 0.000000000000000000 ) ) ;
#28954 = CARTESIAN_POINT ( 'NONE',  ( -6.950374756619247307, 60.97878499907603356, 26.09010956794245217 ) ) ;
#28955 = CARTESIAN_POINT ( 'NONE',  ( 10.37757302488624056, 50.52500000273118985, -31.93888565452638417 ) ) ;
#28956 = CARTESIAN_POINT ( 'NONE',  ( -8.960552108402742093E-16, 78.37500000273119838, -14.63369212191046387 ) ) ;
#28957 = CARTESIAN_POINT ( 'NONE',  ( -20.75514604977248112, 55.67500000273118843, 28.56700777964554661 ) ) ;
#28958 = CARTESIAN_POINT ( 'NONE',  ( -10.37757302488623701, 31.77500000273120051, 31.93888565452638417 ) ) ;
#28959 = CARTESIAN_POINT ( 'NONE',  ( 0.000000000000000000, 0.000000000000000000, 0.000000000000000000 ) ) ;
#28960 = CARTESIAN_POINT ( 'NONE',  ( 1.806199397676865774E-16, -24.47487373415291145, 0.000000000000000000 ) ) ;
#28961 = CARTESIAN_POINT ( 'NONE',  ( 20.08610463437158344, 15.20000000546237118, 27.64615127144129403 ) ) ;
#28962 = DIRECTION ( 'NONE',  ( 0.000000000000000000, 1.000000000000000000, 0.000000000000000000 ) ) ;
#28963 = CARTESIAN_POINT ( 'NONE',  ( -20.08610463437157989, 73.70000000000000284, -27.64615127144129758 ) ) ;
#28964 = CARTESIAN_POINT ( 'NONE',  ( 27.16883889988624290, 13.92500000273118310, 19.73931689729373673 ) ) ;
#28965 = CARTESIAN_POINT ( 'NONE',  ( 7.236395654485760609, 1.024999997268821739, -22.27133577429736633 ) ) ;
#28966 = CARTESIAN_POINT ( 'NONE',  ( 19.82091636218621389, 12.19999999999998863, -14.40073868116559197 ) ) ;
#28967 = CARTESIAN_POINT ( 'NONE',  ( -24.18731323226221974, 20.15847249907602290, 14.01125832528330406 ) ) ;
#28968 = CARTESIAN_POINT ( 'NONE',  ( -2.092463501923844636E-15, 38.00000000546237544, -34.17252228774368916 ) ) ;
#28969 = CARTESIAN_POINT ( 'NONE',  ( -5.147494310547423346, 12.44874571845314115, 32.50000000000000000 ) ) ;
#28970 = CARTESIAN_POINT ( 'NONE',  ( 33.58253175000000113, 28.22500000273118914, -10.91162601494193574 ) ) ;
#28971 = CARTESIAN_POINT ( 'NONE',  ( 26.07999730980477437, 47.52083333333332860, -6.988114217768290004 ) ) ;
#28972 = ORIENTED_EDGE ( 'NONE', *, *, #12161, .F. ) ;
#28973 = CARTESIAN_POINT ( 'NONE',  ( -2.162160676586881955E-15, 60.62500000273117706, -35.31076352940723240 ) ) ;
#28974 = ORIENTED_EDGE ( 'NONE', *, *, #32075, .T. ) ;
#28975 = CARTESIAN_POINT ( 'NONE',  ( 2.740863092043355209E-13, 14.14843749999999289, 30.02300923189239512 ) ) ;
#28976 = CARTESIAN_POINT ( 'NONE',  ( 20.47846945139902530, 15.15663166759064495, 20.53372385742071771 ) ) ;
#28977 = CARTESIAN_POINT ( 'NONE',  ( 6.486482029760649416E-15, 5.625000002731175286, 35.31076352940723240 ) ) ;
#28978 = EDGE_LOOP ( 'NONE', ( #7363, #14964, #1778, #29709 ) ) ;
#28979 = CARTESIAN_POINT ( 'NONE',  ( 18.94512977948575738, 2.424999997268806329, 13.76444248337723408 ) ) ;
#28980 = CARTESIAN_POINT ( 'NONE',  ( 10.37757302488624056, 32.77500000273120406, -31.93888565452638417 ) ) ;
#28981 = CARTESIAN_POINT ( 'NONE',  ( -2.092463501923844636E-15, 36.00000000546238255, -34.17252228774368916 ) ) ;
#28982 = ADVANCED_FACE ( 'NONE', ( #12959 ), #31941, .T. ) ;
#28983 = CARTESIAN_POINT ( 'NONE',  ( 2.897257156509938333E-15, 72.50000000000004263, 15.77193336357400710 ) ) ;
#28984 = CARTESIAN_POINT ( 'NONE',  ( -1.778240108872766143E-15, 54.00000000546237544, -32.49999999999999289 ) ) ;
#28985 = CARTESIAN_POINT ( 'NONE',  ( 33.58253175000000113, 46.47500000273118559, -10.91162601494193751 ) ) ;
#28986 = APPLICATION_PROTOCOL_DEFINITION ( 'draft international standard', 'automotive_design', 1998, #2651 ) ;
#28987 = CARTESIAN_POINT ( 'NONE',  ( -10.04305231718578462, 24.39999999999999147, 30.90933677959249337 ) ) ;
#28988 = CARTESIAN_POINT ( 'NONE',  ( -10.04305231718579172, 23.60000000000000853, -30.90933677959248982 ) ) ;
#28989 = CARTESIAN_POINT ( 'NONE',  ( -15.14183272437242600, 5.300000000000006928, 20.84094480462497856 ) ) ;
#28990 = CARTESIAN_POINT ( 'NONE',  ( -10.37757302488624411, 66.72500000273117848, -31.93888565452638417 ) ) ;
#28991 = CARTESIAN_POINT ( 'NONE',  ( -31.78338918835712334, 66.99999999999997158, 9.699108655006819291 ) ) ;
#28992 = CARTESIAN_POINT ( 'NONE',  ( -10.04305231718579172, 37.59999999999999432, -30.90933677959248982 ) ) ;
#28993 = CARTESIAN_POINT ( 'NONE',  ( -27.16883889988624290, 53.17500000273117422, -19.73931689729374028 ) ) ;
#28994 = CARTESIAN_POINT ( 'NONE',  ( -33.58253175000000113, 13.02500000273117564, -10.91162601494193218 ) ) ;
#28995 = CARTESIAN_POINT ( 'NONE',  ( -14.01125832528285109, 26.18527750092397710, 24.18731323226248264 ) ) ;
#28996 = CARTESIAN_POINT ( 'NONE',  ( 15.14183272437242422, 2.049999994537635484, -20.84094480462497856 ) ) ;
#28997 = CARTESIAN_POINT ( 'NONE',  ( 0.000000000000000000, -20.99999999999998934, -26.50000000000000355 ) ) ;
#28998 = CARTESIAN_POINT ( 'NONE',  ( 20.75514604977249178, 37.82500000273117280, 28.56700777964553950 ) ) ;
#28999 = CARTESIAN_POINT ( 'NONE',  ( 5.147494310547327423, 45.05125428700921475, 32.50000000000003553 ) ) ;
#29000 = CARTESIAN_POINT ( 'NONE',  ( 21.62020457442521248, 52.08848768517668049, 27.37635686616407327 ) ) ;
#29001 = CARTESIAN_POINT ( 'NONE',  ( -11.25946833292375793, 78.67500000273119554, -8.180482586598733619 ) ) ;
#29002 = CARTESIAN_POINT ( 'NONE',  ( -20.53372385742107653, 48.37461833240936215, -20.47846945139867003 ) ) ;
#29003 = CARTESIAN_POINT ( 'NONE',  ( 32.50000000000000000, 57.50000000546238965, -3.980102097228898626E-15 ) ) ;
#29004 = CARTESIAN_POINT ( 'NONE',  ( -11.25946833292375793, 77.17500000273119554, -8.180482586598733619 ) ) ;
#29005 = DIRECTION ( 'NONE',  ( -0.000000000000000000, -1.000000000000000000, -0.000000000000000000 ) ) ;
#29006 = CARTESIAN_POINT ( 'NONE',  ( 19.09188309203661049, 12.85937500000000000, -19.09188309203694445 ) ) ;
#29007 = CARTESIAN_POINT ( 'NONE',  ( -23.41746825000000598, 8.224999997268824359, 7.608796670333726198 ) ) ;
#29008 = CARTESIAN_POINT ( 'NONE',  ( 6.277390505771533514E-15, 67.00000000546236834, 34.17252228774368916 ) ) ;
#29009 = CARTESIAN_POINT ( 'NONE',  ( 28.01184896238290278, 20.02083333333332860, -7.505752307973347470 ) ) ;
#29010 = CARTESIAN_POINT ( 'NONE',  ( 33.58253175000000113, 28.47500000273118204, -10.91162601494193751 ) ) ;
#29011 = CARTESIAN_POINT ( 'NONE',  ( -23.41746824999999887, 16.12499999726882294, -2.867812753649727150E-15 ) ) ;
#29012 = ORIENTED_EDGE ( 'NONE', *, *, #23142, .F. ) ;
#29013 = CARTESIAN_POINT ( 'NONE',  ( -15.04653450569291984, 43.37277750092397355, 25.98046417659859486 ) ) ;
#29014 = CARTESIAN_POINT ( 'NONE',  ( 26.29305231718578995, 15.70000000546238539, -19.10302069950538240 ) ) ;
#29015 = CARTESIAN_POINT ( 'NONE',  ( 7.505752307973351023, 48.38020833333332860, 28.01184896238290278 ) ) ;
#29016 = CARTESIAN_POINT ( 'NONE',  ( 32.50000000000000000, 75.00000000000001421, -3.980102097228898626E-15 ) ) ;
#29017 = CARTESIAN_POINT ( 'NONE',  ( 33.58253175000000113, 52.37500000273121259, -4.112674001490185761E-15 ) ) ;
#29018 = CARTESIAN_POINT ( 'NONE',  ( -32.50000000000000000, 54.60000000546237686, 10.55989012756946366 ) ) ;
#29019 = CARTESIAN_POINT ( 'NONE',  ( -13.91746824999999887, 77.37500000273116996, 0.000000000000000000 ) ) ;
#29020 = CARTESIAN_POINT ( 'NONE',  ( 33.58253175000000113, 44.22500000273117138, -10.91162601494193751 ) ) ;
#29021 = CARTESIAN_POINT ( 'NONE',  ( -15.00000000000000000, 76.35000000546239107, 4.873795443493597723 ) ) ;
#29022 = CARTESIAN_POINT ( 'NONE',  ( -20.75514604977248112, 67.67500000273116711, 28.56700777964554661 ) ) ;
#29023 = CARTESIAN_POINT ( 'NONE',  ( -10.37757302488623701, 59.52500000273118275, 31.93888565452638417 ) ) ;
#29024 = CARTESIAN_POINT ( 'NONE',  ( 26.00068869287367690, 20.45052083333332860, 15.01150461594596486 ) ) ;
#29025 = CARTESIAN_POINT ( 'NONE',  ( -20.08610463437156923, 38.29999999999997584, 27.64615127144130113 ) ) ;
#29026 = CARTESIAN_POINT ( 'NONE',  ( -4.523095164977116484E-15, 4.124999997268806951, 24.62258325217400312 ) ) ;
#29027 = CARTESIAN_POINT ( 'NONE',  ( 20.75514604977249178, 12.07500000273120655, 28.56700777964553950 ) ) ;
#29028 = CARTESIAN_POINT ( 'NONE',  ( -1.778240108872766143E-15, 36.00000000546238255, -32.49999999999999289 ) ) ;
#29029 = CARTESIAN_POINT ( 'NONE',  ( 26.06988505166722803, 35.77045166574266943, -7.025853678916862854 ) ) ;
#29030 = CARTESIAN_POINT ( 'NONE',  ( 13.91746824999999887, 72.37500000273119838, -1.704398294459741270E-15 ) ) ;
#29031 = CARTESIAN_POINT ( 'NONE',  ( -27.16883889988624290, 73.17500000273119554, -19.73931689729374028 ) ) ;
#29032 = CYLINDRICAL_SURFACE ( 'NONE', #8356, 24.50000000000000000 ) ;
#29033 = CARTESIAN_POINT ( 'NONE',  ( 33.58253175000000113, 72.37500000273118417, -4.112674001490185761E-15 ) ) ;
#29034 = ORIENTED_EDGE ( 'NONE', *, *, #30108, .T. ) ;
#29035 = CARTESIAN_POINT ( 'NONE',  ( 18.94512977948576093, 17.32499999726880446, -13.76444248337722875 ) ) ;
#29036 = CARTESIAN_POINT ( 'NONE',  ( 19.09188309203661049, 60.98437499999999289, -19.09188309203694445 ) ) ;
#29037 = CARTESIAN_POINT ( 'NONE',  ( 33.58253175000000113, 54.12500000273119838, -4.112674001490185761E-15 ) ) ;
#29038 = CARTESIAN_POINT ( 'NONE',  ( 6.486482029760649416E-15, 15.87500000273120015, 35.31076352940723240 ) ) ;
#29039 = CARTESIAN_POINT ( 'NONE',  ( 20.75514604977249178, 6.075000002731190563, 28.56700777964553950 ) ) ;
#29040 = CARTESIAN_POINT ( 'NONE',  ( -13.97622843553588901, 41.93489583333333570, 24.20753774853756823 ) ) ;
#29041 = CARTESIAN_POINT ( 'NONE',  ( -7.468012846824771955, 27.47434000092397000, -28.02196122052045624 ) ) ;
#29042 = CARTESIAN_POINT ( 'NONE',  ( 28.00173670424535644, 22.02045166574269075, -7.543491769121920321 ) ) ;
#29043 = CARTESIAN_POINT ( 'NONE',  ( 20.08610463437158344, 75.20000000546241381, 27.64615127144129403 ) ) ;
#29044 = CARTESIAN_POINT ( 'NONE',  ( -26.29305231718578995, 56.70000000546237828, 19.10302069950538595 ) ) ;
#29045 = CARTESIAN_POINT ( 'NONE',  ( -20.75514604977248823, 40.82500000273119412, -28.56700777964554305 ) ) ;
#29046 = CARTESIAN_POINT ( 'NONE',  ( -13.94119854578892514, 47.37201416574269786, 24.22776226481266448 ) ) ;
#29047 = CARTESIAN_POINT ( 'NONE',  ( 14.47279130897151767, 16.92499999726880944, -19.92008829642072598 ) ) ;
#29048 = CYLINDRICAL_SURFACE ( 'NONE', #7890, 32.50000000000000000 ) ;
#29049 = ORIENTED_EDGE ( 'NONE', *, *, #30013, .F. ) ;
#29050 = CARTESIAN_POINT ( 'NONE',  ( 20.75514604977249178, 46.07500000273117280, 28.56700777964553950 ) ) ;
#29051 = CARTESIAN_POINT ( 'NONE',  ( 26.29305231718579350, 50.80000000000001137, 19.10302069950537529 ) ) ;
#29052 = CARTESIAN_POINT ( 'NONE',  ( 19.06425588902592239, 49.53163166759063785, 19.11951029504763611 ) ) ;
#29053 = CARTESIAN_POINT ( 'NONE',  ( -33.58253175000000113, 69.27500000273116143, -10.91162601494193218 ) ) ;
#29054 = ORIENTED_EDGE ( 'NONE', *, *, #11771, .F. ) ;
#29055 = CARTESIAN_POINT ( 'NONE',  ( 10.37757302488624056, 18.52500000273120406, -31.93888565452638417 ) ) ;
#29056 = CARTESIAN_POINT ( 'NONE',  ( 26.00068869287367335, 27.32552083333332860, 15.01150461594596308 ) ) ;
#29057 = ORIENTED_EDGE ( 'NONE', *, *, #24810, .T. ) ;
#29058 = CARTESIAN_POINT ( 'NONE',  ( 0.000000000000000000, 0.000000000000000000, 16.50000000000002842 ) ) ;
#29059 = CARTESIAN_POINT ( 'NONE',  ( 27.16883889988623935, 64.32500000273120122, -19.73931689729374384 ) ) ;
#29060 = CARTESIAN_POINT ( 'NONE',  ( 30.02300923189239512, 44.22656249999997868, -2.619432448724977703E-13 ) ) ;
#29061 = CARTESIAN_POINT ( 'NONE',  ( -32.50000000000000000, 66.60000000546237686, 10.55989012756946366 ) ) ;
#29062 = CARTESIAN_POINT ( 'NONE',  ( -23.41746825000000243, 10.22499999726881725, 7.608796670333725309 ) ) ;
#29063 = CARTESIAN_POINT ( 'NONE',  ( 20.75514604977249178, 5.825000002731198556, 28.56700777964553950 ) ) ;
#29064 = CARTESIAN_POINT ( 'NONE',  ( -27.16883889988624290, 33.17500000273118843, -19.73931689729374028 ) ) ;
#29065 = CARTESIAN_POINT ( 'NONE',  ( -4.635254915624211769, 77.85000000546237686, -14.26584774442730286 ) ) ;
#29066 = CARTESIAN_POINT ( 'NONE',  ( -20.47846945139866648, 64.70274333240935505, 20.53372385742108008 ) ) ;
#29067 = DIRECTION ( 'NONE',  ( 0.000000000000000000, 1.000000000000000000, 0.000000000000000000 ) ) ;
#29068 = CARTESIAN_POINT ( 'NONE',  ( 20.08610463437158344, 65.20000000546235697, 27.64615127144129403 ) ) ;
#29069 = CARTESIAN_POINT ( 'NONE',  ( 10.04305231718578817, 9.399999999999991473, -30.90933677959249337 ) ) ;
#29070 = EDGE_CURVE ( 'NONE', #1729, #21053, #22499, .T. ) ;
#29071 = CARTESIAN_POINT ( 'NONE',  ( 20.08610463437157279, 19.30000000000000426, -27.64615127144129758 ) ) ;
#29072 = CARTESIAN_POINT ( 'NONE',  ( 6.988114217767829928, 60.69791666666667140, -26.07999730980489872 ) ) ;
#29073 = CARTESIAN_POINT ( 'NONE',  ( 23.41746824999999887, 1.124999997268810725, 0.000000000000000000 ) ) ;
#29074 = CARTESIAN_POINT ( 'NONE',  ( -4.300734207923755825, 77.27500000273118985, 13.23629886949340673 ) ) ;
#29075 = CARTESIAN_POINT ( 'NONE',  ( 6.988114217767829928, 36.63541666666666430, -26.07999730980489872 ) ) ;
#29076 = CARTESIAN_POINT ( 'NONE',  ( -20.75514604977248112, 23.42500000273119909, 28.56700777964554661 ) ) ;
#29077 = CARTESIAN_POINT ( 'NONE',  ( -27.16883889988623935, 73.32500000273118701, 19.73931689729374739 ) ) ;
#29078 = CARTESIAN_POINT ( 'NONE',  ( 20.75514604977248467, 38.67500000273117422, -28.56700777964554305 ) ) ;
#29079 = CARTESIAN_POINT ( 'NONE',  ( -20.75514604977248112, 15.67500000273117777, 28.56700777964554661 ) ) ;
#29080 = CARTESIAN_POINT ( 'NONE',  ( 24.22776226481241224, 55.69048583425730925, -13.94119854578936923 ) ) ;
#29081 = EDGE_CURVE ( 'NONE', #21432, #1133, #5404, .T. ) ;
#29082 = CARTESIAN_POINT ( 'NONE',  ( 20.75514604977248467, 70.42500000273119554, -28.56700777964554305 ) ) ;
#29083 = ADVANCED_FACE ( 'NONE', ( #8640 ), #32311, .F. ) ;
#29084 = CARTESIAN_POINT ( 'NONE',  ( -10.04305231718578462, 52.39999999999999147, 30.90933677959249337 ) ) ;
#29085 = CARTESIAN_POINT ( 'NONE',  ( 3.445340210940985210E-14, 7.499999999999994671, 24.50000000000000000 ) ) ;
#29086 = CARTESIAN_POINT ( 'NONE',  ( -33.58253175000000113, 57.02500000273118275, -10.91162601494193041 ) ) ;
#29087 = CARTESIAN_POINT ( 'NONE',  ( -18.94512977948576093, 8.324999997268822227, 13.76444248337722698 ) ) ;
#29088 = ORIENTED_EDGE ( 'NONE', *, *, #22904, .T. ) ;
#29089 = CARTESIAN_POINT ( 'NONE',  ( 33.58253175000000113, 66.47500000273119269, -10.91162601494193751 ) ) ;
#29090 = CARTESIAN_POINT ( 'NONE',  ( -20.08610463437156923, 16.29999999999997939, 27.64615127144130113 ) ) ;
#29091 = CARTESIAN_POINT ( 'NONE',  ( -23.41746825000000243, 18.02499999726880731, -7.608796670333730638 ) ) ;
#29092 = CARTESIAN_POINT ( 'NONE',  ( 13.94119854578937812, 15.29986083425731280, 24.22776226481240514 ) ) ;
#29093 = ORIENTED_EDGE ( 'NONE', *, *, #5807, .T. ) ;
#29094 = CARTESIAN_POINT ( 'NONE',  ( 27.16883889988623935, 46.32500000273119412, -19.73931689729374384 ) ) ;
#29095 = CARTESIAN_POINT ( 'NONE',  ( -32.50000000000000000, 68.50000000546238255, 0.000000000000000000 ) ) ;
#29096 = VERTEX_POINT ( 'NONE', #21368 ) ;
#29097 = CARTESIAN_POINT ( 'NONE',  ( 28.01184896238304134, 40.93229166666666430, 7.505752307972846538 ) ) ;
#29098 = CARTESIAN_POINT ( 'NONE',  ( -10.04305231718579172, 60.10000000546238397, -30.90933677959248982 ) ) ;
#29099 = CARTESIAN_POINT ( 'NONE',  ( -32.50000000000000000, 6.600000005462382191, 10.55989012756946366 ) ) ;
#29100 = CARTESIAN_POINT ( 'NONE',  ( 33.58253175000000113, 78.22500000273119269, -10.91162601494193751 ) ) ;
#29101 = CARTESIAN_POINT ( 'NONE',  ( -20.50609665440969209, 21.45312499999999645, 20.50609665441005092 ) ) ;
#29102 = CARTESIAN_POINT ( 'NONE',  ( -15.14183272437241889, 2.700000000000001954, -20.84094480462497856 ) ) ;
#29103 = CARTESIAN_POINT ( 'NONE',  ( 33.58253175000000823, 8.275000002731179194, 10.91162601494192863 ) ) ;
#29104 = CARTESIAN_POINT ( 'NONE',  ( -32.50000000000000000, 58.10000000000000142, 10.55989012756946366 ) ) ;
#29105 = CARTESIAN_POINT ( 'NONE',  ( -8.601468415847518756, 78.57500000273120122, -11.83890561707634603 ) ) ;
#29106 = DIRECTION ( 'NONE',  ( 0.000000000000000000, 0.000000000000000000, -1.000000000000000000 ) ) ;
#29107 = CARTESIAN_POINT ( 'NONE',  ( 20.47846945139867003, 32.04649333240934084, -20.53372385742107653 ) ) ;
#29108 = AXIS2_PLACEMENT_3D ( 'NONE', #3083, #10803, #21444 ) ;
#29109 = CARTESIAN_POINT ( 'NONE',  ( 8.601468415847516980, 76.67500000273116711, -11.83890561707634781 ) ) ;
#29110 = CARTESIAN_POINT ( 'NONE',  ( -7.505752307972844761, 45.22916666666665719, 28.01184896238304134 ) ) ;
#29111 = APPLICATION_PROTOCOL_DEFINITION ( 'draft international standard', 'automotive_design', 1998, #6136 ) ;
#29112 = CARTESIAN_POINT ( 'NONE',  ( -4.936660134684515206E-16, -18.96891108675447768, 0.000000000000000000 ) ) ;
#29113 = CARTESIAN_POINT ( 'NONE',  ( -24.50000000000000000, 1.000000000000000888, -3.000384657911015469E-15 ) ) ;
#29114 = CARTESIAN_POINT ( 'NONE',  ( 6.277390505771533514E-15, 2.500000000000008882, 34.17252228774368916 ) ) ;
#29115 = CARTESIAN_POINT ( 'NONE',  ( 0.000000000000000000, 52.00000000000000711, 0.000000000000000000 ) ) ;
#29116 = CARTESIAN_POINT ( 'NONE',  ( 13.94119854578893580, 66.27826416574268364, -24.22776226481265383 ) ) ;
#29117 =( BOUNDED_CURVE ( )  B_SPLINE_CURVE ( 2, ( #25373, #30507, #4264, #14738, #32902, #7176, #24857, #27778, #20404, #3929, #27604, #17150, #1677 ),
 .UNSPECIFIED., .F., .T. ) 
 B_SPLINE_CURVE_WITH_KNOTS ( ( 3, 2, 2, 2, 2, 2, 3 ),
 ( 0.3397435897435897578, 0.3410256410256410353, 0.3435897435897435903, 0.3461538461538461453, 0.3487179487179487003, 0.3512820512820512553, 0.3525641025641025883 ),
 .UNSPECIFIED. ) 
 CURVE ( )  GEOMETRIC_REPRESENTATION_ITEM ( )  RATIONAL_B_SPLINE_CURVE ( ( 0.9755282581475768211, 0.9755282581475768211, 1.000000000000000000, 0.9510565162951535312, 1.000000000000000000, 0.9510565162951535312, 1.000000000000000000, 0.9510565162951535312, 1.000000000000000000, 0.9510565162951535312, 1.000000000000000000, 0.9755282581475762660, 0.9755282581475768211 ) ) 
 REPRESENTATION_ITEM ( '' )  );
#29118 = CARTESIAN_POINT ( 'NONE',  ( -20.75514604977248112, 41.42500000273118133, 28.56700777964554661 ) ) ;
#29119 = CARTESIAN_POINT ( 'NONE',  ( 2.897257156509938333E-15, 72.75000000546239676, 15.77193336357400710 ) ) ;
#29120 = CARTESIAN_POINT ( 'NONE',  ( 6.486482029760649416E-15, 57.87500000273117706, 35.31076352940723240 ) ) ;
#29121 = CARTESIAN_POINT ( 'NONE',  ( -20.75514604977248112, 35.67500000273118843, 28.56700777964554661 ) ) ;
#29122 = CARTESIAN_POINT ( 'NONE',  ( 32.50000000000000711, 23.40000000546237402, 10.55989012756945122 ) ) ;
#29123 = CARTESIAN_POINT ( 'NONE',  ( 19.09188309203694800, 20.59374999999999645, 19.09188309203660694 ) ) ;
#29124 = LINE ( 'NONE', #5959, #20189 ) ;
#29125 = CARTESIAN_POINT ( 'NONE',  ( -1.778240108872766143E-15, 49.50000000000000000, -32.49999999999999289 ) ) ;
#29126 = CARTESIAN_POINT ( 'NONE',  ( -2.092463501923844636E-15, 73.49999999999998579, -34.17252228774368916 ) ) ;
#29127 = CARTESIAN_POINT ( 'NONE',  ( 33.58253175000000823, 18.02500000273118630, 10.91162601494192863 ) ) ;
#29128 = CARTESIAN_POINT ( 'NONE',  ( 18.94512977948576093, 6.824999997268821339, -13.76444248337722875 ) ) ;
#29129 = DIRECTION ( 'NONE',  ( -0.000000000000000000, -1.000000000000000000, -0.000000000000000000 ) ) ;
#29130 = CARTESIAN_POINT ( 'NONE',  ( 13.94119854578893580, 21.59076416574269430, -24.22776226481265383 ) ) ;
#29131 = EDGE_CURVE ( 'NONE', #684, #7428, #28618, .T. ) ;
#29132 = CARTESIAN_POINT ( 'NONE',  ( -1.778240108872766143E-15, 11.49999999999999112, -32.49999999999999289 ) ) ;
#29133 = CARTESIAN_POINT ( 'NONE',  ( 33.58253175000000823, 22.02500000273118275, 10.91162601494192685 ) ) ;
#29134 = CARTESIAN_POINT ( 'NONE',  ( -26.07999730980477437, 42.36458333333332860, 6.988114217768305103 ) ) ;
#29135 = ORIENTED_EDGE ( 'NONE', *, *, #15884, .F. ) ;
#29136 = CARTESIAN_POINT ( 'NONE',  ( 33.58253175000000113, 60.22500000273119980, -10.91162601494193751 ) ) ;
#29137 = EDGE_LOOP ( 'NONE', ( #32633, #4741 ) ) ;
#29138 = CARTESIAN_POINT ( 'NONE',  ( -25.98046417659859486, 64.85715250092397355, -15.04653450569291628 ) ) ;
#29139 = CARTESIAN_POINT ( 'NONE',  ( 7.543491769121427382, 14.01079833425730747, -28.00173670424548433 ) ) ;
#29140 = CARTESIAN_POINT ( 'NONE',  ( -33.58253175000000113, 7.125000002731182391, 0.000000000000000000 ) ) ;
#29141 = ORIENTED_EDGE ( 'NONE', *, *, #3192, .F. ) ;
#29142 = CARTESIAN_POINT ( 'NONE',  ( -14.47279130897151589, 1.324999997268808238, -19.92008829642072598 ) ) ;
#29143 = CARTESIAN_POINT ( 'NONE',  ( -10.37757302488624411, 26.97500000273117493, -31.93888565452638417 ) ) ;
#29144 = CARTESIAN_POINT ( 'NONE',  ( 26.29305231718578995, 37.70000000546236407, -19.10302069950538240 ) ) ;
#29145 = CARTESIAN_POINT ( 'NONE',  ( -32.50000000000000000, 79.90000000000001990, -10.55989012756945478 ) ) ;
#29146 = CARTESIAN_POINT ( 'NONE',  ( -20.08610463437156923, 52.80000000546237260, 27.64615127144130113 ) ) ;
#29147 = CARTESIAN_POINT ( 'NONE',  ( 20.75514604977249178, 46.07500000273117280, 28.56700777964553950 ) ) ;
#29148 = CARTESIAN_POINT ( 'NONE',  ( 32.50000000000000000, 25.00000000000000711, -3.980102097228898626E-15 ) ) ;
#29149 = CARTESIAN_POINT ( 'NONE',  ( -20.08610463437157989, 23.70000000000000639, -27.64615127144129758 ) ) ;
#29150 = CARTESIAN_POINT ( 'NONE',  ( 1.577395562988744260E-15, 4.500000000000003553, -25.76082449383753925 ) ) ;
#29151 = CARTESIAN_POINT ( 'NONE',  ( 20.75514604977249178, 65.82500000273115859, 28.56700777964553950 ) ) ;
#29152 = CARTESIAN_POINT ( 'NONE',  ( -33.24513298742183309, 66.99999999999998579, 2.427281437204855230 ) ) ;
#29153 = CARTESIAN_POINT ( 'NONE',  ( -26.29305231718579350, 76.30000000546239391, -19.10302069950537884 ) ) ;
#29154 = CARTESIAN_POINT ( 'NONE',  ( -10.37757302488623701, 53.77500000273119696, 31.93888565452638417 ) ) ;
#29155 = CARTESIAN_POINT ( 'NONE',  ( -14.47279130897152299, 1.924999997268818541, 19.92008829642072243 ) ) ;
#29156 = CARTESIAN_POINT ( 'NONE',  ( -19.82091636218621389, 9.200000000000013500, 14.40073868116558842 ) ) ;
#29157 = CARTESIAN_POINT ( 'NONE',  ( -27.16883889988624290, 14.92500000273117067, -19.73931689729374028 ) ) ;
#29158 = CARTESIAN_POINT ( 'NONE',  ( -19.06425588902591173, 30.62538166759064495, -19.11951029504763611 ) ) ;
#29159 = CARTESIAN_POINT ( 'NONE',  ( 19.22940031075280132, 66.99999999999994316, -26.85591229561295989 ) ) ;
#29160 = CARTESIAN_POINT ( 'NONE',  ( -22.34582402162608616, 52.00000000000002842, 24.25905220314540500 ) ) ;
#29161 = CARTESIAN_POINT ( 'NONE',  ( 27.16883889988624290, 31.92500000273119909, 19.73931689729373673 ) ) ;
#29163 = CARTESIAN_POINT ( 'NONE',  ( -1.778240108872766143E-15, 65.50000000000000000, -32.49999999999999289 ) ) ;
#29162 = ADVANCED_BREP_SHAPE_REPRESENTATION ( '', ( #32070, #1376 ), #19430 ) ;
#29164 = DIRECTION ( 'NONE',  ( 0.000000000000000000, 0.000000000000000000, -1.000000000000000000 ) ) ;
#29165 = CARTESIAN_POINT ( 'NONE',  ( 8.601468415847516980, 80.17500000273112448, -11.83890561707634603 ) ) ;
#29166 = CARTESIAN_POINT ( 'NONE',  ( -26.02091320914878025, 44.79388916574269075, -14.97647472619899389 ) ) ;
#29167 = CARTESIAN_POINT ( 'NONE',  ( 32.50000000000000711, 57.40000000546237402, 10.55989012756945122 ) ) ;
#29168 = ADVANCED_FACE ( 'NONE', ( #13966 ), #29505, .F. ) ;
#29169 = CARTESIAN_POINT ( 'NONE',  ( -13.91746824999999532, 73.47500000273117848, 4.522059556121122093 ) ) ;
#29170 =( LENGTH_UNIT ( ) NAMED_UNIT ( * ) SI_UNIT ( .MILLI., .METRE. ) );
#29171 = CIRCLE ( 'NONE', #23155, 15.00000000000000000 ) ;
#29172 = CARTESIAN_POINT ( 'NONE',  ( 24.20753774853756113, 20.45052083333332504, 13.97622843553589789 ) ) ;
#29173 = EDGE_CURVE ( 'NONE', #679, #20850, #26, .T. ) ;
#29174 = CIRCLE ( 'NONE', #28103, 1.999999999999993117 ) ;
#29175 = CARTESIAN_POINT ( 'NONE',  ( 20.08610463437157279, 71.80000000546236549, -27.64615127144129758 ) ) ;
#29176 = CARTESIAN_POINT ( 'NONE',  ( -26.00068869287340334, 18.15885416666666075, 15.01150461594643382 ) ) ;
#29177 = CARTESIAN_POINT ( 'NONE',  ( -10.37757302488623701, 25.77500000273118275, 31.93888565452638417 ) ) ;
#29178 = CARTESIAN_POINT ( 'NONE',  ( -18.94512977948576093, 14.32499999726880091, 13.76444248337722698 ) ) ;
#29179 = ORIENTED_EDGE ( 'NONE', *, *, #5042, .F. ) ;
#29180 = CARTESIAN_POINT ( 'NONE',  ( -26.02091320914849959, 40.22173583425730925, 14.97647472619947528 ) ) ;
#29181 = CARTESIAN_POINT ( 'NONE',  ( 32.50000000000000711, 19.40000000546238468, 10.55989012756945122 ) ) ;
#29182 = CARTESIAN_POINT ( 'NONE',  ( -7.505752307973343918, 56.97395833333333570, -28.01184896238290989 ) ) ;
#29183 = CARTESIAN_POINT ( 'NONE',  ( -26.29305231718579350, 35.79999999999999716, -19.10302069950537884 ) ) ;
#29184 = CARTESIAN_POINT ( 'NONE',  ( 20.75514604977249178, 48.07500000273120122, 28.56700777964553950 ) ) ;
#29185 = CARTESIAN_POINT ( 'NONE',  ( 10.04305231718578817, 55.90000000546238823, -30.90933677959249337 ) ) ;
#29186 = CARTESIAN_POINT ( 'NONE',  ( -11.25946833292375793, 77.57500000273121543, 8.180482586598737171 ) ) ;
#29187 = CARTESIAN_POINT ( 'NONE',  ( -33.58253175000000113, 37.12500000273119838, 0.000000000000000000 ) ) ;
#29188 = CARTESIAN_POINT ( 'NONE',  ( -2.375766604868045029, 75.80125428700922896, -14.99999999999999822 ) ) ;
#29189 = CARTESIAN_POINT ( 'NONE',  ( -20.75514604977248823, 59.07500000273119412, -28.56700777964554305 ) ) ;
#29190 = CARTESIAN_POINT ( 'NONE',  ( 12.51014164588334232, 74.00000000000002842, 6.166118349127116538 ) ) ;
#29191 = CARTESIAN_POINT ( 'NONE',  ( 33.58253175000000823, 52.06397437591922994, 6.658888170994894828 ) ) ;
#29192 = CARTESIAN_POINT ( 'NONE',  ( 2.740863092043355209E-13, 21.02343750000000000, 30.02300923189239867 ) ) ;
#29193 = CARTESIAN_POINT ( 'NONE',  ( -20.08610463437156923, 40.30000000000001137, 27.64615127144130113 ) ) ;
#29194 = CARTESIAN_POINT ( 'NONE',  ( -18.94512977948576093, 7.824999997268822227, 13.76444248337722698 ) ) ;
#29195 = CARTESIAN_POINT ( 'NONE',  ( 6.486482029760649416E-15, 7.875000002731193049, 35.31076352940723240 ) ) ;
#29196 = CIRCLE ( 'NONE', #28095, 16.50000000000002842 ) ;
#29197 = CARTESIAN_POINT ( 'NONE',  ( 0.000000000000000000, 111.9999999999999858, 13.32050807568876927 ) ) ;
#29198 = CARTESIAN_POINT ( 'NONE',  ( 11.25946833292375793, 74.17500000273119554, 8.180482586598731842 ) ) ;
#29199 = CARTESIAN_POINT ( 'NONE',  ( -20.75514604977248823, 75.07500000273118701, -28.56700777964554305 ) ) ;
#29200 = DIRECTION ( 'NONE',  ( -0.000000000000000000, -1.000000000000000000, -0.000000000000000000 ) ) ;
#29201 = AXIS2_PLACEMENT_3D ( 'NONE', #4898, #4554, #17438 ) ;
#29202 = CARTESIAN_POINT ( 'NONE',  ( -27.16883889988623935, 65.57500000273118701, 19.73931689729374739 ) ) ;
#29203 = EDGE_LOOP ( 'NONE', ( #11092, #14034, #888, #19290 ) ) ;
#29204 = DIRECTION ( 'NONE',  ( 0.000000000000000000, 0.000000000000000000, -1.000000000000000000 ) ) ;
#29205 = CARTESIAN_POINT ( 'NONE',  ( -2.428612866367529427E-13, 63.99218749999997868, -27.95245687107222921 ) ) ;
#29206 = CARTESIAN_POINT ( 'NONE',  ( -20.75514604977248112, 55.42500000273119554, 28.56700777964554661 ) ) ;
#29207 = CARTESIAN_POINT ( 'NONE',  ( 33.58253175000000113, 12.47500000273119447, -10.91162601494193751 ) ) ;
#29208 = CARTESIAN_POINT ( 'NONE',  ( 33.58253175000000823, 6.275000002731184523, 10.91162601494192863 ) ) ;
#29209 = CARTESIAN_POINT ( 'NONE',  ( 24.20753774853731244, 40.50260416666666430, -13.97622843553633132 ) ) ;
#29210 = CARTESIAN_POINT ( 'NONE',  ( -0.04044903254990864921, 25.89881916759064140, 30.02300923189239867 ) ) ;
#29211 = CARTESIAN_POINT ( 'NONE',  ( -15.04653450569338524, 21.01784749907601579, -25.98046417659831775 ) ) ;
#29212 = CARTESIAN_POINT ( 'NONE',  ( -26.29305231718579350, 74.30000000546236549, -19.10302069950537884 ) ) ;
#29213 = CARTESIAN_POINT ( 'NONE',  ( -32.50000000000000000, 56.40000000546237402, -10.55989012756945300 ) ) ;
#29214 = CARTESIAN_POINT ( 'NONE',  ( 33.58253175000000823, 36.02500000273117564, 10.91162601494192685 ) ) ;
#29215 = CARTESIAN_POINT ( 'NONE',  ( -6.950374756619247307, 43.79128499907601935, 26.09010956794245217 ) ) ;
#29216 = CARTESIAN_POINT ( 'NONE',  ( 7.236395654485760609, 15.02499999726880731, -22.27133577429736633 ) ) ;
#29217 = CARTESIAN_POINT ( 'NONE',  ( 7.890940483122900408E-14, 10.49999999999999112, -24.50000000000000000 ) ) ;
#29218 = ORIENTED_EDGE ( 'NONE', *, *, #10945, .F. ) ;
#29219 = CARTESIAN_POINT ( 'NONE',  ( -10.37757302488623701, 47.77500000273120406, 31.93888565452638417 ) ) ;
#29220 = CARTESIAN_POINT ( 'NONE',  ( 9.270509831248421762, 77.30000000000001137, -12.75976212528059861 ) ) ;
#29221 = CARTESIAN_POINT ( 'NONE',  ( -13.94119854578936923, 47.95611083425732346, -24.22776226481241224 ) ) ;
#29222 = CARTESIAN_POINT ( 'NONE',  ( 10.37757302488624056, 70.77500000273117564, -31.93888565452638417 ) ) ;
#29223 = ORIENTED_EDGE ( 'NONE', *, *, #19113, .F. ) ;
#29224 = CARTESIAN_POINT ( 'NONE',  ( 6.486482029760649416E-15, 17.62500000273117351, 35.31076352940723240 ) ) ;
#29225 = CIRCLE ( 'NONE', #14410, 11.32050807568876749 ) ;
#29226 = CARTESIAN_POINT ( 'NONE',  ( -15.01150461594642138, 29.33072916666665719, -26.00068869287340334 ) ) ;
#29227 = ORIENTED_EDGE ( 'NONE', *, *, #8182, .F. ) ;
#29228 = CARTESIAN_POINT ( 'NONE',  ( -26.29305231718578995, 48.70000000546237118, 19.10302069950538595 ) ) ;
#29229 = CARTESIAN_POINT ( 'NONE',  ( -33.58253175000000113, 57.22500000273117848, 10.91162601494193929 ) ) ;
#29230 = CARTESIAN_POINT ( 'NONE',  ( -28.01184896238304134, 49.52604166666666430, -7.505752307972844761 ) ) ;
#29231 = CARTESIAN_POINT ( 'NONE',  ( 20.08610463437157279, 19.80000000546237260, -27.64615127144129758 ) ) ;
#29232 = CARTESIAN_POINT ( 'NONE',  ( 40.00000000000000000, 52.00000000000000711, -23.09401076758505766 ) ) ;
#29233 = CARTESIAN_POINT ( 'NONE',  ( -23.41746824999999887, 10.02499999726882507, -7.608796670333730638 ) ) ;
#29234 = EDGE_CURVE ( 'NONE', #4172, #12253, #10515, .T. ) ;
#29235 = CARTESIAN_POINT ( 'NONE',  ( 6.486482029760649416E-15, 27.87500000273120193, 35.31076352940723240 ) ) ;
#29236 = CARTESIAN_POINT ( 'NONE',  ( 0.000000000000000000, -12.99999999999999822, 0.000000000000000000 ) ) ;
#29237 = CARTESIAN_POINT ( 'NONE',  ( 26.02091320914876960, 63.70013916574268364, 14.97647472619900455 ) ) ;
#29238 = CARTESIAN_POINT ( 'NONE',  ( -5.147494310547430452, 31.55125428154683576, -32.49999999999999289 ) ) ;
#29239 = CARTESIAN_POINT ( 'NONE',  ( -20.08610463437157989, 59.70000000000000284, -27.64615127144129758 ) ) ;
#29240 = CARTESIAN_POINT ( 'NONE',  ( 10.04305231718578817, 7.400000000000003908, -30.90933677959249337 ) ) ;
#29241 = CARTESIAN_POINT ( 'NONE',  ( -19.09188309203660694, 62.70312500000000000, 19.09188309203694800 ) ) ;
#29242 = CARTESIAN_POINT ( 'NONE',  ( 14.47279130897151767, 3.424999997268800112, -19.92008829642072598 ) ) ;
#29243 = CARTESIAN_POINT ( 'NONE',  ( -4.300734207923759378, 72.47500000273119269, -13.23629886949340495 ) ) ;
#29244 = CARTESIAN_POINT ( 'NONE',  ( 26.07999730980477437, 30.33333333333332860, -6.988114217768290004 ) ) ;
#29245 = CARTESIAN_POINT ( 'NONE',  ( -33.58253175000000113, 27.22500000273119269, 10.91162601494193929 ) ) ;
#29246 = CARTESIAN_POINT ( 'NONE',  ( 33.58253175000000113, 76.22500000273119269, -10.91162601494193751 ) ) ;
#29247 = CARTESIAN_POINT ( 'NONE',  ( -10.37757302488624411, 38.97500000273117138, -31.93888565452638417 ) ) ;
#29248 = CARTESIAN_POINT ( 'NONE',  ( 6.486482029760648627E-15, 13.87500000273117706, 35.31076352940722529 ) ) ;
#29249 = CARTESIAN_POINT ( 'NONE',  ( -26.09010956794232428, 54.11496500092397355, 6.950374756619732253 ) ) ;
#29250 = CIRCLE ( 'NONE', #17183, 2.000000000000013767 ) ;
#29251 = CARTESIAN_POINT ( 'NONE',  ( 27.16883889988623935, 68.32500000273117280, -19.73931689729374384 ) ) ;
#29252 = CARTESIAN_POINT ( 'NONE',  ( 32.50000000000000000, 59.50000000546237544, -3.980102097228898626E-15 ) ) ;
#29253 = CARTESIAN_POINT ( 'NONE',  ( -32.50000000000000000, 52.10000000000001563, 10.55989012756946366 ) ) ;
#29254 = CARTESIAN_POINT ( 'NONE',  ( 4.635254915624212657, 78.85000000546239107, 14.26584774442730286 ) ) ;
#29255 = CARTESIAN_POINT ( 'NONE',  ( -10.37757302488624411, 56.72500000273117138, -31.93888565452638417 ) ) ;
#29256 = CARTESIAN_POINT ( 'NONE',  ( -7.236395654485763274, 12.52499999726880375, 22.27133577429736633 ) ) ;
#29257 = VERTEX_POINT ( 'NONE', #2789 ) ;
#29258 = CARTESIAN_POINT ( 'NONE',  ( -10.37757302488623701, 67.77500000273118985, 31.93888565452638417 ) ) ;
#29259 = CARTESIAN_POINT ( 'NONE',  ( -27.16883889988624290, 2.925000002731187543, -19.73931689729374028 ) ) ;
#29260 = CARTESIAN_POINT ( 'NONE',  ( -7.236395654485757944, 5.224999997268803043, -22.27133577429736988 ) ) ;
#29261 = CARTESIAN_POINT ( 'NONE',  ( 6.950374756619721595, 22.31809000092397000, 26.09010956794232428 ) ) ;
#29262 = ADVANCED_FACE ( 'NONE', ( #18422 ), #10855, .F. ) ;
#29263 = ORIENTED_EDGE ( 'NONE', *, *, #7038, .F. ) ;
#29264 = CARTESIAN_POINT ( 'NONE',  ( 33.58253175000000113, 36.22500000273119980, -10.91162601494193751 ) ) ;
#29265 = CARTESIAN_POINT ( 'NONE',  ( -5.147494310547430452, 42.05125428700921475, -32.49999999999999289 ) ) ;
#29266 = VERTEX_POINT ( 'NONE', #2961 ) ;
#29267 = CARTESIAN_POINT ( 'NONE',  ( -20.50609665441004736, 49.81249999999999289, -20.50609665440969565 ) ) ;
#29268 = CARTESIAN_POINT ( 'NONE',  ( -1.778240108872766143E-15, 53.50000000000000000, -32.49999999999999289 ) ) ;
#29269 = CARTESIAN_POINT ( 'NONE',  ( -24.50000000000000000, 2.899999999999995470, -7.960532557706207157 ) ) ;
#29270 = CARTESIAN_POINT ( 'NONE',  ( 5.147494310547434893, 27.05125428700921475, 32.49999999999999289 ) ) ;
#29271 = CONICAL_SURFACE ( 'NONE', #6245, 10.17814985357208890, 0.2617993877991527385 ) ;
#29272 = CARTESIAN_POINT ( 'NONE',  ( 30.02300923189239512, 16.72656249999999645, -2.619432448724977703E-13 ) ) ;
#29273 = ADVANCED_FACE ( 'NONE', ( #18755 ), #29750, .F. ) ;
#29274 = CARTESIAN_POINT ( 'NONE',  ( 7.236395654485755280, 18.22499999726881370, 22.27133577429736988 ) ) ;
#29275 = CARTESIAN_POINT ( 'NONE',  ( -27.16883889988624290, 9.175000002731191984, -19.73931689729374028 ) ) ;
#29276 = CARTESIAN_POINT ( 'NONE',  ( 10.04305231718579705, 58.59999999999998721, 30.90933677959248982 ) ) ;
#29277 = CARTESIAN_POINT ( 'NONE',  ( 13.91746824999999532, 77.97500000273119269, -4.522059556121118540 ) ) ;
#29278 = CARTESIAN_POINT ( 'NONE',  ( 9.270509831248425314, 76.95000000546237118, 12.75976212528059683 ) ) ;
#29279 = CARTESIAN_POINT ( 'NONE',  ( -7.543491769121917656, 38.34857666574267654, -28.00173670424536354 ) ) ;
#29280 = CARTESIAN_POINT ( 'NONE',  ( 11.25946833292375793, 74.57500000273120122, -8.180482586598735395 ) ) ;
#29281 = CARTESIAN_POINT ( 'NONE',  ( 26.00068869287367690, 51.38802083333332860, 15.01150461594596486 ) ) ;
#29282 = EDGE_CURVE ( 'NONE', #23148, #14306, #534, .T. ) ;
#29283 = DIRECTION ( 'NONE',  ( 0.000000000000000000, 0.000000000000000000, 1.000000000000000000 ) ) ;
#29284 = CARTESIAN_POINT ( 'NONE',  ( 20.08610463437158344, 70.70000000000000284, 27.64615127144129403 ) ) ;
#29285 = CARTESIAN_POINT ( 'NONE',  ( 24.22776226481265383, 60.26263916574269786, 13.94119854578893580 ) ) ;
#29286 = CARTESIAN_POINT ( 'NONE',  ( -20.75514604977248823, 40.82500000273120122, -28.56700777964554305 ) ) ;
#29287 = CARTESIAN_POINT ( 'NONE',  ( -15.00000000000000000, 70.35000000546234844, 4.873795443493597723 ) ) ;
#29288 = CARTESIAN_POINT ( 'NONE',  ( 27.16883889988624290, 56.17500000273119554, 19.73931689729373673 ) ) ;
#29289 = CARTESIAN_POINT ( 'NONE',  ( 20.75514604977249178, 34.07500000273117990, 28.56700777964553950 ) ) ;
#29290 = ADVANCED_FACE ( 'NONE', ( #31938 ), #21824, .F. ) ;
#29291 = DIRECTION ( 'NONE',  ( 1.000000000000000000, 0.000000000000000000, -0.000000000000000000 ) ) ;
#29292 = CARTESIAN_POINT ( 'NONE',  ( 19.09188309203661049, 26.60937499999999645, -19.09188309203694445 ) ) ;
#29293 = LINE ( 'NONE', #8695, #15240 ) ;
#29294 = PRESENTATION_LAYER_ASSIGNMENT (  '', '', ( #9540 ) ) ;
#29295 = CARTESIAN_POINT ( 'NONE',  ( -12.13525491562420910, 76.19999999999998863, 8.816778784387098611 ) ) ;
#29296 = CARTESIAN_POINT ( 'NONE',  ( -10.04305231718579172, 71.59999999999998010, -30.90933677959248982 ) ) ;
#29297 = CARTESIAN_POINT ( 'NONE',  ( 33.58253175000000113, 6.125000002731181503, -4.112674001490185761E-15 ) ) ;
#29298 = CARTESIAN_POINT ( 'NONE',  ( -14.47279130897152299, 1.924999997268818541, 19.92008829642072243 ) ) ;
#29299 = CARTESIAN_POINT ( 'NONE',  ( 0.000000000000000000, 52.00000000000000711, 0.000000000000000000 ) ) ;
#29300 = CARTESIAN_POINT ( 'NONE',  ( 19.06425588902558133, 32.04649333240934084, -19.11951029504797006 ) ) ;
#29301 = CARTESIAN_POINT ( 'NONE',  ( -1.778240108872766143E-15, 54.00000000546237544, -32.49999999999999289 ) ) ;
#29302 = CARTESIAN_POINT ( 'NONE',  ( 6.486482029760648627E-15, 21.62500000273119127, 35.31076352940722529 ) ) ;
#29303 = CARTESIAN_POINT ( 'NONE',  ( -19.09188309203694445, 53.25000000000000000, -19.09188309203661049 ) ) ;
#29304 = ORIENTED_EDGE ( 'NONE', *, *, #21531, .F. ) ;
#29305 = CARTESIAN_POINT ( 'NONE',  ( 33.58253175000000113, 58.12500000273116996, -4.112674001490185761E-15 ) ) ;
#29306 = ORIENTED_EDGE ( 'NONE', *, *, #6700, .F. ) ;
#29307 = CARTESIAN_POINT ( 'NONE',  ( -28.01184896238290278, 18.30208333333332860, 7.505752307973363457 ) ) ;
#29308 = CARTESIAN_POINT ( 'NONE',  ( 7.543491769121427382, 10.57329833425730747, -28.00173670424548433 ) ) ;
#29309 = CARTESIAN_POINT ( 'NONE',  ( -27.16883889988624290, 4.925000002731189319, -19.73931689729374028 ) ) ;
#29310 = ORIENTED_EDGE ( 'NONE', *, *, #29672, .T. ) ;
#29311 = CARTESIAN_POINT ( 'NONE',  ( 3.245314017740486554E-15, -20.99999999999998934, 26.50000000000000355 ) ) ;
#29312 = CARTESIAN_POINT ( 'NONE',  ( 33.58253175000000113, 28.47500000273118204, -10.91162601494193751 ) ) ;
#29313 = CARTESIAN_POINT ( 'NONE',  ( 32.50000000000000711, 33.40000000546238113, 10.55989012756945122 ) ) ;
#29314 =( BOUNDED_CURVE ( )  B_SPLINE_CURVE ( 2, ( #23144, #31034, #7530, #4951, #2380, #635, #19516, #13866, #29964, #16610, #29464, #32537, #14030 ),
 .UNSPECIFIED., .F., .T. ) 
 B_SPLINE_CURVE_WITH_KNOTS ( ( 3, 2, 2, 2, 2, 2, 3 ),
 ( 0.1730769230769230727, 0.1743589743589743501, 0.1769230769230769329, 0.1794871794871794879, 0.1820512820512820429, 0.1846153846153846256, 0.1858974358974359031 ),
 .UNSPECIFIED. ) 
 CURVE ( )  GEOMETRIC_REPRESENTATION_ITEM ( )  RATIONAL_B_SPLINE_CURVE ( ( 0.9755282581475768211, 0.9755282581475768211, 1.000000000000000000, 0.9510565162951535312, 1.000000000000000000, 0.9510565162951535312, 1.000000000000000000, 0.9510565162951535312, 1.000000000000000000, 0.9510565162951535312, 1.000000000000000000, 0.9755282581475768211, 0.9755282581475768211 ) ) 
 REPRESENTATION_ITEM ( '' )  );
#29315 = CARTESIAN_POINT ( 'NONE',  ( 26.29305231718579350, 78.79999999999998295, 19.10302069950537529 ) ) ;
#29316 = CARTESIAN_POINT ( 'NONE',  ( -10.04305231718578462, 54.90000000546238823, 30.90933677959249337 ) ) ;
#29317 = CARTESIAN_POINT ( 'NONE',  ( 2.375766604868043252, 73.44874571845316780, -14.99999999999999822 ) ) ;
#29318 = CARTESIAN_POINT ( 'NONE',  ( 27.16883889988624290, 44.17500000273119554, 19.73931689729373673 ) ) ;
#29319 = FILL_AREA_STYLE ('',( #18204 ) ) ;
#29320 = CARTESIAN_POINT ( 'NONE',  ( 26.29305231718579350, 22.80000000000000071, 19.10302069950537529 ) ) ;
#29321 = CARTESIAN_POINT ( 'NONE',  ( 10.04305231718578817, 19.40000000000000213, -30.90933677959249337 ) ) ;
#29322 = CARTESIAN_POINT ( 'NONE',  ( 19.82091636218621389, 14.19999999999999041, -14.40073868116559197 ) ) ;
#29323 = CARTESIAN_POINT ( 'NONE',  ( -2.162160676586881955E-15, 64.62500000273121259, -35.31076352940723240 ) ) ;
#29324 = CARTESIAN_POINT ( 'NONE',  ( -15.14183272437241889, 4.449999994537617631, -20.84094480462497856 ) ) ;
#29325 = CARTESIAN_POINT ( 'NONE',  ( 7.965081083986921939, 73.99999999999998579, -11.86478431723531912 ) ) ;
#29326 = CARTESIAN_POINT ( 'NONE',  ( -33.58253175000000113, 55.47500000273120691, 10.91162601494193929 ) ) ;
#29327 = CARTESIAN_POINT ( 'NONE',  ( 23.41746824999999887, 6.724999997268811924, -7.608796670333727974 ) ) ;
#29328 = CARTESIAN_POINT ( 'NONE',  ( -3.880418787951142701, 9.448745718453144704, 24.49999999999999645 ) ) ;
#29329 = CARTESIAN_POINT ( 'NONE',  ( -33.58253175000000113, 3.125000002731193049, 0.000000000000000000 ) ) ;
#29330 = CARTESIAN_POINT ( 'NONE',  ( 6.950374756619721595, 36.06809000092397355, 26.09010956794232428 ) ) ;
#29331 = CARTESIAN_POINT ( 'NONE',  ( 10.04305231718579705, 25.10000000546236265, 30.90933677959248982 ) ) ;
#29332 = AXIS2_PLACEMENT_3D ( 'NONE', #12323, #11978, #20577 ) ;
#29333 = CARTESIAN_POINT ( 'NONE',  ( -29.41736854754604380, 52.00000000000000000, 14.41477566699508195 ) ) ;
#29334 = CARTESIAN_POINT ( 'NONE',  ( 10.37757302488624767, 25.72500000273118914, 31.93888565452638417 ) ) ;
#29335 = CARTESIAN_POINT ( 'NONE',  ( -1.778240108872766143E-15, 18.00000000546237544, -32.49999999999999289 ) ) ;
#29336 = CYLINDRICAL_SURFACE ( 'NONE', #15558, 32.50000000000000000 ) ;
#29337 = CARTESIAN_POINT ( 'NONE',  ( 32.50000000000000000, 60.99999999999998579, -3.980102097228898626E-15 ) ) ;
#29338 = CARTESIAN_POINT ( 'NONE',  ( 30.02300923189239867, 53.10118083240936215, -0.04044903255044467877 ) ) ;
#29339 = CARTESIAN_POINT ( 'NONE',  ( 26.29305231718578995, 57.70000000546237118, -19.10302069950538240 ) ) ;
#29340 = COLOUR_RGB ( '', 0.72549020, 0.75294118, 0.79215686) ;
#29341 = CARTESIAN_POINT ( 'NONE',  ( 20.08610463437157279, 49.29999999999998295, -27.64615127144129758 ) ) ;
#29342 = CARTESIAN_POINT ( 'NONE',  ( -20.08610463437157989, 58.20000000546238539, -27.64615127144129758 ) ) ;
#29343 = CARTESIAN_POINT ( 'NONE',  ( -13.97622843553588901, 17.87239583333332149, 24.20753774853756823 ) ) ;
#29344 = CARTESIAN_POINT ( 'NONE',  ( -26.29305231718578995, 70.70000000546239960, 19.10302069950538595 ) ) ;
#29345 = CARTESIAN_POINT ( 'NONE',  ( 28.01184896238290278, 33.77083333333333570, -7.505752307973347470 ) ) ;
#29346 = CARTESIAN_POINT ( 'NONE',  ( -23.41746825000000243, 14.22499999726880837, 7.608796670333725309 ) ) ;
#29347 = ORIENTED_EDGE ( 'NONE', *, *, #30730, .F. ) ;
#29348 = CARTESIAN_POINT ( 'NONE',  ( 28.00173670424549499, 38.93267333425729504, 7.543491769121417612 ) ) ;
#29349 = VECTOR ( 'NONE', #3512, 1000.000000000000000 ) ;
#29350 = CARTESIAN_POINT ( 'NONE',  ( -20.08610463437156923, 18.80000000546237615, 27.64615127144130113 ) ) ;
#29351 = CARTESIAN_POINT ( 'NONE',  ( -2.584737979205441561E-13, 50.24218750000000711, -30.02300923189239512 ) ) ;
#29352 = DIRECTION ( 'NONE',  ( -1.000000000000000000, -1.416100796715760863E-16, 0.000000000000000000 ) ) ;
#29353 = CARTESIAN_POINT ( 'NONE',  ( -33.58253175000000113, 49.37500000273120548, 0.000000000000000000 ) ) ;
#29354 = CARTESIAN_POINT ( 'NONE',  ( 20.08610463437158344, 47.20000000546238539, 27.64615127144129403 ) ) ;
#29355 = CARTESIAN_POINT ( 'NONE',  ( -4.300734207923759378, 80.97500000273122112, -13.23629886949340495 ) ) ;
#29356 = CARTESIAN_POINT ( 'NONE',  ( -10.37757302488623701, 35.52500000273117564, 31.93888565452638417 ) ) ;
#29357 = DIRECTION ( 'NONE',  ( -0.000000000000000000, -1.000000000000000000, -0.000000000000000000 ) ) ;
#29358 = CARTESIAN_POINT ( 'NONE',  ( -10.37757302488624411, 58.97500000273120691, -31.93888565452638417 ) ) ;
#29359 = CARTESIAN_POINT ( 'NONE',  ( -32.50000000000000000, 0.5000000054623809920, 0.000000000000000000 ) ) ;
#29360 = CARTESIAN_POINT ( 'NONE',  ( -20.75514604977248112, 53.42500000273117422, 28.56700777964554661 ) ) ;
#29361 = CARTESIAN_POINT ( 'NONE',  ( 32.50000000000000000, 39.10000000000002274, -10.55989012756945833 ) ) ;
#29362 = CARTESIAN_POINT ( 'NONE',  ( 23.41746825000000243, 2.524999997268798868, 7.608796670333735079 ) ) ;
#29363 = EDGE_CURVE ( 'NONE', #16782, #26497, #33004, .T. ) ;
#29364 = CARTESIAN_POINT ( 'NONE',  ( -27.16883889988623935, 5.575000002731201221, 19.73931689729374739 ) ) ;
#29365 = CARTESIAN_POINT ( 'NONE',  ( -26.29305231718578995, 66.70000000546237118, 19.10302069950538595 ) ) ;
#29366 = CARTESIAN_POINT ( 'NONE',  ( 13.91746825000000065, 74.27500000273117564, 4.522059556121114987 ) ) ;
#29367 = CARTESIAN_POINT ( 'NONE',  ( 20.75514604977248467, 74.67500000273118133, -28.56700777964554305 ) ) ;
#29368 = CARTESIAN_POINT ( 'NONE',  ( -24.50000000000000000, 4.899999999999990585, -7.960532557706207157 ) ) ;
#29369 = ADVANCED_FACE ( 'NONE', ( #25745 ), #25405, .T. ) ;
#29370 = CARTESIAN_POINT ( 'NONE',  ( 20.75514604977249178, 68.07500000273118701, 28.56700777964553950 ) ) ;
#29371 = ORIENTED_EDGE ( 'NONE', *, *, #8471, .F. ) ;
#29372 = CARTESIAN_POINT ( 'NONE',  ( 18.94512977948575738, 16.92499999726882010, 13.76444248337723408 ) ) ;
#29373 = CARTESIAN_POINT ( 'NONE',  ( 26.09010956794232428, 11.14621500092397532, -6.950374756619718042 ) ) ;
#29374 = CARTESIAN_POINT ( 'NONE',  ( 2.445080149700053643E-15, 76.50000000000000000, 15.00000000000000000 ) ) ;
#29375 = AXIS2_PLACEMENT_3D ( 'NONE', #7935, #15332, #4679 ) ;
#29376 = CARTESIAN_POINT ( 'NONE',  ( -33.58253175000000113, 45.12500000273119127, 0.000000000000000000 ) ) ;
#29377 = CARTESIAN_POINT ( 'NONE',  ( 20.75514604977248467, 8.675000002731195536, -28.56700777964554305 ) ) ;
#29378 = CARTESIAN_POINT ( 'NONE',  ( -33.58253175000000113, 65.47500000273117848, 10.91162601494193929 ) ) ;
#29379 = CARTESIAN_POINT ( 'NONE',  ( -27.95245687107223276, 52.82031249999998579, 2.498001805406602216E-13 ) ) ;
#29380 = CARTESIAN_POINT ( 'NONE',  ( -28.00173670424549499, 33.77642333425730214, -7.543491769121417612 ) ) ;
#29381 = CARTESIAN_POINT ( 'NONE',  ( -20.47846945139866648, 30.32774333240935150, 20.53372385742108008 ) ) ;
#29382 = CARTESIAN_POINT ( 'NONE',  ( -32.50000000000000000, 72.50000000546238255, 0.000000000000000000 ) ) ;
#29383 = DIRECTION ( 'NONE',  ( 0.000000000000000000, -0.000000000000000000, 1.000000000000000000 ) ) ;
#29384 = CARTESIAN_POINT ( 'NONE',  ( 33.58253175000000113, 40.22500000273118559, -10.91162601494193574 ) ) ;
#29385 = CARTESIAN_POINT ( 'NONE',  ( 26.06988505166722803, 42.64545166574268364, -7.025853678916862854 ) ) ;
#29386 = CARTESIAN_POINT ( 'NONE',  ( -18.94512977948575738, 15.42499999726881832, -13.76444248337723231 ) ) ;
#29387 = CARTESIAN_POINT ( 'NONE',  ( 3.880418787951140036, 14.44874571845315536, -24.49999999999999645 ) ) ;
#29388 = ORIENTED_EDGE ( 'NONE', *, *, #2231, .T. ) ;
#29389 = CARTESIAN_POINT ( 'NONE',  ( 27.16883889988623935, 48.57500000273119412, -19.73931689729374384 ) ) ;
#29390 = DIRECTION ( 'NONE',  ( -0.000000000000000000, -1.000000000000000000, -0.000000000000000000 ) ) ;
#29391 = CARTESIAN_POINT ( 'NONE',  ( 27.95245687107223986, 52.53944416759064495, 0.04044903254993640479 ) ) ;
#29392 = CARTESIAN_POINT ( 'NONE',  ( 10.37757302488624767, 67.97500000273117848, 31.93888565452638417 ) ) ;
#29393 = ORIENTED_EDGE ( 'NONE', *, *, #26431, .F. ) ;
#29394 = CARTESIAN_POINT ( 'NONE',  ( -33.58253175000000113, 19.02500000273118630, -10.91162601494193218 ) ) ;
#29395 = CARTESIAN_POINT ( 'NONE',  ( -7.505752307973343918, 22.59895833333332860, -28.01184896238290989 ) ) ;
#29396 = ORIENTED_EDGE ( 'NONE', *, *, #24524, .T. ) ;
#29397 = CARTESIAN_POINT ( 'NONE',  ( -10.04305231718578462, 48.90000000546238113, 30.90933677959249337 ) ) ;
#29398 = CARTESIAN_POINT ( 'NONE',  ( -33.58253175000000113, 57.02500000273118275, -10.91162601494193218 ) ) ;
#29399 = CARTESIAN_POINT ( 'NONE',  ( 26.00068869287340334, 50.81510416666667140, -15.01150461594642316 ) ) ;
#29400 = CARTESIAN_POINT ( 'NONE',  ( -32.50000000000000000, 18.60000000546238041, 10.55989012756946366 ) ) ;
#29401 = CARTESIAN_POINT ( 'NONE',  ( 0.000000000000000000, 16.99999999999998579, 0.000000000000000000 ) ) ;
#29402 = CARTESIAN_POINT ( 'NONE',  ( -18.94512977948575738, 9.924999997268812990, -13.76444248337723231 ) ) ;
#29403 = CARTESIAN_POINT ( 'NONE',  ( 20.75514604977248467, 26.67500000273118133, -28.56700777964554305 ) ) ;
#29404 = CARTESIAN_POINT ( 'NONE',  ( -32.50000000000000000, 63.89999999999998437, -10.55989012756945300 ) ) ;
#29405 = CARTESIAN_POINT ( 'NONE',  ( -24.18731323226221974, 20.15847249907602290, 14.01125832528330406 ) ) ;
#29406 = CARTESIAN_POINT ( 'NONE',  ( -13.91746824999999532, 78.77500000273116143, -4.522059556121115875 ) ) ;
#29407 = CARTESIAN_POINT ( 'NONE',  ( -10.04305231718579172, 28.10000000546236620, -30.90933677959248982 ) ) ;
#29408 = CARTESIAN_POINT ( 'NONE',  ( -20.08610463437156923, 8.300000000000000711, 27.64615127144130113 ) ) ;
#29409 = ORIENTED_EDGE ( 'NONE', *, *, #4947, .T. ) ;
#29410 = CARTESIAN_POINT ( 'NONE',  ( -19.82091636218621034, 16.54999999453762882, -14.40073868116559552 ) ) ;
#29411 = CARTESIAN_POINT ( 'NONE',  ( 4.300734207923761154, 73.47500000273119269, 13.23629886949340495 ) ) ;
#29412 = CARTESIAN_POINT ( 'NONE',  ( 27.95245687107222921, 33.91406249999997158, -2.463307335887066074E-13 ) ) ;
#29413 =( BOUNDED_CURVE ( )  B_SPLINE_CURVE ( 2, ( #16927, #6282, #11272, #19005, #19171, #3379, #32357, #32193, #26883, #29284, #21906, #16265, #26721 ),
 .UNSPECIFIED., .F., .F. ) 
 B_SPLINE_CURVE_WITH_KNOTS ( ( 3, 2, 2, 2, 2, 2, 3 ),
 ( 0.1089743589743589758, 0.1102564102564102533, 0.1128205128205128221, 0.1153846153846153910, 0.1179487179487179460, 0.1205128205128205149, 0.1217948717948718063 ),
 .UNSPECIFIED. ) 
 CURVE ( )  GEOMETRIC_REPRESENTATION_ITEM ( )  RATIONAL_B_SPLINE_CURVE ( ( 0.9755282581475768211, 0.9755282581475768211, 1.000000000000000000, 0.9510565162951535312, 1.000000000000000000, 0.9510565162951535312, 1.000000000000000000, 0.9510565162951535312, 1.000000000000000000, 0.9510565162951535312, 1.000000000000000000, 0.9755282581475765991, 0.9755282581475767101 ) ) 
 REPRESENTATION_ITEM ( '' )  );
#29414 = CARTESIAN_POINT ( 'NONE',  ( 27.16883889988623935, 24.32500000273119056, -19.73931689729374384 ) ) ;
#29415 = CARTESIAN_POINT ( 'NONE',  ( 20.75514604977248467, 74.42500000273119554, -28.56700777964554305 ) ) ;
#29416 = CARTESIAN_POINT ( 'NONE',  ( 20.75514604977248467, 28.67500000273117777, -28.56700777964554305 ) ) ;
#29417 = CARTESIAN_POINT ( 'NONE',  ( -10.37757302488624411, 14.97500000273119269, -31.93888565452638417 ) ) ;
#29418 = CARTESIAN_POINT ( 'NONE',  ( -7.025853678916393008, 60.41704833425730214, 26.06988505166735592 ) ) ;
#29419 = CARTESIAN_POINT ( 'NONE',  ( 33.58253175000000113, 70.22500000273120691, -10.91162601494193574 ) ) ;
#29420 = LINE ( 'NONE', #16562, #29349 ) ;
#29421 = CARTESIAN_POINT ( 'NONE',  ( 2.688165632520823219E-15, 75.87500000273119838, 14.63369212191046209 ) ) ;
#29422 = CARTESIAN_POINT ( 'NONE',  ( 26.29305231718579350, 56.80000000000000426, 19.10302069950537529 ) ) ;
#29423 = CARTESIAN_POINT ( 'NONE',  ( 1.076200423132605543E-16, 66.99999999999998579, -46.18802153517007980 ) ) ;
#29424 = CARTESIAN_POINT ( 'NONE',  ( -33.58253175000000113, 55.02500000273118985, -10.91162601494193041 ) ) ;
#29425 = CARTESIAN_POINT ( 'NONE',  ( -23.41746825000000243, 12.02499999726881974, -7.608796670333730638 ) ) ;
#29426 = EDGE_LOOP ( 'NONE', ( #14267, #20599, #32962, #1199 ) ) ;
#29427 = CARTESIAN_POINT ( 'NONE',  ( 33.58253175000000823, 64.27500000273118985, 10.91162601494192863 ) ) ;
#29428 = CARTESIAN_POINT ( 'NONE',  ( -32.50000000000000000, 61.99999999999998579, 0.000000000000000000 ) ) ;
#29429 = CARTESIAN_POINT ( 'NONE',  ( 18.94512977948575738, 6.424999997268809437, 13.76444248337723408 ) ) ;
#29430 = CARTESIAN_POINT ( 'NONE',  ( 26.09010956794232428, 28.33371500092397355, -6.950374756619718042 ) ) ;
#29431 = ORIENTED_EDGE ( 'NONE', *, *, #16975, .T. ) ;
#29432 = CARTESIAN_POINT ( 'NONE',  ( 20.75514604977249178, 39.82500000273116569, 28.56700777964553950 ) ) ;
#29433 = DIRECTION ( 'NONE',  ( -0.000000000000000000, -1.000000000000000000, -0.000000000000000000 ) ) ;
#29434 = ORIENTED_EDGE ( 'NONE', *, *, #8408, .F. ) ;
#29435 = CARTESIAN_POINT ( 'NONE',  ( 7.505752307973351023, 51.81770833333332860, 28.01184896238290278 ) ) ;
#29436 = CARTESIAN_POINT ( 'NONE',  ( 32.50000000000000000, 11.50000000546236301, -3.980102097228898626E-15 ) ) ;
#29437 = CARTESIAN_POINT ( 'NONE',  ( 4.635254915624212657, 74.85000000546237686, 14.26584774442730286 ) ) ;
#29438 = CARTESIAN_POINT ( 'NONE',  ( 33.58253175000000113, 76.22500000273119269, -10.91162601494193751 ) ) ;
#29439 = CARTESIAN_POINT ( 'NONE',  ( -30.02300923189239512, 25.32031250000000000, 2.654126918244515359E-13 ) ) ;
#29440 = CARTESIAN_POINT ( 'NONE',  ( 24.50000000000000000, 6.000000000000005329, 0.000000000000000000 ) ) ;
#29441 = CARTESIAN_POINT ( 'NONE',  ( -10.37757302488623701, 9.775000002731182747, 31.93888565452638417 ) ) ;
#29442 = CARTESIAN_POINT ( 'NONE',  ( -20.75514604977248823, 14.82500000273117635, -28.56700777964554305 ) ) ;
#29443 = CARTESIAN_POINT ( 'NONE',  ( 26.29305231718579350, 57.30000000546237260, 19.10302069950537529 ) ) ;
#29444 = LINE ( 'NONE', #3536, #9350 ) ;
#29445 = CARTESIAN_POINT ( 'NONE',  ( -30.02300923189239867, 34.19493083240935505, 0.04044903255044988294 ) ) ;
#29446 = CARTESIAN_POINT ( 'NONE',  ( 4.300734207923757602, 76.77500000273118985, -13.23629886949340673 ) ) ;
#29447 = CARTESIAN_POINT ( 'NONE',  ( -7.505752307972844761, 48.66666666666666430, 28.01184896238304134 ) ) ;
#29448 = FACE_OUTER_BOUND ( 'NONE', #1913, .T. ) ;
#29449 = CARTESIAN_POINT ( 'NONE',  ( -10.04305231718578462, 38.90000000546237402, 30.90933677959249337 ) ) ;
#29450 = CARTESIAN_POINT ( 'NONE',  ( -27.95245687107223986, 65.13243083240935505, 0.04044903255043252877 ) ) ;
#29451 = CARTESIAN_POINT ( 'NONE',  ( -20.75514604977248112, 45.42500000273119554, 28.56700777964554661 ) ) ;
#29452 = CARTESIAN_POINT ( 'NONE',  ( 13.91746825000000065, 79.77500000273116143, 4.522059556121114987 ) ) ;
#29453 = CARTESIAN_POINT ( 'NONE',  ( -27.16883889988624290, 47.17500000273118843, -19.73931689729374028 ) ) ;
#29454 = CARTESIAN_POINT ( 'NONE',  ( -10.37757302488624411, 32.97500000273117848, -31.93888565452638417 ) ) ;
#29455 = CARTESIAN_POINT ( 'NONE',  ( 5.779280353836490358E-15, 66.50000000000000000, 32.49999999999999289 ) ) ;
#29456 = CARTESIAN_POINT ( 'NONE',  ( -27.95245687107223276, 21.88281249999999289, 2.498001805406602216E-13 ) ) ;
#29457 = CARTESIAN_POINT ( 'NONE',  ( 3.880418787951134707, 11.30125427608447097, 24.50000000000000000 ) ) ;
#29458 = CARTESIAN_POINT ( 'NONE',  ( 10.04305231718579705, 30.60000000000001563, 30.90933677959248982 ) ) ;
#29459 = CARTESIAN_POINT ( 'NONE',  ( -10.04305231718578462, 76.40000000000000568, 30.90933677959249337 ) ) ;
#29460 = CARTESIAN_POINT ( 'NONE',  ( -33.58253175000000113, 9.025000002731184523, -10.91162601494193218 ) ) ;
#29461 = CARTESIAN_POINT ( 'NONE',  ( -14.47279130897151767, 3.324999997268803131, -19.92008829642072598 ) ) ;
#29462 = CARTESIAN_POINT ( 'NONE',  ( 5.779280353836490358E-15, 53.00000000546238255, 32.49999999999999289 ) ) ;
#29463 = CARTESIAN_POINT ( 'NONE',  ( 13.94119854578893580, 28.46576416574268720, -24.22776226481265383 ) ) ;
#29464 = CARTESIAN_POINT ( 'NONE',  ( -10.04305231718579172, 65.60000000000000853, -30.90933677959248982 ) ) ;
#29465 = CARTESIAN_POINT ( 'NONE',  ( 10.37757302488624767, 19.72500000273119625, 31.93888565452638417 ) ) ;
#29466 = CARTESIAN_POINT ( 'NONE',  ( -24.20753774853730889, 55.97135416666665719, 13.97622843553633842 ) ) ;
#29467 = VERTEX_POINT ( 'NONE', #1883 ) ;
#29468 = CARTESIAN_POINT ( 'NONE',  ( -33.58253175000000113, 59.02500000273120406, -10.91162601494193218 ) ) ;
#29469 = ORIENTED_EDGE ( 'NONE', *, *, #13656, .T. ) ;
#29470 = CARTESIAN_POINT ( 'NONE',  ( -28.01184896238290278, 28.61458333333333215, 7.505752307973363457 ) ) ;
#29471 = CARTESIAN_POINT ( 'NONE',  ( 14.97647472619947351, 22.17486083425730925, 26.02091320914850314 ) ) ;
#29472 = CARTESIAN_POINT ( 'NONE',  ( -10.04305231718579172, 9.599999999999997868, -30.90933677959248982 ) ) ;
#29473 = CARTESIAN_POINT ( 'NONE',  ( -7.236395654485757944, 7.224999997268804819, -22.27133577429736988 ) ) ;
#29474 = CARTESIAN_POINT ( 'NONE',  ( -2.162160676586881955E-15, 30.87500000273119483, -35.31076352940723240 ) ) ;
#29475 = VECTOR ( 'NONE', #29067, 1000.000000000000000 ) ;
#29476 = CARTESIAN_POINT ( 'NONE',  ( 20.08610463437157279, 33.80000000546235839, -27.64615127144129758 ) ) ;
#29477 = CARTESIAN_POINT ( 'NONE',  ( 20.08610463437158344, 78.70000000000000284, 27.64615127144129403 ) ) ;
#29478 = CARTESIAN_POINT ( 'NONE',  ( 5.147494310547426899, 53.44874571845315359, -32.50000000000000000 ) ) ;
#29479 = LINE ( 'NONE', #3247, #6151 ) ;
#29480 = CARTESIAN_POINT ( 'NONE',  ( 33.58253175000000113, 42.47500000273119980, -10.91162601494193751 ) ) ;
#29481 = CARTESIAN_POINT ( 'NONE',  ( -32.50000000000000000, 22.00000000000000711, 0.000000000000000000 ) ) ;
#29482 = CARTESIAN_POINT ( 'NONE',  ( 32.50000000000000000, 19.10000000000000497, -10.55989012756945833 ) ) ;
#29483 = CARTESIAN_POINT ( 'NONE',  ( 15.14183272437241889, 13.70000000000000462, 20.84094480462498211 ) ) ;
#29484 = EDGE_CURVE ( 'NONE', #30610, #11703, #9985, .T. ) ;
#29485 = CARTESIAN_POINT ( 'NONE',  ( -33.58253175000000113, 65.02500000273118985, -10.91162601494193218 ) ) ;
#29486 = CARTESIAN_POINT ( 'NONE',  ( 33.58253175000000823, 52.27500000273118275, 10.91162601494192685 ) ) ;
#29487 = CARTESIAN_POINT ( 'NONE',  ( 18.94512977948576093, 10.82499999726882578, -13.76444248337722875 ) ) ;
#29488 = CARTESIAN_POINT ( 'NONE',  ( 24.50000000000000000, 4.000000000000003553, 0.000000000000000000 ) ) ;
#29489 = CARTESIAN_POINT ( 'NONE',  ( 20.75514604977248467, 2.425000002731189763, -28.56700777964554305 ) ) ;
#29490 = CARTESIAN_POINT ( 'NONE',  ( -19.11951029504763611, 36.64100666759062364, 19.06425588902592239 ) ) ;
#29491 = CARTESIAN_POINT ( 'NONE',  ( 23.37900124392997014, 16.99999999999998934, -1.544069416992833066 ) ) ;
#29492 = DIRECTION ( 'NONE',  ( 0.000000000000000000, 0.000000000000000000, 1.000000000000000000 ) ) ;
#29493 = PRODUCT_DEFINITION_CONTEXT ( 'detailed design', #7454, 'design' ) ;
#29494 = CARTESIAN_POINT ( 'NONE',  ( -10.37757302488624411, 28.72500000273118914, -31.93888565452638417 ) ) ;
#29495 = CARTESIAN_POINT ( 'NONE',  ( 5.147494310547434893, 61.05125428700922185, 32.49999999999999289 ) ) ;
#29496 = CARTESIAN_POINT ( 'NONE',  ( 24.50000000000000000, 14.09999999999999076, -7.960532557706203605 ) ) ;
#29497 = EDGE_CURVE ( 'NONE', #11025, #29752, #24023, .T. ) ;
#29498 = CARTESIAN_POINT ( 'NONE',  ( 15.04653450569339945, 53.67409749907601935, 25.98046417659831775 ) ) ;
#29499 = CARTESIAN_POINT ( 'NONE',  ( -20.08610463437157989, 46.20000000546237828, -27.64615127144129758 ) ) ;
#29500 = CARTESIAN_POINT ( 'NONE',  ( 5.779280353836490358E-15, 48.50000000000000000, 32.49999999999999289 ) ) ;
#29501 = CARTESIAN_POINT ( 'NONE',  ( 6.988114217768294445, 27.75520833333332860, 26.07999730980477437 ) ) ;
#29502 = VERTEX_POINT ( 'NONE', #30886 ) ;
#29503 = CARTESIAN_POINT ( 'NONE',  ( 10.37757302488624056, 76.52500000273120406, -31.93888565452638417 ) ) ;
#29504 = CARTESIAN_POINT ( 'NONE',  ( 26.00068869287340334, 33.62760416666665719, -15.01150461594642316 ) ) ;
#29505 =( BOUNDED_SURFACE ( )  B_SPLINE_SURFACE ( 1, 2, ( 
 ( #29562, #18632, #5573, #13642, #24430, #24272, #24106, #5742, #21530, #3002, #5908, #11387, #31978, #8475, #21864, #18962, #11225, #13475, #13804, #2828, #23940, #29406, #26999, #16385, #26339, #21701, #28904, #15882, #409, #10895, #574, #12054, #11547, #1411, #12227, #27507, #22524, #29729, #24594, #17219, #27342, #6234, #30233, #22029, #16715, #3996, #14137, #6737, #14810, #1236, #14469, #1067, #4336, #30066, #19961, #14302, #16879, #32975, #17046, #27169, #22197, #33152, #19286, #24926, #24758, #19620, #32473, #3662, #6908, #8974, #4168, #9479, #19456, #9300, #6572, #19784, #27853, #27678, #17388, #3828, #11714, #29903, #11888, #6405, #9139, #14640, #32644, #22360, #25274, #32807, #1747, #25100, #1577, #30409, #22700, #7765, #15503, #1926, #5020, #23222, #28363 ),
 ( #7245, #20827, #10008, #4506, #18251, #7598, #14980, #20480, #25786, #33681, #17910, #28698, #2275, #18076, #12575, #23562, #15679, #15331, #12749, #5195, #30931, #10180, #12917, #20662, #12403, #26128, #23046, #2625, #9828, #23393, #28525, #25450, #13088, #17561, #31102, #33504, #20304, #25957, #9656, #4850, #7424, #2451, #33855, #10349, #22873, #31271, #25622, #20136, #33331, #30755, #30581, #17733, #2102, #7077, #28018, #28190, #4678, #15157, #21657, #11187, #32102, #3294, #8431, #8600, #195, #13760, #24230, #5363, #19083, #26636, #13430, #29366, #29198, #8263, #10682, #18920, #701, #5866, #23898, #29523, #16344, #31442, #6026, #20993, #369, #21163, #16504, #5533, #15843, #26300, #29030, #13255, #3130, #13603, #26957, #3457, #23729, #26800, #16014, #8103, #13928 ) ),
 .UNSPECIFIED., .F., .F., .T. ) 
 B_SPLINE_SURFACE_WITH_KNOTS ( ( 2, 2 ),
 ( 3, 2, 2, 2, 2, 2, 2, 2, 2, 2, 2, 2, 2, 2, 2, 2, 2, 2, 2, 2, 2, 2, 2, 2, 2, 2, 2, 2, 2, 2, 2, 2, 2, 2, 2, 2, 2, 2, 2, 2, 2, 2, 2, 2, 2, 2, 2, 2, 2, 2, 3 ),
 ( 0.000000000000000000, 1.000000000000000000 ),
 ( 0.000000000000000000, 0.02000000000000000042, 0.04000000000000000083, 0.05999999999999999778, 0.08000000000000000167, 0.1000000000000000056, 0.1199999999999999956, 0.1400000000000000133, 0.1600000000000000033, 0.1799999999999999933, 0.2000000000000000111, 0.2200000000000000011, 0.2399999999999999911, 0.2600000000000000089, 0.2800000000000000266, 0.2999999999999999889, 0.3200000000000000067, 0.3400000000000000244, 0.3599999999999999867, 0.3800000000000000044, 0.4000000000000000222, 0.4199999999999999845, 0.4400000000000000022, 0.4600000000000000200, 0.4799999999999999822, 0.5000000000000000000, 0.5200000000000000178, 0.5400000000000000355, 0.5600000000000000533, 0.5799999999999999600, 0.5999999999999999778, 0.6199999999999999956, 0.6400000000000000133, 0.6600000000000000311, 0.6800000000000000488, 0.6999999999999999556, 0.7199999999999999734, 0.7399999999999999911, 0.7600000000000000089, 0.7800000000000000266, 0.8000000000000000444, 0.8199999999999999512, 0.8399999999999999689, 0.8599999999999999867, 0.8800000000000000044, 0.9000000000000000222, 0.9200000000000000400, 0.9399999999999999467, 0.9599999999999999645, 0.9799999999999999822, 1.000000000000000000 ),
 .UNSPECIFIED. ) 
 GEOMETRIC_REPRESENTATION_ITEM ( )  RATIONAL_B_SPLINE_SURFACE ( (
 ( 1.000000000000000000, 0.9510565162951535312, 1.000000000000000000, 0.9510565162951535312, 1.000000000000000000, 0.9510565162951535312, 1.000000000000000000, 0.9510565162951535312, 1.000000000000000000, 0.9510565162951535312, 1.000000000000000000, 0.9510565162951535312, 1.000000000000000000, 0.9510565162951535312, 1.000000000000000000, 0.9510565162951535312, 1.000000000000000000, 0.9510565162951535312, 1.000000000000000000, 0.9510565162951535312, 1.000000000000000000, 0.9510565162951535312, 1.000000000000000000, 0.9510565162951535312, 1.000000000000000000, 0.9510565162951535312, 1.000000000000000000, 0.9510565162951535312, 1.000000000000000000, 0.9510565162951535312, 1.000000000000000000, 0.9510565162951535312, 1.000000000000000000, 0.9510565162951535312, 1.000000000000000000, 0.9510565162951535312, 1.000000000000000000, 0.9510565162951535312, 1.000000000000000000, 0.9510565162951535312, 1.000000000000000000, 0.9510565162951535312, 1.000000000000000000, 0.9510565162951535312, 1.000000000000000000, 0.9510565162951535312, 1.000000000000000000, 0.9510565162951535312, 1.000000000000000000, 0.9510565162951535312, 1.000000000000000000, 0.9510565162951535312, 1.000000000000000000, 0.9510565162951535312, 1.000000000000000000, 0.9510565162951535312, 1.000000000000000000, 0.9510565162951535312, 1.000000000000000000, 0.9510565162951535312, 1.000000000000000000, 0.9510565162951535312, 1.000000000000000000, 0.9510565162951535312, 1.000000000000000000, 0.9510565162951535312, 1.000000000000000000, 0.9510565162951535312, 1.000000000000000000, 0.9510565162951535312, 1.000000000000000000, 0.9510565162951535312, 1.000000000000000000, 0.9510565162951535312, 1.000000000000000000, 0.9510565162951535312, 1.000000000000000000, 0.9510565162951535312, 1.000000000000000000, 0.9510565162951535312, 1.000000000000000000, 0.9510565162951535312, 1.000000000000000000, 0.9510565162951535312, 1.000000000000000000, 0.9510565162951535312, 1.000000000000000000, 0.9510565162951535312, 1.000000000000000000, 0.9510565162951535312, 1.000000000000000000, 0.9510565162951535312, 1.000000000000000000, 0.9510565162951535312, 1.000000000000000000, 0.9510565162951535312, 1.000000000000000000, 0.9510565162951535312, 1.000000000000000000, 0.9510565162951535312, 1.000000000000000000),
 ( 1.000000000000000000, 0.9510565162951535312, 1.000000000000000000, 0.9510565162951535312, 1.000000000000000000, 0.9510565162951535312, 1.000000000000000000, 0.9510565162951535312, 1.000000000000000000, 0.9510565162951535312, 1.000000000000000000, 0.9510565162951535312, 1.000000000000000000, 0.9510565162951535312, 1.000000000000000000, 0.9510565162951535312, 1.000000000000000000, 0.9510565162951535312, 1.000000000000000000, 0.9510565162951535312, 1.000000000000000000, 0.9510565162951535312, 1.000000000000000000, 0.9510565162951535312, 1.000000000000000000, 0.9510565162951535312, 1.000000000000000000, 0.9510565162951535312, 1.000000000000000000, 0.9510565162951535312, 1.000000000000000000, 0.9510565162951535312, 1.000000000000000000, 0.9510565162951535312, 1.000000000000000000, 0.9510565162951535312, 1.000000000000000000, 0.9510565162951535312, 1.000000000000000000, 0.9510565162951535312, 1.000000000000000000, 0.9510565162951535312, 1.000000000000000000, 0.9510565162951535312, 1.000000000000000000, 0.9510565162951535312, 1.000000000000000000, 0.9510565162951535312, 1.000000000000000000, 0.9510565162951535312, 1.000000000000000000, 0.9510565162951535312, 1.000000000000000000, 0.9510565162951535312, 1.000000000000000000, 0.9510565162951535312, 1.000000000000000000, 0.9510565162951535312, 1.000000000000000000, 0.9510565162951535312, 1.000000000000000000, 0.9510565162951535312, 1.000000000000000000, 0.9510565162951535312, 1.000000000000000000, 0.9510565162951535312, 1.000000000000000000, 0.9510565162951535312, 1.000000000000000000, 0.9510565162951535312, 1.000000000000000000, 0.9510565162951535312, 1.000000000000000000, 0.9510565162951535312, 1.000000000000000000, 0.9510565162951535312, 1.000000000000000000, 0.9510565162951535312, 1.000000000000000000, 0.9510565162951535312, 1.000000000000000000, 0.9510565162951535312, 1.000000000000000000, 0.9510565162951535312, 1.000000000000000000, 0.9510565162951535312, 1.000000000000000000, 0.9510565162951535312, 1.000000000000000000, 0.9510565162951535312, 1.000000000000000000, 0.9510565162951535312, 1.000000000000000000, 0.9510565162951535312, 1.000000000000000000, 0.9510565162951535312, 1.000000000000000000, 0.9510565162951535312, 1.000000000000000000, 0.9510565162951535312, 1.000000000000000000) ) ) 
 REPRESENTATION_ITEM ( '' )  SURFACE ( )  );
#29506 = CARTESIAN_POINT ( 'NONE',  ( -7.236395654485763274, 16.52499999726880731, 22.27133577429736633 ) ) ;
#29507 = VERTEX_POINT ( 'NONE', #28318 ) ;
#29508 = CARTESIAN_POINT ( 'NONE',  ( 7.468012846824777284, 46.38059000092397355, 28.02196122052045268 ) ) ;
#29509 = CARTESIAN_POINT ( 'NONE',  ( 20.08610463437157279, 15.80000000546238326, -27.64615127144129758 ) ) ;
#29510 = CARTESIAN_POINT ( 'NONE',  ( 7.505752307972854531, 53.82291666666666430, -28.01184896238303423 ) ) ;
#29511 = LINE ( 'NONE', #10838, #3690 ) ;
#29512 = CARTESIAN_POINT ( 'NONE',  ( -27.16883889988624290, 49.17500000273117422, -19.73931689729374028 ) ) ;
#29513 = CARTESIAN_POINT ( 'NONE',  ( 20.08610463437158344, 49.20000000546237828, 27.64615127144129403 ) ) ;
#29514 = CARTESIAN_POINT ( 'NONE',  ( 8.601468415847520532, 78.07500000273120122, 11.83890561707634781 ) ) ;
#29515 = CARTESIAN_POINT ( 'NONE',  ( 33.58253175000000113, 34.12500000273119127, -4.112674001490185761E-15 ) ) ;
#29516 = CARTESIAN_POINT ( 'NONE',  ( -8.446640517145639571E-15, 77.00000000546236834, 32.49999999999999289 ) ) ;
#29517 = CARTESIAN_POINT ( 'NONE',  ( -33.58253175000000113, 61.27500000273118985, -10.91162601494193218 ) ) ;
#29518 = FILL_AREA_STYLE_COLOUR ( '', #29340 ) ;
#29519 = CARTESIAN_POINT ( 'NONE',  ( 10.04305231718579705, 42.60000000000000142, 30.90933677959248982 ) ) ;
#29520 = CARTESIAN_POINT ( 'NONE',  ( 23.41746825000000243, 12.72499999726882436, -7.608796670333727974 ) ) ;
#29521 = CARTESIAN_POINT ( 'NONE',  ( -27.16883889988623935, 3.575000002731199000, 19.73931689729374739 ) ) ;
#29522 = DIRECTION ( 'NONE',  ( 0.000000000000000000, 0.000000000000000000, -1.000000000000000000 ) ) ;
#29523 = CARTESIAN_POINT ( 'NONE',  ( -13.91746824999999532, 73.47500000273117848, 4.522059556121122093 ) ) ;
#29524 = CARTESIAN_POINT ( 'NONE',  ( 27.16883889988624290, 72.17500000273119554, 19.73931689729373673 ) ) ;
#29525 = CARTESIAN_POINT ( 'NONE',  ( -24.50000000000000000, 5.000000000000004441, -3.000384657911015469E-15 ) ) ;
#29526 = CARTESIAN_POINT ( 'NONE',  ( -2.162160676586881955E-15, 68.87500000273118417, -35.31076352940723240 ) ) ;
#29527 = VERTEX_POINT ( 'NONE', #31061 ) ;
#29528 = CARTESIAN_POINT ( 'NONE',  ( -24.50000000000000000, 6.749999994537625447, -3.000384657911015469E-15 ) ) ;
#29529 = CARTESIAN_POINT ( 'NONE',  ( -24.20753774853756823, 66.85677083333334281, -13.97622843553588723 ) ) ;
#29530 = CARTESIAN_POINT ( 'NONE',  ( 0.000000000000000000, -10.99999999999999645, 0.000000000000000000 ) ) ;
#29531 = CARTESIAN_POINT ( 'NONE',  ( -2.162160676586881955E-15, 44.62500000273119838, -35.31076352940723240 ) ) ;
#29532 = CARTESIAN_POINT ( 'NONE',  ( -33.58253175000000113, 11.27500000273118630, -10.91162601494193218 ) ) ;
#29533 = CARTESIAN_POINT ( 'NONE',  ( 33.58253175000000113, 62.47500000273118559, -10.91162601494193574 ) ) ;
#29534 = CARTESIAN_POINT ( 'NONE',  ( -26.07999730980477437, 45.80208333333333570, 6.988114217768305103 ) ) ;
#29535 = CARTESIAN_POINT ( 'NONE',  ( -28.00173670424549499, 40.65142333425730214, -7.543491769121417612 ) ) ;
#29536 = CARTESIAN_POINT ( 'NONE',  ( 20.47846945139867003, 28.60899333240935150, -20.53372385742107653 ) ) ;
#29537 = CARTESIAN_POINT ( 'NONE',  ( 32.50000000000000000, 65.60000000546237686, -10.55989012756945833 ) ) ;
#29538 = FACE_OUTER_BOUND ( 'NONE', #10753, .T. ) ;
#29539 = CARTESIAN_POINT ( 'NONE',  ( -19.11951029504797006, 51.81211833240936215, -19.06425588902558133 ) ) ;
#29540 = CARTESIAN_POINT ( 'NONE',  ( 14.47279130897151589, 16.32499999726882933, 19.92008829642072953 ) ) ;
#29541 = CARTESIAN_POINT ( 'NONE',  ( 5.147494310547434893, 13.05125428700922718, 32.49999999999999289 ) ) ;
#29542 = VERTEX_POINT ( 'NONE', #7555 ) ;
#29543 = EDGE_CURVE ( 'NONE', #29467, #726, #2572, .T. ) ;
#29544 = CARTESIAN_POINT ( 'NONE',  ( -20.75514604977248823, 49.07500000273117280, -28.56700777964554305 ) ) ;
#29545 = CARTESIAN_POINT ( 'NONE',  ( 32.50000000000000000, 50.99999999999999289, -3.980102097228898626E-15 ) ) ;
#29546 = CARTESIAN_POINT ( 'NONE',  ( -19.11951029504763611, 53.82850666759064495, 19.06425588902592239 ) ) ;
#29547 = CARTESIAN_POINT ( 'NONE',  ( -2.162160676586881955E-15, 66.87500000273119838, -35.31076352940723240 ) ) ;
#29548 = EDGE_CURVE ( 'NONE', #32174, #13932, #6059, .T. ) ;
#29549 = ORIENTED_EDGE ( 'NONE', *, *, #20791, .F. ) ;
#29550 = CARTESIAN_POINT ( 'NONE',  ( -33.58253175000000113, 15.22500000273119447, 10.91162601494193929 ) ) ;
#29551 = CARTESIAN_POINT ( 'NONE',  ( -7.505752307973343918, 26.03645833333333215, -28.01184896238290989 ) ) ;
#29552 = VERTEX_POINT ( 'NONE', #31400 ) ;
#29553 = CARTESIAN_POINT ( 'NONE',  ( -1.778240108872766143E-15, 48.00000000546238255, -32.49999999999999289 ) ) ;
#29554 = CARTESIAN_POINT ( 'NONE',  ( 10.37757302488624056, 54.52500000273119696, -31.93888565452638417 ) ) ;
#29555 = CARTESIAN_POINT ( 'NONE',  ( 2.740863092043355209E-13, 62.27343749999999289, 30.02300923189239512 ) ) ;
#29556 = CARTESIAN_POINT ( 'NONE',  ( 26.29305231718579350, 19.30000000546239391, 19.10302069950537529 ) ) ;
#29557 = LINE ( 'NONE', #27336, #27822 ) ;
#29558 = CARTESIAN_POINT ( 'NONE',  ( 1.507698388325705758E-15, 11.62499999726880340, -24.62258325217400312 ) ) ;
#29559 = CARTESIAN_POINT ( 'NONE',  ( 10.37757302488624056, 20.77500000273119340, -31.93888565452638417 ) ) ;
#29560 = DIRECTION ( 'NONE',  ( 0.000000000000000000, -1.000000000000000000, 0.000000000000000000 ) ) ;
#29561 = CARTESIAN_POINT ( 'NONE',  ( 26.02091320914876960, 67.13763916574266943, 14.97647472619900455 ) ) ;
#29562 = CARTESIAN_POINT ( 'NONE',  ( -13.91746824999999887, 80.87500000273118417, 0.000000000000000000 ) ) ;
#29563 = CARTESIAN_POINT ( 'NONE',  ( -5.147494310547423346, 28.94874572391553258, 32.50000000000000000 ) ) ;
#29564 = CARTESIAN_POINT ( 'NONE',  ( -32.50000000000000000, 7.999999999999992895, 0.000000000000000000 ) ) ;
#29565 = ORIENTED_EDGE ( 'NONE', *, *, #29173, .T. ) ;
#29566 = CARTESIAN_POINT ( 'NONE',  ( 7.236395654485760609, 1.524999997268822183, -22.27133577429736633 ) ) ;
#29567 = CARTESIAN_POINT ( 'NONE',  ( 13.91746824999999887, 73.87500000273116996, -1.704398294459741270E-15 ) ) ;
#29568 = CARTESIAN_POINT ( 'NONE',  ( -6.988114217768288228, 39.78645833333332860, -26.07999730980477437 ) ) ;
#29569 = CARTESIAN_POINT ( 'NONE',  ( 10.37757302488624056, 22.52500000273119340, -31.93888565452638417 ) ) ;
#29570 = CARTESIAN_POINT ( 'NONE',  ( -27.16883889988624290, 64.92500000273119554, -19.73931689729374028 ) ) ;
#29571 = CARTESIAN_POINT ( 'NONE',  ( -33.58253175000000113, 31.27500000273118275, -10.91162601494193218 ) ) ;
#29572 = CARTESIAN_POINT ( 'NONE',  ( 27.16883889988624290, 14.17500000273118310, 19.73931689729373673 ) ) ;
#29573 = CARTESIAN_POINT ( 'NONE',  ( -33.58253175000000113, 9.475000002731199800, 10.91162601494193929 ) ) ;
#29574 = CARTESIAN_POINT ( 'NONE',  ( -0.04044903254992426173, 60.27381916759065206, 27.95245687107223276 ) ) ;
#29575 = CARTESIAN_POINT ( 'NONE',  ( 6.486482029760648627E-15, 71.62500000273118417, 35.31076352940722529 ) ) ;
#29576 = CARTESIAN_POINT ( 'NONE',  ( 26.00068869287340334, 54.25260416666666430, -15.01150461594642316 ) ) ;
#29577 = DIRECTION ( 'NONE',  ( 0.000000000000000000, 0.000000000000000000, 1.000000000000000000 ) ) ;
#29578 = CARTESIAN_POINT ( 'NONE',  ( -13.91746824999999887, 79.37500000273118417, 0.000000000000000000 ) ) ;
#29579 = CARTESIAN_POINT ( 'NONE',  ( -26.29305231718578995, 54.20000000000000995, 19.10302069950538595 ) ) ;
#29580 = CARTESIAN_POINT ( 'NONE',  ( 2.375766604868044141, 79.69874572391552192, -14.99999999999999822 ) ) ;
#29581 = CARTESIAN_POINT ( 'NONE',  ( -27.16883889988624290, 58.92500000273118133, -19.73931689729374028 ) ) ;
#29582 = CARTESIAN_POINT ( 'NONE',  ( 14.47279130897151589, 12.82499999726882400, 19.92008829642072953 ) ) ;
#29583 = EDGE_CURVE ( 'NONE', #17758, #16375, #6, .T. ) ;
#29584 = ORIENTED_EDGE ( 'NONE', *, *, #25577, .F. ) ;
#29585 = CARTESIAN_POINT ( 'NONE',  ( 6.486482029760649416E-15, 65.87500000273119838, 35.31076352940723240 ) ) ;
#29586 = CARTESIAN_POINT ( 'NONE',  ( -33.58253175000000113, 3.125000002731193049, 0.000000000000000000 ) ) ;
#29587 = CARTESIAN_POINT ( 'NONE',  ( -14.47279130897151589, 3.324999997268803131, -19.92008829642072598 ) ) ;
#29588 = CARTESIAN_POINT ( 'NONE',  ( 19.11951029504763611, 21.17225666759064850, -19.06425588902591173 ) ) ;
#29589 = EDGE_CURVE ( 'NONE', #33710, #19766, #1637, .T. ) ;
#29590 = VERTEX_POINT ( 'NONE', #28428 ) ;
#29591 = CARTESIAN_POINT ( 'NONE',  ( -33.58253175000000113, 37.12500000273118417, 0.000000000000000000 ) ) ;
#29592 = CARTESIAN_POINT ( 'NONE',  ( -10.04305231718579172, 68.10000000546237686, -30.90933677959248982 ) ) ;
#29593 = ORIENTED_EDGE ( 'NONE', *, *, #1689, .T. ) ;
#29594 = CARTESIAN_POINT ( 'NONE',  ( -7.505752307973343918, 53.53645833333332860, -28.01184896238290989 ) ) ;
#29595 = CARTESIAN_POINT ( 'NONE',  ( -26.29305231718579350, 60.30000000546238681, -19.10302069950537884 ) ) ;
#29596 = CARTESIAN_POINT ( 'NONE',  ( 2.067204126564591252E-14, 2.500000000000004885, -24.50000000000000000 ) ) ;
#29597 = CARTESIAN_POINT ( 'NONE',  ( -20.75514604977248823, 72.82500000273118701, -28.56700777964554305 ) ) ;
#29598 = CARTESIAN_POINT ( 'NONE',  ( 15.01150461594643204, 31.04947916666666075, 26.00068869287340334 ) ) ;
#29599 = CARTESIAN_POINT ( 'NONE',  ( 7.570916362186207671, 7.599999999999996092, 23.30088464923126779 ) ) ;
#29600 = CARTESIAN_POINT ( 'NONE',  ( 20.75514604977248467, 6.675000002731201754, -28.56700777964554305 ) ) ;
#29601 = CARTESIAN_POINT ( 'NONE',  ( 20.75514604977249178, 17.82500000273120122, 28.56700777964553950 ) ) ;
#29602 =( BOUNDED_CURVE ( )  B_SPLINE_CURVE ( 2, ( #24368, #30003, #32247, #21796, #6001, #32576, #14404, #26931, #11160, #9075, #16475, #3429, #3765 ),
 .UNSPECIFIED., .F., .T. ) 
 B_SPLINE_CURVE_WITH_KNOTS ( ( 3, 2, 2, 2, 2, 2, 3 ),
 ( 0.6089743589743590313, 0.6102564102564103088, 0.6128205128205128638, 0.6153846153846154188, 0.6179487179487179738, 0.6205128205128205288, 0.6217948717948718063 ),
 .UNSPECIFIED. ) 
 CURVE ( )  GEOMETRIC_REPRESENTATION_ITEM ( )  RATIONAL_B_SPLINE_CURVE ( ( 0.9755282581475768211, 0.9755282581475778203, 1.000000000000000000, 0.9510565162951535312, 1.000000000000000000, 0.9510565162951535312, 1.000000000000000000, 0.9510565162951535312, 1.000000000000000000, 0.9510565162951535312, 1.000000000000000000, 0.9755282581475768211, 0.9755282581475768211 ) ) 
 REPRESENTATION_ITEM ( '' )  );
#29603 = CARTESIAN_POINT ( 'NONE',  ( 11.25946833292375793, 75.67500000273119554, 8.180482586598731842 ) ) ;
#29604 = DIRECTION ( 'NONE',  ( -1.000000000000000000, -1.087251435804610394E-16, 0.000000000000000000 ) ) ;
#29605 = CARTESIAN_POINT ( 'NONE',  ( 28.02196122052058413, 42.93190999907601935, 7.468012846824272799 ) ) ;
#29606 = CARTESIAN_POINT ( 'NONE',  ( -9.270509831248421762, 80.29999999999999716, 12.75976212528060039 ) ) ;
#29607 = CARTESIAN_POINT ( 'NONE',  ( 20.50609665440969565, 50.67187500000000000, -20.50609665441004736 ) ) ;
#29608 = CARTESIAN_POINT ( 'NONE',  ( 32.50000000000000000, 53.60000000546238397, -10.55989012756945833 ) ) ;
#29609 = CARTESIAN_POINT ( 'NONE',  ( 13.97622843553633665, 17.29947916666666430, 24.20753774853730889 ) ) ;
#29610 = CARTESIAN_POINT ( 'NONE',  ( -33.58253175000000113, 45.22500000273117848, 10.91162601494193929 ) ) ;
#29611 = CARTESIAN_POINT ( 'NONE',  ( 13.91746824999999532, 71.97500000273117848, -4.522059556121118540 ) ) ;
#29612 = CARTESIAN_POINT ( 'NONE',  ( 27.16883889988623935, 46.57500000273119412, -19.73931689729374384 ) ) ;
#29613 = CARTESIAN_POINT ( 'NONE',  ( -27.16883889988623935, 29.57500000273119412, 19.73931689729374739 ) ) ;
#29614 = CARTESIAN_POINT ( 'NONE',  ( 24.50000000000000000, 18.00000000000001421, 0.000000000000000000 ) ) ;
#29615 = CARTESIAN_POINT ( 'NONE',  ( -19.09188309203660694, 24.89062500000000000, 19.09188309203694800 ) ) ;
#29616 = DIRECTION ( 'NONE',  ( -1.000000000000000000, 0.000000000000000000, 0.000000000000000000 ) ) ;
#29617 = CARTESIAN_POINT ( 'NONE',  ( 2.445080149700053643E-15, 76.49999999999998579, 15.00000000000000000 ) ) ;
#29618 = CARTESIAN_POINT ( 'NONE',  ( 26.29305231718578995, 73.20000000000000284, -19.10302069950538240 ) ) ;
#29619 = CARTESIAN_POINT ( 'NONE',  ( 33.58253175000000113, 12.12500000273118772, -4.112674001490185761E-15 ) ) ;
#29620 = CARTESIAN_POINT ( 'NONE',  ( -23.41746825000000243, 5.724999997268815477, 7.608796670333725309 ) ) ;
#29621 = CARTESIAN_POINT ( 'NONE',  ( 0.000000000000000000, 74.00000000000001421, 0.000000000000000000 ) ) ;
#29622 = CARTESIAN_POINT ( 'NONE',  ( 27.95245687107223276, 29.03868083240935505, -0.04044903255042905932 ) ) ;
#29623 = CARTESIAN_POINT ( 'NONE',  ( -32.50000000000000000, 60.09999999999999432, 10.55989012756946366 ) ) ;
#29624 = CARTESIAN_POINT ( 'NONE',  ( -2.162160676586882350E-15, 20.62500000273119483, -35.31076352940722529 ) ) ;
#29625 = CARTESIAN_POINT ( 'NONE',  ( -7.236395654485757944, 7.724999997268805707, -22.27133577429736988 ) ) ;
#29626 = CARTESIAN_POINT ( 'NONE',  ( -13.97622843553588901, 52.24739583333332860, 24.20753774853756823 ) ) ;
#29627 = VERTEX_POINT ( 'NONE', #20376 ) ;
#29628 = CARTESIAN_POINT ( 'NONE',  ( 10.37757302488624056, 56.52500000273118275, -31.93888565452638417 ) ) ;
#29629 = ORIENTED_EDGE ( 'NONE', *, *, #13776, .F. ) ;
#29630 = CARTESIAN_POINT ( 'NONE',  ( -26.00068869287368756, 25.60677083333332149, -15.01150461594595775 ) ) ;
#29631 = CARTESIAN_POINT ( 'NONE',  ( -0.04044903254990864921, 25.89881916759064140, 30.02300923189239867 ) ) ;
#29632 = VECTOR ( 'NONE', #32555, 1000.000000000000000 ) ;
#29633 = CARTESIAN_POINT ( 'NONE',  ( 24.50000000000000000, 15.64999999453761248, 7.960532557706212486 ) ) ;
#29634 = CARTESIAN_POINT ( 'NONE',  ( 23.41746825000000243, 4.524999997268823293, 7.608796670333735079 ) ) ;
#29635 = CARTESIAN_POINT ( 'NONE',  ( 6.486482029760649416E-15, 25.87500000273117351, 35.31076352940723240 ) ) ;
#29636 = CARTESIAN_POINT ( 'NONE',  ( -32.50000000000000000, 30.60000000546238041, 10.55989012756946366 ) ) ;
#29637 = CARTESIAN_POINT ( 'NONE',  ( 32.50000000000000000, 71.10000000000000853, -10.55989012756945833 ) ) ;
#29638 = CARTESIAN_POINT ( 'NONE',  ( 3.980102097228898626E-15, 0.000000000000000000, 32.50000000000000000 ) ) ;
#29639 = FACE_OUTER_BOUND ( 'NONE', #32748, .T. ) ;
#29640 = CARTESIAN_POINT ( 'NONE',  ( -7.543491769121417612, 56.97954833425730925, 28.00173670424549499 ) ) ;
#29641 = CARTESIAN_POINT ( 'NONE',  ( -27.16883889988624290, 41.17500000273119554, -19.73931689729374028 ) ) ;
#29642 = CARTESIAN_POINT ( 'NONE',  ( 1.507698388325705758E-15, 7.624999997268814056, -24.62258325217400312 ) ) ;
#29643 = CARTESIAN_POINT ( 'NONE',  ( -10.04305231718578462, 22.40000000000000213, 30.90933677959249337 ) ) ;
#29644 = AXIS2_PLACEMENT_3D ( 'NONE', #16860, #11693, #33126 ) ;
#29645 = CARTESIAN_POINT ( 'NONE',  ( -15.14183272437242600, 11.29999999999999361, 20.84094480462497856 ) ) ;
#29646 = CARTESIAN_POINT ( 'NONE',  ( 19.06425588902558133, 38.92149333240934794, -19.11951029504797006 ) ) ;
#29647 = CARTESIAN_POINT ( 'NONE',  ( 27.16883889988624290, 61.92500000273118133, 19.73931689729373673 ) ) ;
#29648 = CARTESIAN_POINT ( 'NONE',  ( 33.58253175000000113, 52.37500000273121259, -4.112674001490185761E-15 ) ) ;
#29649 = CARTESIAN_POINT ( 'NONE',  ( -23.41746824999999887, 9.524999997268810858, -7.608796670333730638 ) ) ;
#29650 = CARTESIAN_POINT ( 'NONE',  ( 7.570916362186213000, 4.399999999999987033, -23.30088464923126423 ) ) ;
#29651 = CARTESIAN_POINT ( 'NONE',  ( 33.58253175000000113, 8.225000002731182036, -10.91162601494193751 ) ) ;
#29652 = CARTESIAN_POINT ( 'NONE',  ( 27.95245687107223986, 42.22694416759065206, 0.04044903254993640479 ) ) ;
#29653 = CARTESIAN_POINT ( 'NONE',  ( 16.03387900638540842, 16.99999999999998224, -17.08446609624581569 ) ) ;
#29654 = CARTESIAN_POINT ( 'NONE',  ( 7.738208025867137962, 52.00000000000001421, 32.61747650539062704 ) ) ;
#29655 = CARTESIAN_POINT ( 'NONE',  ( -2.162160676586881955E-15, 26.62500000273118417, -35.31076352940723240 ) ) ;
#29656 = AXIS2_PLACEMENT_3D ( 'NONE', #110, #10431, #7680 ) ;
#29658 = AXIS2_PLACEMENT_3D ( 'NONE', #3525, #18657, #21731 ) ;
#29657 = DIRECTION ( 'NONE',  ( -0.000000000000000000, 1.000000000000000000, -0.000000000000000000 ) ) ;
#29659 = CARTESIAN_POINT ( 'NONE',  ( -1.778240108872766143E-15, 62.00000000546238255, -32.49999999999999289 ) ) ;
#29660 = CARTESIAN_POINT ( 'NONE',  ( 10.04305231718578817, 1.900000005462365582, -30.90933677959249337 ) ) ;
#29661 = CARTESIAN_POINT ( 'NONE',  ( 28.02196122052058413, 60.11940999907602645, 7.468012846824272799 ) ) ;
#29662 = CARTESIAN_POINT ( 'NONE',  ( -20.08610463437156923, 50.80000000546237970, 27.64615127144130113 ) ) ;
#29663 = CARTESIAN_POINT ( 'NONE',  ( -13.91746824999999532, 71.47500000273119269, 4.522059556121122093 ) ) ;
#29664 = CARTESIAN_POINT ( 'NONE',  ( -24.49999999999965894, 16.89999999999998437, -7.960532557706680556 ) ) ;
#29665 = CARTESIAN_POINT ( 'NONE',  ( -19.09188309203694445, 22.31250000000000000, -19.09188309203661049 ) ) ;
#29666 = CARTESIAN_POINT ( 'NONE',  ( -33.58253175000000113, 75.02500000273117564, -10.91162601494193218 ) ) ;
#29667 = CARTESIAN_POINT ( 'NONE',  ( 2.740863092043355209E-13, 34.77343750000000000, 30.02300923189239512 ) ) ;
#29668 = CARTESIAN_POINT ( 'NONE',  ( 1.093617666956751375E-13, 60.00000000546237544, -32.50000000000000711 ) ) ;
#29669 = EDGE_LOOP ( 'NONE', ( #17693, #19088, #1480, #20118 ) ) ;
#29670 = CARTESIAN_POINT ( 'NONE',  ( -15.04653450569291984, 46.81027750092398776, 25.98046417659859486 ) ) ;
#29671 = CARTESIAN_POINT ( 'NONE',  ( 26.29305231718578995, 7.700000005462379171, -19.10302069950538240 ) ) ;
#29672 = EDGE_CURVE ( 'NONE', #32174, #8211, #28260, .T. ) ;
#29673 = CARTESIAN_POINT ( 'NONE',  ( -15.01150461594595775, 59.12239583333333570, 26.00068869287368756 ) ) ;
#29674 = CARTESIAN_POINT ( 'NONE',  ( -5.147494310547423346, 46.94874572391552903, 32.50000000000000000 ) ) ;
#29675 = CARTESIAN_POINT ( 'NONE',  ( -33.58253175000000113, 47.27500000273116143, -10.91162601494193218 ) ) ;
#29676 = CARTESIAN_POINT ( 'NONE',  ( -2.092463501923844636E-15, 48.00000000546238255, -34.17252228774368916 ) ) ;
#29677 = CARTESIAN_POINT ( 'NONE',  ( -8.601468415847515203, 77.67500000273122396, 11.83890561707634959 ) ) ;
#29678 = CARTESIAN_POINT ( 'NONE',  ( -10.37757302488623701, 33.52500000273117564, 31.93888565452638417 ) ) ;
#29679 = CARTESIAN_POINT ( 'NONE',  ( 26.29305231718579350, 77.30000000546239391, 19.10302069950537529 ) ) ;
#29680 = CARTESIAN_POINT ( 'NONE',  ( 10.37757302488624056, 62.77500000273117564, -31.93888565452638417 ) ) ;
#29681 = ADVANCED_FACE ( 'NONE', ( #30649 ), #33224, .F. ) ;
#29682 = CARTESIAN_POINT ( 'NONE',  ( -10.04305231718578462, 38.39999999999999147, 30.90933677959249337 ) ) ;
#29683 = CARTESIAN_POINT ( 'NONE',  ( -23.41746825000000598, 9.724999997268804819, 7.608796670333726198 ) ) ;
#29684 = CARTESIAN_POINT ( 'NONE',  ( 6.486482029760649416E-15, 3.875000002731201931, 35.31076352940723240 ) ) ;
#29685 = CARTESIAN_POINT ( 'NONE',  ( -20.08610463437156923, 70.80000000546235128, 27.64615127144130113 ) ) ;
#29686 = CARTESIAN_POINT ( 'NONE',  ( -13.91746824999999887, 77.37500000273116996, 0.000000000000000000 ) ) ;
#29687 = CARTESIAN_POINT ( 'NONE',  ( 27.16883889988623935, 74.57500000273120122, -19.73931689729374384 ) ) ;
#29688 = CARTESIAN_POINT ( 'NONE',  ( -19.82091636218621034, 18.54999999453762882, -14.40073868116559552 ) ) ;
#29689 = ADVANCED_FACE ( 'NONE', ( #20209 ), #15398, .T. ) ;
#29690 = CARTESIAN_POINT ( 'NONE',  ( -10.37757302488624411, 66.97500000273119269, -31.93888565452638417 ) ) ;
#29691 = VERTEX_POINT ( 'NONE', #2344 ) ;
#29692 = CARTESIAN_POINT ( 'NONE',  ( -24.50000000000001066, 2.849999994537639303, 7.960532557706201828 ) ) ;
#29693 = CARTESIAN_POINT ( 'NONE',  ( 14.01125832528286352, 14.15402750092397532, -24.18731323226246843 ) ) ;
#29694 = LINE ( 'NONE', #16512, #31610 ) ;
#29695 = AXIS2_PLACEMENT_3D ( 'NONE', #27232, #32370, #6468 ) ;
#29696 = CARTESIAN_POINT ( 'NONE',  ( 6.486482029760649416E-15, 45.62500000273118417, 35.31076352940723240 ) ) ;
#29697 = CARTESIAN_POINT ( 'NONE',  ( 33.58253175000000823, 10.27500000273117564, 10.91162601494192863 ) ) ;
#29698 = CARTESIAN_POINT ( 'NONE',  ( -33.58253175000000113, 63.37500000273120548, 0.000000000000000000 ) ) ;
#29699 = CARTESIAN_POINT ( 'NONE',  ( -26.07999730980490583, 46.08854166666666430, -6.988114217767815717 ) ) ;
#29700 =( BOUNDED_CURVE ( )  B_SPLINE_CURVE ( 2, ( #406, #5570, #8300, #11063, #26506, #21699, #18792, #29404, #5906, #28734, #31480, #16383, #16052 ),
 .UNSPECIFIED., .F., .T. ) 
 B_SPLINE_CURVE_WITH_KNOTS ( ( 3, 2, 2, 2, 2, 2, 3 ),
 ( 0.1987179487179487336, 0.2000000000000000111, 0.2025641025641025661, 0.2051282051282051211, 0.2076923076923077038, 0.2102564102564102588, 0.2115384615384615363 ),
 .UNSPECIFIED. ) 
 CURVE ( )  GEOMETRIC_REPRESENTATION_ITEM ( )  RATIONAL_B_SPLINE_CURVE ( ( 0.9755282581475768211, 0.9755282581475770431, 1.000000000000000000, 0.9510565162951535312, 1.000000000000000000, 0.9510565162951535312, 1.000000000000000000, 0.9510565162951535312, 1.000000000000000000, 0.9510565162951535312, 1.000000000000000000, 0.9755282581475768211, 0.9755282581475768211 ) ) 
 REPRESENTATION_ITEM ( '' )  );
#29701 = CARTESIAN_POINT ( 'NONE',  ( -20.53372385742071771, 36.64100666759062364, 20.47846945139902530 ) ) ;
#29702 = CARTESIAN_POINT ( 'NONE',  ( 26.02091320914876960, 29.32513916574269075, 14.97647472619900455 ) ) ;
#29703 = CARTESIAN_POINT ( 'NONE',  ( -10.04305231718579172, 68.10000000546239107, -30.90933677959248982 ) ) ;
#29704 = CARTESIAN_POINT ( 'NONE',  ( 11.25946833292375793, 79.67500000273119554, 8.180482586598731842 ) ) ;
#29705 =( BOUNDED_CURVE ( )  B_SPLINE_CURVE ( 2, ( #16224, #26678, #11065, #18633, #13476, #23941, #5234, #5061, #7804, #28738, #21034, #15883, #26340 ),
 .UNSPECIFIED., .F., .T. ) 
 B_SPLINE_CURVE_WITH_KNOTS ( ( 3, 2, 2, 2, 2, 2, 3 ),
 ( 0.03205128205128205537, 0.03333333333333333287, 0.03589743589743589480, 0.03846153846153846367, 0.04102564102564102561, 0.04358974358974358754, 0.04487179487179487197 ),
 .UNSPECIFIED. ) 
 CURVE ( )  GEOMETRIC_REPRESENTATION_ITEM ( )  RATIONAL_B_SPLINE_CURVE ( ( 0.9755282581475768211, 0.9755282581475768211, 1.000000000000000000, 0.9510565162951535312, 1.000000000000000000, 0.9510565162951535312, 1.000000000000000000, 0.9510565162951535312, 1.000000000000000000, 0.9510565162951535312, 1.000000000000000000, 0.9755282581475768211, 0.9755282581475768211 ) ) 
 REPRESENTATION_ITEM ( '' )  );
#29706 = CARTESIAN_POINT ( 'NONE',  ( -26.06988505166722803, 51.23920166574269786, 7.025853678916877953 ) ) ;
#29707 = CARTESIAN_POINT ( 'NONE',  ( 23.41746824999999887, 16.62499999726882294, 0.000000000000000000 ) ) ;
#29708 = CARTESIAN_POINT ( 'NONE',  ( -15.14183272437242067, 16.69999999999999574, -20.84094480462497856 ) ) ;
#29709 = ORIENTED_EDGE ( 'NONE', *, *, #5171, .F. ) ;
#29710 = CARTESIAN_POINT ( 'NONE',  ( -33.58253175000000113, 45.47500000273119980, 10.91162601494193929 ) ) ;
#29711 = CARTESIAN_POINT ( 'NONE',  ( -20.08610463437157989, 75.69999999999998863, -27.64615127144129758 ) ) ;
#29712 = CARTESIAN_POINT ( 'NONE',  ( -24.18731323226248264, 54.54465250092398776, -14.01125832528284931 ) ) ;
#29713 = CARTESIAN_POINT ( 'NONE',  ( 20.75514604977249178, 72.07500000273120122, 28.56700777964553950 ) ) ;
#29714 = ORIENTED_EDGE ( 'NONE', *, *, #4526, .F. ) ;
#29715 = CARTESIAN_POINT ( 'NONE',  ( 6.486482029760649416E-15, 15.62500000273117884, 35.31076352940723240 ) ) ;
#29716 = CARTESIAN_POINT ( 'NONE',  ( 28.01184896238304134, 27.18229166666666430, 7.505752307972846538 ) ) ;
#29717 = ORIENTED_EDGE ( 'NONE', *, *, #24050, .F. ) ;
#29718 = AXIS2_PLACEMENT_3D ( 'NONE', #23047, #17911, #31443 ) ;
#29719 = CARTESIAN_POINT ( 'NONE',  ( 5.779280353836490358E-15, 65.00000000546236834, 32.49999999999999289 ) ) ;
#29720 = CARTESIAN_POINT ( 'NONE',  ( 20.75514604977249178, 57.82500000273118701, 28.56700777964553950 ) ) ;
#29721 = CARTESIAN_POINT ( 'NONE',  ( 7.505752307973351023, 62.13020833333334281, 28.01184896238290278 ) ) ;
#29722 = CARTESIAN_POINT ( 'NONE',  ( 32.50000000000000711, 9.400000005462381125, 10.55989012756945122 ) ) ;
#29723 = CIRCLE ( 'NONE', #14953, 24.49999999999999645 ) ;
#29724 = CYLINDRICAL_SURFACE ( 'NONE', #6991, 24.50000000000000000 ) ;
#29725 = CARTESIAN_POINT ( 'NONE',  ( 7.236395654485760609, 17.52499999726880731, -22.27133577429736633 ) ) ;
#29726 = CARTESIAN_POINT ( 'NONE',  ( -20.75514604977248823, 23.07500000273117635, -28.56700777964554305 ) ) ;
#29727 = SURFACE_STYLE_USAGE ( .BOTH. , #1409 ) ;
#29728 = CARTESIAN_POINT ( 'NONE',  ( 19.11951029504797006, 19.15586833240934794, 19.06425588902558133 ) ) ;
#29729 = CARTESIAN_POINT ( 'NONE',  ( -8.601468415847515203, 77.17500000273120975, 11.83890561707634959 ) ) ;
#29730 = DIRECTION ( 'NONE',  ( -0.000000000000000000, -1.000000000000000000, -0.000000000000000000 ) ) ;
#29731 = CARTESIAN_POINT ( 'NONE',  ( 5.147494310547643614, 15.44874571845315181, -32.49999999999992895 ) ) ;
#29732 = CARTESIAN_POINT ( 'NONE',  ( -32.50000000000000000, 10.10000000000000142, 10.55989012756946366 ) ) ;
#29733 = VERTEX_POINT ( 'NONE', #4744 ) ;
#29734 = CARTESIAN_POINT ( 'NONE',  ( 1.507698388325705758E-15, 9.624999997268808727, -24.62258325217400312 ) ) ;
#29735 = CARTESIAN_POINT ( 'NONE',  ( 11.25946833292375793, 78.07500000273121543, -8.180482586598735395 ) ) ;
#29736 = CARTESIAN_POINT ( 'NONE',  ( 13.97622843553633665, 44.79947916666667140, 24.20753774853730889 ) ) ;
#29737 = EDGE_CURVE ( 'NONE', #4339, #21971, #2357, .T. ) ;
#29738 = CARTESIAN_POINT ( 'NONE',  ( 33.58253175000000823, 16.02500000273119340, 10.91162601494192863 ) ) ;
#29739 = CARTESIAN_POINT ( 'NONE',  ( 20.75514604977249178, 69.82500000273118701, 28.56700777964553950 ) ) ;
#29740 = CARTESIAN_POINT ( 'NONE',  ( -27.16883889988624290, 31.17500000273119909, -19.73931689729374028 ) ) ;
#29741 = CARTESIAN_POINT ( 'NONE',  ( 10.37757302488624056, 16.77500000273117564, -31.93888565452638417 ) ) ;
#29742 = CARTESIAN_POINT ( 'NONE',  ( 33.58253175000000113, 6.475000002731177595, -10.91162601494193574 ) ) ;
#29743 = CARTESIAN_POINT ( 'NONE',  ( -0.04044903254992426173, 63.71131916759064495, 27.95245687107223276 ) ) ;
#29744 = CARTESIAN_POINT ( 'NONE',  ( 7.505752307973351023, 55.25520833333333570, 28.01184896238290278 ) ) ;
#29745 = CARTESIAN_POINT ( 'NONE',  ( 10.04305231718579705, 59.10000000546239107, 30.90933677959248982 ) ) ;
#29746 = CARTESIAN_POINT ( 'NONE',  ( -4.300734207923755825, 75.77500000273118985, 13.23629886949340673 ) ) ;
#29747 = CARTESIAN_POINT ( 'NONE',  ( 20.08610463437158344, 50.69999999999999574, 27.64615127144129403 ) ) ;
#29748 = DIRECTION ( 'NONE',  ( -0.8660254037844385966, 0.000000000000000000, 0.5000000000000000000 ) ) ;
#29749 = CARTESIAN_POINT ( 'NONE',  ( -2.162160676586882350E-15, 54.62500000273116996, -35.31076352940722529 ) ) ;
#29750 = CONICAL_SURFACE ( 'NONE', #12219, 10.72870458603808075, 0.8042044335707554392 ) ;
#29751 = CARTESIAN_POINT ( 'NONE',  ( 7.236395654485760609, 13.52499999726880553, -22.27133577429736633 ) ) ;
#29752 = VERTEX_POINT ( 'NONE', #17627 ) ;
#29753 = CARTESIAN_POINT ( 'NONE',  ( -33.58253175000000113, 69.47500000273116427, 10.91162601494193929 ) ) ;
#29754 = CARTESIAN_POINT ( 'NONE',  ( -1.053607264507113999E-13, 63.00000000546238255, 32.50000000000000711 ) ) ;
#29755 = CARTESIAN_POINT ( 'NONE',  ( 7.236395654485760609, 5.024999997268825069, -22.27133577429736633 ) ) ;
#29756 = CARTESIAN_POINT ( 'NONE',  ( 19.11951029504763611, 24.60975666759063785, -19.06425588902591173 ) ) ;
#29757 = ORIENTED_EDGE ( 'NONE', *, *, #1373, .F. ) ;
#29758 = CARTESIAN_POINT ( 'NONE',  ( 33.58253175000000823, 34.02500000273118275, 10.91162601494192863 ) ) ;
#29759 = CARTESIAN_POINT ( 'NONE',  ( -32.50000000000000000, 68.40000000546240244, -10.55989012756945300 ) ) ;
#29760 = VERTEX_POINT ( 'NONE', #17802 ) ;
#29761 = CARTESIAN_POINT ( 'NONE',  ( 7.505752307972854531, 50.38541666666666430, -28.01184896238303423 ) ) ;
#29762 = CARTESIAN_POINT ( 'NONE',  ( -20.75514604977248112, 59.67500000273118133, 28.56700777964554661 ) ) ;
#29763 = CARTESIAN_POINT ( 'NONE',  ( 3.445340210940985210E-14, 7.249999994537622783, 24.50000000000000000 ) ) ;
#29764 = CARTESIAN_POINT ( 'NONE',  ( 20.75514604977248467, 72.42500000273119554, -28.56700777964554305 ) ) ;
#29765 = CARTESIAN_POINT ( 'NONE',  ( -20.50609665441004736, 29.18749999999999645, -20.50609665440969565 ) ) ;
#29766 = CARTESIAN_POINT ( 'NONE',  ( -24.50000000000000355, 4.899999999999989697, -7.960532557706207157 ) ) ;
#29767 = CARTESIAN_POINT ( 'NONE',  ( 13.38408793869266766, -57.48236190979495319, 0.000000000000000000 ) ) ;
#29768 = CARTESIAN_POINT ( 'NONE',  ( 20.75514604977248467, 16.42500000273118133, -28.56700777964554305 ) ) ;
#29769 = CARTESIAN_POINT ( 'NONE',  ( -32.50000000000000000, 0.6000000054623972900, 10.55989012756946366 ) ) ;
#29770 = CARTESIAN_POINT ( 'NONE',  ( -28.00173670424535644, 47.80170166574269786, 7.543491769121936308 ) ) ;
#29771 = CARTESIAN_POINT ( 'NONE',  ( 9.270509831248423538, 81.29999999999999716, -12.75976212528059861 ) ) ;
#29772 = CIRCLE ( 'NONE', #8079, 12.11607355459420354 ) ;
#29773 = CARTESIAN_POINT ( 'NONE',  ( 28.01184896238290278, 50.95833333333332860, -7.505752307973347470 ) ) ;
#29774 = AXIS2_PLACEMENT_3D ( 'NONE', #11648, #18888, #22131 ) ;
#29775 = CARTESIAN_POINT ( 'NONE',  ( 1.555960095263670572E-15, 8.249999994537619230, -24.50000000000000000 ) ) ;
#29776 = CARTESIAN_POINT ( 'NONE',  ( -32.50000000000000000, 54.40000000546238823, -10.55989012756945300 ) ) ;
#29777 = CARTESIAN_POINT ( 'NONE',  ( 19.11951029504797006, 67.28086833240935505, 19.06425588902558133 ) ) ;
#29778 = ADVANCED_FACE ( 'NONE', ( #20553 ), #8938, .T. ) ;
#29779 = CARTESIAN_POINT ( 'NONE',  ( -20.75514604977248823, 42.82500000273119412, -28.56700777964554305 ) ) ;
#29780 = CARTESIAN_POINT ( 'NONE',  ( 13.91746825000000065, 77.77500000273114722, 4.522059556121114987 ) ) ;
#29781 = CARTESIAN_POINT ( 'NONE',  ( -27.16883889988623935, 49.57500000273120122, 19.73931689729374739 ) ) ;
#29782 = CARTESIAN_POINT ( 'NONE',  ( 20.75514604977248467, 30.67500000273119909, -28.56700777964554305 ) ) ;
#29783 = CARTESIAN_POINT ( 'NONE',  ( 11.76128613161001368, 16.99999999999998579, 20.76574261957635059 ) ) ;
#29784 = EDGE_CURVE ( 'NONE', #27962, #29096, #10249, .T. ) ;
#29785 = CARTESIAN_POINT ( 'NONE',  ( -2.428612866367529427E-13, 19.30468749999999645, -27.95245687107223276 ) ) ;
#29786 = DIRECTION ( 'NONE',  ( 0.000000000000000000, 0.000000000000000000, 1.000000000000000000 ) ) ;
#29787 = CARTESIAN_POINT ( 'NONE',  ( -12.13525491562420910, 80.19999999999998863, 8.816778784387098611 ) ) ;
#29788 = CARTESIAN_POINT ( 'NONE',  ( -2.092463501923844636E-15, 65.49999999999998579, -34.17252228774368916 ) ) ;
#29789 = CARTESIAN_POINT ( 'NONE',  ( -33.58253175000000113, 7.025000002731188964, -10.91162601494193218 ) ) ;
#29790 = CARTESIAN_POINT ( 'NONE',  ( 18.94512977948575738, 6.424999997268809437, 13.76444248337723408 ) ) ;
#29791 = CARTESIAN_POINT ( 'NONE',  ( 30.02300923189239867, 29.03868083240935505, -0.04044903255044467877 ) ) ;
#29792 = DIRECTION ( 'NONE',  ( -0.000000000000000000, 1.000000000000000000, -0.000000000000000000 ) ) ;
#29793 = CARTESIAN_POINT ( 'NONE',  ( -19.11951029504797006, 27.74961833240935505, -19.06425588902558133 ) ) ;
#29794 = CARTESIAN_POINT ( 'NONE',  ( -15.00000000000000000, 76.15000000546235981, -4.873795443493594171 ) ) ;
#29795 = CARTESIAN_POINT ( 'NONE',  ( -27.16883889988624290, 18.92500000273117422, -19.73931689729374028 ) ) ;
#29796 = CARTESIAN_POINT ( 'NONE',  ( -7.236395654485763274, 6.524999997268826846, 22.27133577429736633 ) ) ;
#29797 = VECTOR ( 'NONE', #22794, 1000.000000000000000 ) ;
#29798 = CARTESIAN_POINT ( 'NONE',  ( -6.988114217767819270, 55.54166666666667140, 26.07999730980490583 ) ) ;
#29799 = CIRCLE ( 'NONE', #754, 9.000000000000001776 ) ;
#29800 = ORIENTED_EDGE ( 'NONE', *, *, #4749, .F. ) ;
#29801 = CARTESIAN_POINT ( 'NONE',  ( 6.486482029760649416E-15, 57.62500000273119127, 35.31076352940723240 ) ) ;
#29802 = CARTESIAN_POINT ( 'NONE',  ( 33.58253175000000113, 28.37500000273117351, -4.112674001490185761E-15 ) ) ;
#29803 =( BOUNDED_CURVE ( )  B_SPLINE_CURVE ( 2, ( #14189, #31865, #8860, #26891, #29787, #3550, #11439, #18847, #14022, #22086, #32033, #21759, #21916 ),
 .UNSPECIFIED., .F., .T. ) 
 B_SPLINE_CURVE_WITH_KNOTS ( ( 3, 2, 2, 2, 2, 2, 3 ),
 ( 0.1500000000000000222, 0.1600000000000000033, 0.1799999999999999933, 0.2000000000000000111, 0.2200000000000000011, 0.2399999999999999911, 0.2500000000000000000 ),
 .UNSPECIFIED. ) 
 CURVE ( )  GEOMETRIC_REPRESENTATION_ITEM ( )  RATIONAL_B_SPLINE_CURVE ( ( 0.9755282581475768211, 0.9755282581475768211, 1.000000000000000000, 0.9510565162951535312, 1.000000000000000000, 0.9510565162951535312, 1.000000000000000000, 0.9510565162951535312, 1.000000000000000000, 0.9510565162951535312, 1.000000000000000000, 0.9755282581475768211, 0.9755282581475768211 ) ) 
 REPRESENTATION_ITEM ( '' )  );
#29804 = ORIENTED_EDGE ( 'NONE', *, *, #18195, .F. ) ;
#29805 = CARTESIAN_POINT ( 'NONE',  ( -26.00068869287340334, 21.59635416666666785, 15.01150461594643382 ) ) ;
#29806 = CARTESIAN_POINT ( 'NONE',  ( 7.543491769121427382, 20.88579833425730925, -28.00173670424548433 ) ) ;
#29807 = CARTESIAN_POINT ( 'NONE',  ( -1.778240108872766143E-15, 39.50000000000000000, -32.49999999999999289 ) ) ;
#29808 = CARTESIAN_POINT ( 'NONE',  ( -7.570916362186210335, 18.34999999453762598, -23.30088464923126779 ) ) ;
#29809 = CARTESIAN_POINT ( 'NONE',  ( 23.41746825000000243, 2.724999997268822138, -7.608796670333727974 ) ) ;
#29810 = CARTESIAN_POINT ( 'NONE',  ( 20.75514604977248467, 28.67500000273117777, -28.56700777964554305 ) ) ;
#29811 = CARTESIAN_POINT ( 'NONE',  ( -2.092463501923844636E-15, 34.00000000546236123, -34.17252228774368916 ) ) ;
#29812 = CARTESIAN_POINT ( 'NONE',  ( 26.29305231718579350, 74.80000000000001137, 19.10302069950537529 ) ) ;
#29813 = CARTESIAN_POINT ( 'NONE',  ( -26.29305231718578995, 6.700000005462392494, 19.10302069950538595 ) ) ;
#29814 = CARTESIAN_POINT ( 'NONE',  ( -24.50000000000000000, 10.90000000000000568, -7.960532557706207157 ) ) ;
#29815 = CARTESIAN_POINT ( 'NONE',  ( -26.02091320914849959, 57.40923583425731636, 14.97647472619947528 ) ) ;
#29816 = CARTESIAN_POINT ( 'NONE',  ( -20.75514604977248823, 39.07500000273119412, -28.56700777964554305 ) ) ;
#29817 = CARTESIAN_POINT ( 'NONE',  ( -26.00068869287340334, 21.59635416666666430, 15.01150461594643559 ) ) ;
#29818 = CARTESIAN_POINT ( 'NONE',  ( -23.41746825000000598, 10.22499999726881903, 7.608796670333726198 ) ) ;
#29819 = CARTESIAN_POINT ( 'NONE',  ( 6.277390505771533514E-15, 16.50000000000000000, 34.17252228774368916 ) ) ;
#29820 =( GEOMETRIC_REPRESENTATION_CONTEXT ( 3 ) GLOBAL_UNCERTAINTY_ASSIGNED_CONTEXT ( ( #11645 ) ) GLOBAL_UNIT_ASSIGNED_CONTEXT ( ( #8558, #11803, #32724 ) ) REPRESENTATION_CONTEXT ( 'NONE', 'WORKASPACE' ) );
#29821 = CARTESIAN_POINT ( 'NONE',  ( -15.14183272437241889, 10.70000000000001172, -20.84094480462497856 ) ) ;
#29822 = CARTESIAN_POINT ( 'NONE',  ( -6.950374756619247307, 43.79128499907601935, 26.09010956794245217 ) ) ;
#29823 = CARTESIAN_POINT ( 'NONE',  ( 27.16883889988624290, 65.92500000273118133, 19.73931689729373673 ) ) ;
#29824 = CARTESIAN_POINT ( 'NONE',  ( -10.37757302488624411, 46.97500000273119269, -31.93888565452638417 ) ) ;
#29825 = CARTESIAN_POINT ( 'NONE',  ( 7.236395654485760609, 9.024999997268828622, -22.27133577429736633 ) ) ;
#29826 = CARTESIAN_POINT ( 'NONE',  ( 19.82091636218621034, 3.549999994537617276, 14.40073868116559730 ) ) ;
#29827 = CARTESIAN_POINT ( 'NONE',  ( 20.75514604977249178, 5.825000002731198556, 28.56700777964553950 ) ) ;
#29828 = ADVANCED_FACE ( 'NONE', ( #28592 ), #26029, .F. ) ;
#29829 = EDGE_CURVE ( 'NONE', #22342, #16123, #13095, .T. ) ;
#29830 = CARTESIAN_POINT ( 'NONE',  ( -27.95245687107223986, 40.50819416759064495, -0.04044903254993292840 ) ) ;
#29831 = CARTESIAN_POINT ( 'NONE',  ( 3.673940397442059178E-15, 11.99999999999999645, -30.00000000000000000 ) ) ;
#29832 = CARTESIAN_POINT ( 'NONE',  ( 0.000000000000000000, 80.00000000000001421, 0.000000000000000000 ) ) ;
#29833 = UNCERTAINTY_MEASURE_WITH_UNIT (LENGTH_MEASURE( 1.000000000000000082E-05 ), #30188, 'distance_accuracy_value', 'NONE');
#29834 = CARTESIAN_POINT ( 'NONE',  ( -10.37757302488623701, 29.52500000273118630, 31.93888565452638417 ) ) ;
#29835 = CARTESIAN_POINT ( 'NONE',  ( -5.147494310547423346, 56.94874572391555034, 32.50000000000000000 ) ) ;
#29836 = FACE_OUTER_BOUND ( 'NONE', #55, .T. ) ;
#29837 = CARTESIAN_POINT ( 'NONE',  ( 28.00173670424535644, 56.39545166574268364, -7.543491769121920321 ) ) ;
#29838 = CARTESIAN_POINT ( 'NONE',  ( -32.50000000000000000, 46.60000000546237686, 10.55989012756946366 ) ) ;
#29839 = CARTESIAN_POINT ( 'NONE',  ( 26.29305231718579350, 48.80000000000001137, 19.10302069950537529 ) ) ;
#29840 = CARTESIAN_POINT ( 'NONE',  ( 6.988114217767829928, 26.32291666666666075, -26.07999730980489872 ) ) ;
#29841 = EDGE_CURVE ( 'NONE', #24826, #13703, #20472, .T. ) ;
#29842 = ORIENTED_EDGE ( 'NONE', *, *, #4845, .F. ) ;
#29843 = CARTESIAN_POINT ( 'NONE',  ( -27.16883889988623935, 77.32500000273120122, 19.73931689729374739 ) ) ;
#29844 = CARTESIAN_POINT ( 'NONE',  ( -15.01150461594595775, 31.62239583333332860, 26.00068869287368756 ) ) ;
#29845 =( BOUNDED_CURVE ( )  B_SPLINE_CURVE ( 2, ( #15598, #17826, #31196, #7686, #12664, #33599, #2546, #33780, #28615, #13013, #33425, #23484, #23133, #28788, #20399, #9922, #5287, #25710, #15769, #28283, #20578, #4770, #7520, #33945, #15247, #10437, #28449, #26224, #4940, #7855, #15422, #18343, #116, #21086, #2190, #31535, #25876, #2369, #5456, #15937, #12498, #24157, #291, #19178, #24323, #13528, #21914, #19341, #3548, #8357, #31701, #29785, #5958, #796, #21256, #13858, #32364, #8858, #11437, #11279, #29123, #3057, #8528, #14020, #3224, #5791, #16765, #16602, #27055, #29456, #26561, #11117, #21756, #8193, #24483, #32201, #23992, #16438, #18684, #627, #32031, #19013, #26890, #31863, #463, #3388, #21585, #8694, #957, #6289, #29615, #6117, #2886, #13352, #23826, #13692, #10779, #5626, #16110, #10946, #21421, #18845, #29292, #16272, #26730, #30119, #15168, #4862, #7437, #10020, #7256, #11602, #4517, #6622, #14992, #33342, #25462, #17743, #1937, #24643, #20491, #28203, #10192, #17923, #22885, #15342, #9839, #20317, #28374, #4689, #1117, #12415, #17101, #9028, #14354, #30942, #25634, #12761, #25797, #2113, #19509, #30766, #12586, #23233, #23056, #16934, #33515, #2286, #33693, #20675, #27560, #31114, #27392, #7608, #11768, #9189, #27223, #3717, #32694, #14187, #22084, #32527, #29956, #6460, #3881, #24813, #1289, #22251, #19673, #18765, #10526, #13614, #18600, #31282, #18262, #5715, #23741, #24079, #21003, #16024, #18433, #7775, #15854, #2636, #37, #5373, #26310, #23572, #16193, #31452, #26479, #5031, #2799, #7945, #23909, #28708, #31949, #26647, #20837, #29209, #28877, #5206, #5543, #15690, #13266, #2972, #21174, #13442, #2462, #29040, #544, #3141, #11032, #380, #10359, #18088, #205, #21501, #28536, #12928, #10866, #31781, #8273, #10693, #26139, #31616, #21340, #23405, #15517, #25968, #13099, #8113, #33866, #6204, #3635, #8613, #29534, #11519, #29699, #16684, #27141, #16854, #22171, #32615, #14109, #24566, #22335, #8948, #1039, #19258, #21999, #17019, #16356, #6037, #32447, #3306, #29876, #26968, #11687, #3469, #19426, #19593, #9112, #24731, #6376, #26811, #27311, #21837, #3802, #14274, #1206, #30041, #6546, #5878, #27479, #3968, #19096, #14441, #24896, #1382, #13939, #11856, #8442, #18933, #13771, #29379, #32282, #24241, #16516, #712, #11198, #21669, #32115, #24403, #879, #8775, #11359, #1549, #32780, #12025, #9274, #6709, #14612, #19758, #4137, #25068, #30207, #17191, #27649, #23773, #20866, #5407, #16057, #2493, #21371, #5576, #7806, #241, #12962, #28906, #26342, #13300, #10727, #26175, #18295, #21204, #18462, #26512, #10898, #31815, #15886, #31648, #11067, #8146, #18635, #7976, #2831, #5745, #5063, #28740, #29072, #15720, #26000, #5236, #16226, #69, #3005, #8306, #18797, #13478, #23943, #15548, #412, #10555, #29241, #26680, #3176, #13645, #24109, #28567, #577, #31147, #7638, #18120, #23436, #33897, #10388, #31312, #2669, #13128, #23602, #21036, #31486, #17580, #7268, #5040, #15002, #4355, #22543, #12594, #25297, #23065, #20683, #19981, #15352 ),
 .UNSPECIFIED., .F., .T. ) 
 B_SPLINE_CURVE_WITH_KNOTS ( ( 3, 2, 2, 2, 2, 2, 2, 2, 2, 2, 2, 2, 2, 2, 2, 2, 2, 2, 2, 2, 2, 2, 2, 2, 2, 2, 2, 2, 2, 2, 2, 2, 2, 2, 2, 2, 2, 2, 2, 2, 2, 2, 2, 2, 2, 2, 2, 2, 2, 2, 2, 2, 2, 2, 2, 2, 2, 2, 2, 2, 2, 2, 2, 2, 2, 2, 2, 2, 2, 2, 2, 2, 2, 2, 2, 2, 2, 2, 2, 2, 2, 2, 2, 2, 2, 2, 2, 2, 2, 2, 2, 2, 2, 2, 2, 2, 2, 2, 2, 2, 2, 2, 2, 2, 2, 2, 2, 2, 2, 2, 2, 2, 2, 2, 2, 2, 2, 2, 2, 2, 2, 2, 2, 2, 2, 2, 2, 2, 2, 2, 2, 2, 2, 2, 2, 2, 2, 2, 2, 2, 2, 2, 2, 2, 2, 2, 2, 2, 2, 2, 2, 2, 2, 2, 2, 2, 2, 2, 2, 2, 2, 2, 2, 2, 2, 2, 2, 2, 2, 2, 2, 2, 2, 2, 2, 2, 2, 2, 2, 2, 2, 2, 2, 2, 2, 2, 2, 2, 2, 2, 2, 2, 3 ),
 ( 0.000000000000000000, 0.005208333333333333044, 0.01041666666666666609, 0.01562500000000000000, 0.02083333333333333218, 0.02604166666666666782, 0.03125000000000000000, 0.03645833333333333565, 0.04166666666666666435, 0.04687500000000000000, 0.05208333333333333565, 0.05729166666666666435, 0.06250000000000000000, 0.06770833333333332871, 0.07291666666666667129, 0.07812500000000000000, 0.08333333333333332871, 0.08854166666666667129, 0.09375000000000000000, 0.09895833333333332871, 0.1041666666666666713, 0.1093750000000000000, 0.1145833333333333287, 0.1197916666666666713, 0.1250000000000000000, 0.1302083333333333426, 0.1354166666666666574, 0.1406250000000000000, 0.1458333333333333426, 0.1510416666666666574, 0.1562500000000000000, 0.1614583333333333426, 0.1666666666666666574, 0.1718750000000000000, 0.1770833333333333426, 0.1822916666666666574, 0.1875000000000000000, 0.1927083333333333426, 0.1979166666666666574, 0.2031250000000000000, 0.2083333333333333426, 0.2135416666666666574, 0.2187500000000000000, 0.2239583333333333426, 0.2291666666666666574, 0.2343750000000000000, 0.2395833333333333426, 0.2447916666666666574, 0.2500000000000000000, 0.2552083333333333148, 0.2604166666666666852, 0.2656250000000000000, 0.2708333333333333148, 0.2760416666666666852, 0.2812500000000000000, 0.2864583333333333148, 0.2916666666666666852, 0.2968750000000000000, 0.3020833333333333148, 0.3072916666666666852, 0.3125000000000000000, 0.3177083333333333148, 0.3229166666666666852, 0.3281250000000000000, 0.3333333333333333148, 0.3385416666666666852, 0.3437500000000000000, 0.3489583333333333148, 0.3541666666666666852, 0.3593750000000000000, 0.3645833333333333148, 0.3697916666666666852, 0.3750000000000000000, 0.3802083333333333148, 0.3854166666666666852, 0.3906250000000000000, 0.3958333333333333148, 0.4010416666666666852, 0.4062500000000000000, 0.4114583333333333148, 0.4166666666666666852, 0.4218750000000000000, 0.4270833333333333148, 0.4322916666666666852, 0.4375000000000000000, 0.4427083333333333148, 0.4479166666666666852, 0.4531250000000000000, 0.4583333333333333148, 0.4635416666666666852, 0.4687500000000000000, 0.4739583333333333148, 0.4791666666666666852, 0.4843750000000000000, 0.4895833333333333148, 0.4947916666666666852, 0.5000000000000000000, 0.5052083333333333703, 0.5104166666666666297, 0.5156250000000000000, 0.5208333333333333703, 0.5260416666666666297, 0.5312500000000000000, 0.5364583333333333703, 0.5416666666666666297, 0.5468750000000000000, 0.5520833333333333703, 0.5572916666666666297, 0.5625000000000000000, 0.5677083333333333703, 0.5729166666666666297, 0.5781250000000000000, 0.5833333333333333703, 0.5885416666666666297, 0.5937500000000000000, 0.5989583333333333703, 0.6041666666666666297, 0.6093750000000000000, 0.6145833333333333703, 0.6197916666666666297, 0.6250000000000000000, 0.6302083333333333703, 0.6354166666666666297, 0.6406250000000000000, 0.6458333333333333703, 0.6510416666666666297, 0.6562500000000000000, 0.6614583333333333703, 0.6666666666666666297, 0.6718750000000000000, 0.6770833333333333703, 0.6822916666666666297, 0.6875000000000000000, 0.6927083333333333703, 0.6979166666666666297, 0.7031250000000000000, 0.7083333333333333703, 0.7135416666666666297, 0.7187500000000000000, 0.7239583333333333703, 0.7291666666666666297, 0.7343750000000000000, 0.7395833333333333703, 0.7447916666666666297, 0.7500000000000000000, 0.7552083333333333703, 0.7604166666666666297, 0.7656250000000000000, 0.7708333333333333703, 0.7760416666666666297, 0.7812500000000000000, 0.7864583333333333703, 0.7916666666666666297, 0.7968750000000000000, 0.8020833333333333703, 0.8072916666666666297, 0.8125000000000000000, 0.8177083333333333703, 0.8229166666666666297, 0.8281250000000000000, 0.8333333333333333703, 0.8385416666666666297, 0.8437500000000000000, 0.8489583333333333703, 0.8541666666666666297, 0.8593750000000000000, 0.8645833333333333703, 0.8697916666666666297, 0.8750000000000000000, 0.8802083333333333703, 0.8854166666666666297, 0.8906250000000000000, 0.8958333333333333703, 0.9010416666666666297, 0.9062500000000000000, 0.9114583333333333703, 0.9166666666666666297, 0.9218750000000000000, 0.9270833333333333703, 0.9322916666666666297, 0.9375000000000000000, 0.9427083333333333703, 0.9479166666666666297, 0.9531250000000000000, 0.9583333333333333703, 0.9635416666666666297, 0.9687500000000000000, 0.9739583333333333703, 0.9791666666666666297, 0.9843750000000000000, 0.9895833333333333703, 0.9947916666666666297, 1.000000000000000000 ),
 .UNSPECIFIED. ) 
 CURVE ( )  GEOMETRIC_REPRESENTATION_ITEM ( )  RATIONAL_B_SPLINE_CURVE ( ( 1.000000000000000000, 0.9659258262890683122, 1.000000000000000000, 0.9659258262890683122, 1.000000000000000000, 0.9659258262890683122, 1.000000000000000000, 0.9659258262890683122, 1.000000000000000000, 0.9659258262890683122, 1.000000000000000000, 0.9659258262890683122, 1.000000000000000000, 0.9659258262890683122, 1.000000000000000000, 0.9659258262890683122, 1.000000000000000000, 0.9659258262890683122, 1.000000000000000000, 0.9659258262890683122, 1.000000000000000000, 0.9659258262890683122, 1.000000000000000000, 0.9659258262890683122, 1.000000000000000000, 0.9659258262890683122, 1.000000000000000000, 0.9659258262890683122, 1.000000000000000000, 0.9659258262890683122, 1.000000000000000000, 0.9659258262890683122, 1.000000000000000000, 0.9659258262890683122, 1.000000000000000000, 0.9659258262890683122, 1.000000000000000000, 0.9659258262890683122, 1.000000000000000000, 0.9659258262890683122, 1.000000000000000000, 0.9659258262890683122, 1.000000000000000000, 0.9659258262890683122, 1.000000000000000000, 0.9659258262890683122, 1.000000000000000000, 0.9659258262890683122, 1.000000000000000000, 0.9659258262890683122, 1.000000000000000000, 0.9659258262890683122, 1.000000000000000000, 0.9659258262890683122, 1.000000000000000000, 0.9659258262890683122, 1.000000000000000000, 0.9659258262890683122, 1.000000000000000000, 0.9659258262890683122, 1.000000000000000000, 0.9659258262890683122, 1.000000000000000000, 0.9659258262890683122, 1.000000000000000000, 0.9659258262890683122, 1.000000000000000000, 0.9659258262890683122, 1.000000000000000000, 0.9659258262890683122, 1.000000000000000000, 0.9659258262890683122, 1.000000000000000000, 0.9659258262890683122, 1.000000000000000000, 0.9659258262890683122, 1.000000000000000000, 0.9659258262890683122, 1.000000000000000000, 0.9659258262890683122, 1.000000000000000000, 0.9659258262890683122, 1.000000000000000000, 0.9659258262890683122, 1.000000000000000000, 0.9659258262890683122, 1.000000000000000000, 0.9659258262890683122, 1.000000000000000000, 0.9659258262890683122, 1.000000000000000000, 0.9659258262890683122, 1.000000000000000000, 0.9659258262890683122, 1.000000000000000000, 0.9659258262890683122, 1.000000000000000000, 0.9659258262890683122, 1.000000000000000000, 0.9659258262890683122, 1.000000000000000000, 0.9659258262890683122, 1.000000000000000000, 0.9659258262890683122, 1.000000000000000000, 0.9659258262890683122, 1.000000000000000000, 0.9659258262890683122, 1.000000000000000000, 0.9659258262890683122, 1.000000000000000000, 0.9659258262890683122, 1.000000000000000000, 0.9659258262890683122, 1.000000000000000000, 0.9659258262890683122, 1.000000000000000000, 0.9659258262890683122, 1.000000000000000000, 0.9659258262890683122, 1.000000000000000000, 0.9659258262890683122, 1.000000000000000000, 0.9659258262890683122, 1.000000000000000000, 0.9659258262890683122, 1.000000000000000000, 0.9659258262890683122, 1.000000000000000000, 0.9659258262890683122, 1.000000000000000000, 0.9659258262890683122, 1.000000000000000000, 0.9659258262890683122, 1.000000000000000000, 0.9659258262890683122, 1.000000000000000000, 0.9659258262890683122, 1.000000000000000000, 0.9659258262890683122, 1.000000000000000000, 0.9659258262890683122, 1.000000000000000000, 0.9659258262890683122, 1.000000000000000000, 0.9659258262890683122, 1.000000000000000000, 0.9659258262890683122, 1.000000000000000000, 0.9659258262890683122, 1.000000000000000000, 0.9659258262890683122, 1.000000000000000000, 0.9659258262890683122, 1.000000000000000000, 0.9659258262890683122, 1.000000000000000000, 0.9659258262890683122, 1.000000000000000000, 0.9659258262890683122, 1.000000000000000000, 0.9659258262890683122, 1.000000000000000000, 0.9659258262890683122, 1.000000000000000000, 0.9659258262890683122, 1.000000000000000000, 0.9659258262890683122, 1.000000000000000000, 0.9659258262890683122, 1.000000000000000000, 0.9659258262890683122, 1.000000000000000000, 0.9659258262890683122, 1.000000000000000000, 0.9659258262890683122, 1.000000000000000000, 0.9659258262890683122, 1.000000000000000000, 0.9659258262890683122, 1.000000000000000000, 0.9659258262890683122, 1.000000000000000000, 0.9659258262890683122, 1.000000000000000000, 0.9659258262890683122, 1.000000000000000000, 0.9659258262890683122, 1.000000000000000000, 0.9659258262890683122, 1.000000000000000000, 0.9659258262890683122, 1.000000000000000000, 0.9659258262890683122, 1.000000000000000000, 0.9659258262890683122, 1.000000000000000000, 0.9659258262890683122, 1.000000000000000000, 0.9659258262890683122, 1.000000000000000000, 0.9659258262890683122, 1.000000000000000000, 0.9659258262890683122, 1.000000000000000000, 0.9659258262890683122, 1.000000000000000000, 0.9659258262890683122, 1.000000000000000000, 0.9659258262890683122, 1.000000000000000000, 0.9659258262890683122, 1.000000000000000000, 0.9659258262890683122, 1.000000000000000000, 0.9659258262890683122, 1.000000000000000000, 0.9659258262890683122, 1.000000000000000000, 0.9659258262890683122, 1.000000000000000000, 0.9659258262890683122, 1.000000000000000000, 0.9659258262890683122, 1.000000000000000000, 0.9659258262890683122, 1.000000000000000000, 0.9659258262890683122, 1.000000000000000000, 0.9659258262890683122, 1.000000000000000000, 0.9659258262890683122, 1.000000000000000000, 0.9659258262890683122, 1.000000000000000000, 0.9659258262890683122, 1.000000000000000000, 0.9659258262890683122, 1.000000000000000000, 0.9659258262890683122, 1.000000000000000000, 0.9659258262890683122, 1.000000000000000000, 0.9659258262890683122, 1.000000000000000000, 0.9659258262890683122, 1.000000000000000000, 0.9659258262890683122, 1.000000000000000000, 0.9659258262890683122, 1.000000000000000000, 0.9659258262890683122, 1.000000000000000000, 0.9659258262890683122, 1.000000000000000000, 0.9659258262890683122, 1.000000000000000000, 0.9659258262890683122, 1.000000000000000000, 0.9659258262890683122, 1.000000000000000000, 0.9659258262890683122, 1.000000000000000000, 0.9659258262890683122, 1.000000000000000000, 0.9659258262890683122, 1.000000000000000000, 0.9659258262890683122, 1.000000000000000000, 0.9659258262890683122, 1.000000000000000000, 0.9659258262890683122, 1.000000000000000000, 0.9659258262890683122, 1.000000000000000000, 0.9659258262890683122, 1.000000000000000000, 0.9659258262890683122, 1.000000000000000000, 0.9659258262890683122, 1.000000000000000000, 0.9659258262890683122, 1.000000000000000000, 0.9659258262890683122, 1.000000000000000000, 0.9659258262890683122, 1.000000000000000000, 0.9659258262890683122, 1.000000000000000000, 0.9659258262890683122, 1.000000000000000000, 0.9659258262890683122, 1.000000000000000000, 0.9659258262890683122, 1.000000000000000000, 0.9659258262890683122, 1.000000000000000000, 0.9659258262890683122, 1.000000000000000000, 0.9659258262890683122, 1.000000000000000000, 0.9659258262890683122, 1.000000000000000000, 0.9659258262890683122, 1.000000000000000000, 0.9659258262890683122, 1.000000000000000000, 0.9659258262890683122, 1.000000000000000000, 0.9659258262890683122, 1.000000000000000000, 0.9659258262890683122, 1.000000000000000000, 0.9659258262890683122, 1.000000000000000000, 0.9659258262890683122, 1.000000000000000000, 0.9659258262890683122, 1.000000000000000000, 0.9659258262890683122, 1.000000000000000000, 0.9659258262890683122, 1.000000000000000000, 0.9659258262890683122, 1.000000000000000000, 0.9659258262890683122, 1.000000000000000000, 0.9659258262890683122, 1.000000000000000000, 0.9659258262890683122, 1.000000000000000000, 0.9659258262890683122, 1.000000000000000000, 0.9659258262890683122, 1.000000000000000000, 0.9659258262890683122, 1.000000000000000000, 0.9659258262890683122, 1.000000000000000000, 0.9659258262890683122, 1.000000000000000000, 0.9659258262890683122, 1.000000000000000000, 0.9659258262890683122, 1.000000000000000000, 0.9659258262890683122, 1.000000000000000000, 0.9659258262890683122, 1.000000000000000000, 0.9659258262890683122, 1.000000000000000000, 0.9659258262890683122, 1.000000000000000000, 0.9659258262890683122, 1.000000000000000000, 0.9659258262890683122, 1.000000000000000000, 0.9659258262890683122, 1.000000000000000000, 0.9659258262890683122, 1.000000000000000000, 0.9659258262890683122, 1.000000000000000000, 0.9659258262890683122, 1.000000000000000000, 0.9659258262890683122, 1.000000000000000000, 0.9659258262890683122, 1.000000000000000000, 0.9659258262890683122, 1.000000000000000000, 0.9659258262890683122, 1.000000000000000000, 0.9659258262890683122, 1.000000000000000000, 0.9659258262890683122, 1.000000000000000000, 0.9659258262890683122, 1.000000000000000000, 0.9659258262890683122, 1.000000000000000000, 0.9659258262890683122, 1.000000000000000000, 0.9659258262890683122, 1.000000000000000000 ) ) 
 REPRESENTATION_ITEM ( '' )  );
#29846 =( GEOMETRIC_REPRESENTATION_CONTEXT ( 3 ) GLOBAL_UNCERTAINTY_ASSIGNED_CONTEXT ( ( #3761 ) ) GLOBAL_UNIT_ASSIGNED_CONTEXT ( ( #29170, #26101, #2598 ) ) REPRESENTATION_CONTEXT ( 'NONE', 'WORKASPACE' ) );
#29847 = FACE_OUTER_BOUND ( 'NONE', #27791, .T. ) ;
#29848 = EDGE_LOOP ( 'NONE', ( #31045, #33352, #16677, #4193, #24930, #1305, #15782, #6894 ) ) ;
#29849 = CARTESIAN_POINT ( 'NONE',  ( -7.543491769121417612, 50.10454833425731636, 28.00173670424549499 ) ) ;
#29850 = CARTESIAN_POINT ( 'NONE',  ( -32.50000000000000000, 12.60000000546238219, 10.55989012756946366 ) ) ;
#29851 = CARTESIAN_POINT ( 'NONE',  ( 15.01150461594596308, 64.27864583333332860, -26.00068869287367335 ) ) ;
#29852 = CARTESIAN_POINT ( 'NONE',  ( -27.16883889988624290, 47.17500000273119554, -19.73931689729374028 ) ) ;
#29853 = CARTESIAN_POINT ( 'NONE',  ( 20.08610463437158344, 51.20000000546237828, 27.64615127144129403 ) ) ;
#29854 = CARTESIAN_POINT ( 'NONE',  ( -9.657523855033125146E-16, 81.50000000000000000, -15.77193336357400710 ) ) ;
#29855 = CARTESIAN_POINT ( 'NONE',  ( 33.58253175000000113, 36.12500000273119127, -4.112674001490185761E-15 ) ) ;
#29856 = CARTESIAN_POINT ( 'NONE',  ( -20.08610463437156923, 62.80000000546237260, 27.64615127144130113 ) ) ;
#29857 = CARTESIAN_POINT ( 'NONE',  ( 33.58253175000000823, 64.27500000273118985, 10.91162601494192863 ) ) ;
#29858 =( NAMED_UNIT ( * ) SI_UNIT ( $, .STERADIAN. ) SOLID_ANGLE_UNIT ( ) );
#29859 = CARTESIAN_POINT ( 'NONE',  ( 10.04305231718579705, 38.60000000000000853, 30.90933677959248982 ) ) ;
#29860 = CARTESIAN_POINT ( 'NONE',  ( 26.29305231718579350, 30.79999999999999361, 19.10302069950537529 ) ) ;
#29861 = CARTESIAN_POINT ( 'NONE',  ( 7.236395654485755280, 14.22499999726881192, 22.27133577429736988 ) ) ;
#29862 = CARTESIAN_POINT ( 'NONE',  ( -20.75514604977248823, 5.075000002731193227, -28.56700777964554305 ) ) ;
#29863 = DIRECTION ( 'NONE',  ( -1.224646799147353454E-16, 1.000000000000000000, -0.000000000000000000 ) ) ;
#29864 = CARTESIAN_POINT ( 'NONE',  ( 11.25946833292375793, 78.17500000273119554, 8.180482586598731842 ) ) ;
#29865 = CARTESIAN_POINT ( 'NONE',  ( -33.58253175000000113, 69.37500000273119838, 0.000000000000000000 ) ) ;
#29866 = CARTESIAN_POINT ( 'NONE',  ( -7.570916362186210335, 18.34999999453762598, -23.30088464923126779 ) ) ;
#29867 = CARTESIAN_POINT ( 'NONE',  ( 10.37757302488624767, 67.97500000273119269, 31.93888565452638417 ) ) ;
#29868 = ORIENTED_EDGE ( 'NONE', *, *, #7432, .F. ) ;
#29869 = CARTESIAN_POINT ( 'NONE',  ( 7.570916362186207671, 3.349999994537639303, 23.30088464923126779 ) ) ;
#29870 = STYLED_ITEM ( 'NONE', ( #11342 ), #11923 ) ;
#29871 = CARTESIAN_POINT ( 'NONE',  ( 14.01125832528286352, 10.71652750092397888, -24.18731323226246843 ) ) ;
#29872 = DIRECTION ( 'NONE',  ( 0.000000000000000000, -1.000000000000000000, 0.000000000000000000 ) ) ;
#29873 = CARTESIAN_POINT ( 'NONE',  ( 20.75514604977248467, 46.42500000273119554, -28.56700777964554305 ) ) ;
#29874 = CARTESIAN_POINT ( 'NONE',  ( -10.37757302488623701, 9.775000002731168536, 31.93888565452638417 ) ) ;
#29875 = CARTESIAN_POINT ( 'NONE',  ( 33.58253175000000823, 64.27500000273118985, 10.91162601494192685 ) ) ;
#29876 = CARTESIAN_POINT ( 'NONE',  ( -6.988114217767819270, 48.66666666666666430, 26.07999730980490583 ) ) ;
#29877 = CARTESIAN_POINT ( 'NONE',  ( 30.02300923189239867, 42.22694416759065206, 0.04044903254992252006 ) ) ;
#29878 = CARTESIAN_POINT ( 'NONE',  ( -7.468012846824272799, 30.04128499907601224, 28.02196122052058413 ) ) ;
#29879 = CARTESIAN_POINT ( 'NONE',  ( -26.29305231718578995, 66.70000000546237118, 19.10302069950538595 ) ) ;
#29880 = CARTESIAN_POINT ( 'NONE',  ( 13.91746824999999532, 77.97500000273122112, -4.522059556121118540 ) ) ;
#29881 = CARTESIAN_POINT ( 'NONE',  ( 24.22776226481265383, 53.38763916574269786, 13.94119854578893580 ) ) ;
#29882 = CARTESIAN_POINT ( 'NONE',  ( -10.04305231718578462, 58.40000000000000568, 30.90933677959249337 ) ) ;
#29883 = CARTESIAN_POINT ( 'NONE',  ( 5.779280353836490358E-15, 13.00000000546238077, 32.49999999999999289 ) ) ;
#29884 = ORIENTED_EDGE ( 'NONE', *, *, #30099, .F. ) ;
#29885 = CARTESIAN_POINT ( 'NONE',  ( -20.75514604977248823, 41.07500000273119412, -28.56700777964554305 ) ) ;
#29886 = CARTESIAN_POINT ( 'NONE',  ( -14.47279130897151767, 1.824999997268821783, -19.92008829642072598 ) ) ;
#29887 = CARTESIAN_POINT ( 'NONE',  ( 10.04305231718579705, 27.10000000546238041, 30.90933677959248982 ) ) ;
#29888 = VERTEX_POINT ( 'NONE', #1821 ) ;
#29889 = CARTESIAN_POINT ( 'NONE',  ( 28.01184896238304134, 37.49479166666666430, 7.505752307972846538 ) ) ;
#29890 = VERTEX_POINT ( 'NONE', #28767 ) ;
#29891 = VERTEX_POINT ( 'NONE', #5263 ) ;
#29892 = CARTESIAN_POINT ( 'NONE',  ( -32.50000000000000000, 55.99999999999999289, 0.000000000000000000 ) ) ;
#29893 = CARTESIAN_POINT ( 'NONE',  ( 10.37757302488624056, 52.52500000273118985, -31.93888565452638417 ) ) ;
#29894 = CARTESIAN_POINT ( 'NONE',  ( -7.505752307972844761, 55.54166666666667140, 28.01184896238304134 ) ) ;
#29895 = CARTESIAN_POINT ( 'NONE',  ( -26.29305231718578995, 10.70000000546239605, 19.10302069950538595 ) ) ;
#29896 = DIRECTION ( 'NONE',  ( 1.000000000000000000, 0.000000000000000000, 1.224646799147353454E-16 ) ) ;
#29897 = CARTESIAN_POINT ( 'NONE',  ( 7.236395654485755280, 12.72499999726881015, 22.27133577429736988 ) ) ;
#29898 = CARTESIAN_POINT ( 'NONE',  ( 26.29305231718579350, 58.80000000000001847, 19.10302069950537529 ) ) ;
#29899 = CARTESIAN_POINT ( 'NONE',  ( -27.16883889988624290, 21.17500000273120264, -19.73931689729374028 ) ) ;
#29900 = STYLED_ITEM ( 'NONE', ( #26997 ), #9785 ) ;
#29901 = CARTESIAN_POINT ( 'NONE',  ( -32.50000000000000000, 24.40000000546237047, -10.55989012756945300 ) ) ;
#29902 = CARTESIAN_POINT ( 'NONE',  ( -24.18731323226221974, 16.72097249907602290, 14.01125832528330406 ) ) ;
#29903 = CARTESIAN_POINT ( 'NONE',  ( -13.91746824999999532, 72.77500000273117564, -4.522059556121115875 ) ) ;
#29904 = CARTESIAN_POINT ( 'NONE',  ( 7.890940483122900408E-14, 16.49999999999999645, -24.50000000000000000 ) ) ;
#29905 = CARTESIAN_POINT ( 'NONE',  ( -1.778240108872766143E-15, 63.50000000000000000, -32.49999999999999289 ) ) ;
#29906 =( BOUNDED_CURVE ( )  B_SPLINE_CURVE ( 2, ( #25272, #30929, #7422, #28188, #4676, #1745, #15155 ),
 .UNSPECIFIED., .F., .T. ) 
 B_SPLINE_CURVE_WITH_KNOTS ( ( 3, 2, 2, 3 ),
 ( 0.000000000000000000, 0.01111111111111111154, 0.02222222222222222307, 0.02777777777777777624 ),
 .UNSPECIFIED. ) 
 CURVE ( )  GEOMETRIC_REPRESENTATION_ITEM ( )  RATIONAL_B_SPLINE_CURVE ( ( 1.000000000000000000, 0.9510565162951535312, 1.000000000000000000, 0.9510565162951535312, 1.000000000000000000, 0.9755282581475768211, 0.9755282581475768211 ) ) 
 REPRESENTATION_ITEM ( '' )  );
#29907 = CARTESIAN_POINT ( 'NONE',  ( -2.092463501923844636E-15, 11.50000000000000000, -34.17252228774368916 ) ) ;
#29908 = EDGE_LOOP ( 'NONE', ( #932, #6676, #29717, #11512 ) ) ;
#29909 = CARTESIAN_POINT ( 'NONE',  ( -7.236395654485757944, 5.724999997268803931, -22.27133577429736988 ) ) ;
#29910 = DIRECTION ( 'NONE',  ( 0.4999999999999997224, 0.000000000000000000, -0.8660254037844387076 ) ) ;
#29911 = CARTESIAN_POINT ( 'NONE',  ( 2.584737979205441561E-13, 38.21093750000000000, 27.95245687107222921 ) ) ;
#29912 = EDGE_CURVE ( 'NONE', #9084, #4172, #29225, .T. ) ;
#29913 = CARTESIAN_POINT ( 'NONE',  ( -27.16883889988623935, 17.32500000273118346, 19.73931689729374739 ) ) ;
#29914 = CARTESIAN_POINT ( 'NONE',  ( -10.37757302488624411, 64.72500000273119269, -31.93888565452638417 ) ) ;
#29915 = CARTESIAN_POINT ( 'NONE',  ( -20.75514604977248823, 33.07500000273117990, -28.56700777964554305 ) ) ;
#29916 = CARTESIAN_POINT ( 'NONE',  ( -10.37757302488623701, 17.77500000273117564, 31.93888565452638417 ) ) ;
#29917 = CARTESIAN_POINT ( 'NONE',  ( 27.16883889988624290, 12.17500000273119554, 19.73931689729373673 ) ) ;
#29918 = CARTESIAN_POINT ( 'NONE',  ( -30.02300923189239867, 13.00819416759064318, -0.04044903254991731589 ) ) ;
#29919 = CARTESIAN_POINT ( 'NONE',  ( -2.584737979205441561E-13, 57.11718750000000711, -30.02300923189239512 ) ) ;
#29920 = CARTESIAN_POINT ( 'NONE',  ( 20.08610463437158344, 3.200000005462373398, 27.64615127144129403 ) ) ;
#29921 = CARTESIAN_POINT ( 'NONE',  ( 8.601468415847516980, 78.67500000273119554, -11.83890561707634603 ) ) ;
#29922 = CARTESIAN_POINT ( 'NONE',  ( -32.50000000000000000, 47.89999999999999858, -10.55989012756945478 ) ) ;
#29923 = DIRECTION ( 'NONE',  ( 0.000000000000000000, 0.000000000000000000, 1.000000000000000000 ) ) ;
#29924 = CARTESIAN_POINT ( 'NONE',  ( -27.16883889988623935, 49.32500000273118701, 19.73931689729374739 ) ) ;
#29925 = CARTESIAN_POINT ( 'NONE',  ( 23.41746825000000243, 4.524999997268823293, 7.608796670333735079 ) ) ;
#29926 = ORIENTED_EDGE ( 'NONE', *, *, #17205, .F. ) ;
#29927 = CARTESIAN_POINT ( 'NONE',  ( -27.16883889988623935, 63.57500000273117990, 19.73931689729374739 ) ) ;
#29928 = CARTESIAN_POINT ( 'NONE',  ( 32.50000000000000000, 17.10000000000001208, -10.55989012756945833 ) ) ;
#29929 = CARTESIAN_POINT ( 'NONE',  ( -4.523095164977116484E-15, 8.124999997268826490, 24.62258325217400312 ) ) ;
#29930 = CARTESIAN_POINT ( 'NONE',  ( 7.025853678916403666, 24.32329833425730214, -26.06988505166735237 ) ) ;
#29931 = ORIENTED_EDGE ( 'NONE', *, *, #10511, .T. ) ;
#29932 = CARTESIAN_POINT ( 'NONE',  ( -33.58253175000000113, 37.02500000273117564, -10.91162601494193218 ) ) ;
#29933 = CARTESIAN_POINT ( 'NONE',  ( 3.469446951953614189E-15, -57.99999999999999289, 0.000000000000000000 ) ) ;
#29934 = ORIENTED_EDGE ( 'NONE', *, *, #2724, .T. ) ;
#29935 = CARTESIAN_POINT ( 'NONE',  ( -30.02300923189239512, 52.82031249999997868, 2.654126918244515359E-13 ) ) ;
#29936 = CARTESIAN_POINT ( 'NONE',  ( 20.75514604977249178, 58.07500000273117990, 28.56700777964553950 ) ) ;
#29937 = CARTESIAN_POINT ( 'NONE',  ( 32.50000000000000000, 58.99999999999998579, -3.980102097228898626E-15 ) ) ;
#29938 = CARTESIAN_POINT ( 'NONE',  ( -33.58253175000000113, 73.22500000273117848, 10.91162601494193929 ) ) ;
#29939 = CARTESIAN_POINT ( 'NONE',  ( 7.505752307973351023, 27.75520833333332860, 28.01184896238290278 ) ) ;
#29940 = CARTESIAN_POINT ( 'NONE',  ( -15.14183272437242600, 3.300000000000012257, 20.84094480462497856 ) ) ;
#29941 = CARTESIAN_POINT ( 'NONE',  ( -10.37757302488623701, 1.775000002731175197, 31.93888565452638417 ) ) ;
#29942 = CARTESIAN_POINT ( 'NONE',  ( -27.16883889988623935, 17.32500000273118346, 19.73931689729374739 ) ) ;
#29943 = CARTESIAN_POINT ( 'NONE',  ( -20.08610463437156923, 0.8000000054623617185, 27.64615127144130113 ) ) ;
#29944 = CARTESIAN_POINT ( 'NONE',  ( 14.97647472619900455, 42.21576416574269075, -26.02091320914876960 ) ) ;
#29945 = CARTESIAN_POINT ( 'NONE',  ( -12.13525491562420910, 78.19999999999998863, 8.816778784387098611 ) ) ;
#29946 = CARTESIAN_POINT ( 'NONE',  ( -20.50609665441004736, 56.68749999999998579, -20.50609665440969565 ) ) ;
#29947 = CARTESIAN_POINT ( 'NONE',  ( 10.04305231718578817, 53.90000000546239534, -30.90933677959249337 ) ) ;
#29948 = CARTESIAN_POINT ( 'NONE',  ( -7.570916362186215665, 7.149999994537637349, 23.30088464923126423 ) ) ;
#29949 = CARTESIAN_POINT ( 'NONE',  ( -5.147494310547430452, 38.05125428700922185, -32.49999999999999289 ) ) ;
#29950 = CARTESIAN_POINT ( 'NONE',  ( -26.09010956794245217, 68.71315999907601224, -6.950374756619243755 ) ) ;
#29951 = CARTESIAN_POINT ( 'NONE',  ( 33.58253175000000113, 36.12500000273119127, -4.112674001490185761E-15 ) ) ;
#29952 = CARTESIAN_POINT ( 'NONE',  ( -8.960552108402742093E-16, 74.37500000273121259, -14.63369212191046387 ) ) ;
#29953 = CARTESIAN_POINT ( 'NONE',  ( -10.37757302488623701, 49.77500000273120406, 31.93888565452638417 ) ) ;
#29954 = CARTESIAN_POINT ( 'NONE',  ( -27.16883889988624290, 25.17500000273117777, -19.73931689729374028 ) ) ;
#29955 = CARTESIAN_POINT ( 'NONE',  ( 21.46812038053990079, 16.99999999999998934, 9.396489787187540799 ) ) ;
#29956 = CARTESIAN_POINT ( 'NONE',  ( -19.09188309203660694, 35.20312500000000000, 19.09188309203694800 ) ) ;
#29957 = CARTESIAN_POINT ( 'NONE',  ( 15.14183272437242067, 1.700000000000004396, 20.84094480462498211 ) ) ;
#29958 = CARTESIAN_POINT ( 'NONE',  ( -8.891200544363830713E-16, 75.50000000000001421, -15.00000000000000000 ) ) ;
#29959 = CARTESIAN_POINT ( 'NONE',  ( 32.50000000000000000, 66.99999999999998579, -3.980102097228898626E-15 ) ) ;
#29960 = CARTESIAN_POINT ( 'NONE',  ( -23.41746825000000243, 13.72499999726882258, 7.608796670333725309 ) ) ;
#29961 = CARTESIAN_POINT ( 'NONE',  ( 7.468012846824281681, 21.44753499907601579, -28.02196122052058058 ) ) ;
#29962 = CARTESIAN_POINT ( 'NONE',  ( 3.980102097228898626E-15, 80.00000000000001421, 32.50000000000000000 ) ) ;
#29963 = CARTESIAN_POINT ( 'NONE',  ( -24.18731323226221974, 40.78347249907601935, 14.01125832528330406 ) ) ;
#29964 = CARTESIAN_POINT ( 'NONE',  ( -26.29305231718579350, 65.80000000000001137, -19.10302069950537884 ) ) ;
#29965 = CARTESIAN_POINT ( 'NONE',  ( -33.58253175000000113, 15.12500000273120371, 0.000000000000000000 ) ) ;
#29966 = CARTESIAN_POINT ( 'NONE',  ( -23.41746824999999887, 4.124999997268813168, -2.867812753649727150E-15 ) ) ;
#29967 = CARTESIAN_POINT ( 'NONE',  ( 2.584737979205441561E-13, 55.39843749999999289, 27.95245687107222921 ) ) ;
#29968 = EDGE_LOOP ( 'NONE', ( #17073, #19814, #27707, #10113 ) ) ;
#29969 = CARTESIAN_POINT ( 'NONE',  ( 10.37757302488624767, 55.72500000273118559, 31.93888565452638417 ) ) ;
#29970 = CARTESIAN_POINT ( 'NONE',  ( 6.486482029760649416E-15, 25.87500000273117351, 35.31076352940723240 ) ) ;
#29971 = EDGE_CURVE ( 'NONE', #7495, #5936, #16604, .T. ) ;
#29972 = EDGE_LOOP ( 'NONE', ( #13670, #31083, #6850, #12385 ) ) ;
#29973 = CARTESIAN_POINT ( 'NONE',  ( 15.01150461594643204, 24.17447916666666785, 26.00068869287340334 ) ) ;
#29974 = CARTESIAN_POINT ( 'NONE',  ( 7.543491769121427382, 24.32329833425730214, -28.00173670424548433 ) ) ;
#29975 = CARTESIAN_POINT ( 'NONE',  ( -10.04305231718578462, 10.39999999999999325, 30.90933677959249337 ) ) ;
#29976 = CARTESIAN_POINT ( 'NONE',  ( -4.732186688966233175E-15, 15.24999999453762811, 25.76082449383753925 ) ) ;
#29977 = EDGE_CURVE ( 'NONE', #23373, #27958, #8006, .T. ) ;
#29978 = CARTESIAN_POINT ( 'NONE',  ( -7.236395654485763274, 4.024999997268824181, 22.27133577429736633 ) ) ;
#29979 = CARTESIAN_POINT ( 'NONE',  ( -33.58253175000000113, 19.37500000273118062, 0.000000000000000000 ) ) ;
#29980 = CARTESIAN_POINT ( 'NONE',  ( 6.277390505771533514E-15, 31.00000000546236834, 34.17252228774368916 ) ) ;
#29981 = CARTESIAN_POINT ( 'NONE',  ( -10.04305231718579172, 69.59999999999999432, -30.90933677959248982 ) ) ;
#29982 = FACE_OUTER_BOUND ( 'NONE', #25482, .T. ) ;
#29983 = CARTESIAN_POINT ( 'NONE',  ( 14.97647472619947351, 53.11236083425731636, 26.02091320914850314 ) ) ;
#29984 = CARTESIAN_POINT ( 'NONE',  ( 10.37757302488624056, 34.77500000273120406, -31.93888565452638417 ) ) ;
#29985 = CARTESIAN_POINT ( 'NONE',  ( 27.16883889988623935, 54.32500000273120122, -19.73931689729374384 ) ) ;
#29986 = CARTESIAN_POINT ( 'NONE',  ( -26.00068869287340334, 31.90885416666666785, 15.01150461594643559 ) ) ;
#29987 = SURFACE_STYLE_FILL_AREA ( #24352 ) ;
#29988 = CARTESIAN_POINT ( 'NONE',  ( -14.47279130897152122, 8.424999997268816543, 19.92008829642072243 ) ) ;
#29989 = CARTESIAN_POINT ( 'NONE',  ( -32.50000000000000000, 16.00000000000001421, 0.000000000000000000 ) ) ;
#29990 = CARTESIAN_POINT ( 'NONE',  ( 24.50000000000000355, 13.89999999999999858, 7.960532557706212486 ) ) ;
#29991 = CARTESIAN_POINT ( 'NONE',  ( -19.06425588902558133, 47.51524333240936215, 19.11951029504797006 ) ) ;
#29992 = CARTESIAN_POINT ( 'NONE',  ( 27.16883889988624290, 53.92500000273120264, 19.73931689729373673 ) ) ;
#29993 = CARTESIAN_POINT ( 'NONE',  ( 33.58253175000000823, 48.27500000273119696, 10.91162601494192685 ) ) ;
#29994 = CARTESIAN_POINT ( 'NONE',  ( 7.236395654485755280, 12.22499999726881015, 22.27133577429736988 ) ) ;
#29995 = CARTESIAN_POINT ( 'NONE',  ( 10.04305231718579705, 67.10000000546237686, 30.90933677959248982 ) ) ;
#29996 = CARTESIAN_POINT ( 'NONE',  ( -27.16883889988624290, 2.925000002731187543, -19.73931689729374028 ) ) ;
#29997 = CARTESIAN_POINT ( 'NONE',  ( -19.06425588902591173, 37.50038166759063074, -19.11951029504763611 ) ) ;
#29998 = CARTESIAN_POINT ( 'NONE',  ( 31.78768264672016741, 66.99999999999997158, -7.374898305514718366 ) ) ;
#29999 = FACE_OUTER_BOUND ( 'NONE', #33532, .T. ) ;
#30000 = CARTESIAN_POINT ( 'NONE',  ( -20.75514604977248823, 26.82500000273117280, -28.56700777964554305 ) ) ;
#30001 = LINE ( 'NONE', #6506, #28635 ) ;
#30002 = CARTESIAN_POINT ( 'NONE',  ( -32.50000000000000000, 58.50000000546237544, 0.000000000000000000 ) ) ;
#30003 = CARTESIAN_POINT ( 'NONE',  ( -5.147494310547640062, 30.94874572391553258, 32.49999999999992895 ) ) ;
#30004 = CARTESIAN_POINT ( 'NONE',  ( -20.53372385742107653, 51.81211833240936215, -20.47846945139867003 ) ) ;
#30005 = CARTESIAN_POINT ( 'NONE',  ( -32.50000000000000000, 50.40000000546237402, -10.55989012756945478 ) ) ;
#30006 =( BOUNDED_CURVE ( )  B_SPLINE_CURVE ( 2, ( #25026, #7004, #17486, #6831, #14906, #27948, #9398, #11644, #11982, #9231, #22451, #22623, #24688 ),
 .UNSPECIFIED., .F., .T. ) 
 B_SPLINE_CURVE_WITH_KNOTS ( ( 3, 2, 2, 2, 2, 2, 3 ),
 ( 0.1944444444444444475, 0.2000000000000000111, 0.2111111111111111105, 0.2222222222222222099, 0.2333333333333333370, 0.2444444444444444364, 0.2499999999999999722 ),
 .UNSPECIFIED. ) 
 CURVE ( )  GEOMETRIC_REPRESENTATION_ITEM ( )  RATIONAL_B_SPLINE_CURVE ( ( 0.9755282581475768211, 0.9755282581475768211, 1.000000000000000000, 0.9510565162951535312, 1.000000000000000000, 0.9510565162951535312, 1.000000000000000000, 0.9510565162951535312, 1.000000000000000000, 0.9510565162951535312, 1.000000000000000000, 0.9755282581475768211, 0.9755282581475768211 ) ) 
 REPRESENTATION_ITEM ( '' )  );
#30007 = CARTESIAN_POINT ( 'NONE',  ( -10.04305231718579172, 58.10000000546237686, -30.90933677959248982 ) ) ;
#30008 = CARTESIAN_POINT ( 'NONE',  ( -10.37757302488623701, 31.52500000273117564, 31.93888565452638417 ) ) ;
#30009 = CARTESIAN_POINT ( 'NONE',  ( -19.09188309203694445, 29.18749999999999645, -19.09188309203661049 ) ) ;
#30010 = CARTESIAN_POINT ( 'NONE',  ( -33.58253175000000113, 75.12500000273118417, 0.000000000000000000 ) ) ;
#30011 = CARTESIAN_POINT ( 'NONE',  ( 20.50609665441005092, 30.90624999999999645, 20.50609665440969209 ) ) ;
#30012 = AXIS2_PLACEMENT_3D ( 'NONE', #8358, #11280, #29616 ) ;
#30013 = EDGE_CURVE ( 'NONE', #18081, #16083, #20110, .T. ) ;
#30014 = CARTESIAN_POINT ( 'NONE',  ( 0.000000000000000000, 52.00000000000000711, 0.000000000000000000 ) ) ;
#30015 = ORIENTED_EDGE ( 'NONE', *, *, #24524, .F. ) ;
#30016 = CARTESIAN_POINT ( 'NONE',  ( 28.02196122052045268, 48.95871500092396644, -7.468012846824774620 ) ) ;
#30017 = CARTESIAN_POINT ( 'NONE',  ( 32.50000000000000000, 11.50000000546237722, -3.980102097228898626E-15 ) ) ;
#30018 = CARTESIAN_POINT ( 'NONE',  ( -15.01150461594595775, 62.55989583333332860, 26.00068869287368756 ) ) ;
#30019 = CARTESIAN_POINT ( 'NONE',  ( 20.08610463437157279, 57.29999999999999005, -27.64615127144129758 ) ) ;
#30020 = CARTESIAN_POINT ( 'NONE',  ( -20.75514604977248823, 41.07500000273119412, -28.56700777964554305 ) ) ;
#30021 = CARTESIAN_POINT ( 'NONE',  ( -32.50000000000000000, 48.50000000546239676, 0.000000000000000000 ) ) ;
#30022 = CARTESIAN_POINT ( 'NONE',  ( -9.270509831248421762, 80.30000000000002558, 12.75976212528060039 ) ) ;
#30023 = CARTESIAN_POINT ( 'NONE',  ( -10.37757302488623701, 29.52500000273117209, 31.93888565452638417 ) ) ;
#30024 = CARTESIAN_POINT ( 'NONE',  ( 1.555960095263670572E-15, 12.50000000000000355, -24.50000000000000000 ) ) ;
#30025 = CARTESIAN_POINT ( 'NONE',  ( -2.162160676586881955E-15, 56.87500000273117706, -35.31076352940723240 ) ) ;
#30026 = CARTESIAN_POINT ( 'NONE',  ( -26.29305231718579350, 35.79999999999998295, -19.10302069950537884 ) ) ;
#30027 = CARTESIAN_POINT ( 'NONE',  ( -32.50000000000000000, 31.90000000000001279, -10.55989012756945478 ) ) ;
#30028 = CARTESIAN_POINT ( 'NONE',  ( -23.41746824999999887, 9.624999997268817609, -2.867812753649727150E-15 ) ) ;
#30029 = CARTESIAN_POINT ( 'NONE',  ( -33.58253175000000113, 1.475000002731190474, 10.91162601494193929 ) ) ;
#30030 = DIRECTION ( 'NONE',  ( 0.000000000000000000, 0.000000000000000000, -1.000000000000000000 ) ) ;
#30031 = CARTESIAN_POINT ( 'NONE',  ( 13.91746824999999532, 80.47500000273119269, -4.522059556121118540 ) ) ;
#30032 = CARTESIAN_POINT ( 'NONE',  ( 33.58253175000000823, 66.27500000273117564, 10.91162601494192685 ) ) ;
#30033 = CARTESIAN_POINT ( 'NONE',  ( 3.880418787951150694, 4.198745712990782586, -24.49999999999999645 ) ) ;
#30034 = VERTEX_POINT ( 'NONE', #29268 ) ;
#30035 = CARTESIAN_POINT ( 'NONE',  ( 24.50000000000000355, 5.649999994537638237, 7.960532557706212486 ) ) ;
#30036 = CARTESIAN_POINT ( 'NONE',  ( 24.22776226481241224, 11.00298583425731103, -13.94119854578936923 ) ) ;
#30037 = CARTESIAN_POINT ( 'NONE',  ( 0.000000000000000000, 102.0000000000000284, 0.000000000000000000 ) ) ;
#30038 = CARTESIAN_POINT ( 'NONE',  ( 20.75514604977249178, 45.82500000273118701, 28.56700777964553950 ) ) ;
#30039 = CARTESIAN_POINT ( 'NONE',  ( 27.16883889988624290, 2.175000002731186655, 19.73931689729373673 ) ) ;
#30040 = CARTESIAN_POINT ( 'NONE',  ( -20.75514604977248823, 63.07500000273119412, -28.56700777964554305 ) ) ;
#30041 = CARTESIAN_POINT ( 'NONE',  ( 24.20753774853731244, 50.81510416666666430, -13.97622843553633132 ) ) ;
#30042 = CARTESIAN_POINT ( 'NONE',  ( 7.543491769121427382, 41.51079833425730214, -28.00173670424548433 ) ) ;
#30043 = CARTESIAN_POINT ( 'NONE',  ( 30.02300923189239867, 25.60118083240935860, -0.04044903255044467877 ) ) ;
#30044 = CARTESIAN_POINT ( 'NONE',  ( -20.08610463437156923, 64.80000000546237970, 27.64615127144130113 ) ) ;
#30045 = CARTESIAN_POINT ( 'NONE',  ( -13.91746824999999532, 76.97500000273119269, 4.522059556121122093 ) ) ;
#30046 = CARTESIAN_POINT ( 'NONE',  ( 26.09010956794244507, 56.68190999907602645, 6.950374756619249084 ) ) ;
#30047 = CARTESIAN_POINT ( 'NONE',  ( 5.779280353836490358E-15, 14.50000000000000178, 32.49999999999999289 ) ) ;
#30048 = CARTESIAN_POINT ( 'NONE',  ( 20.08610463437158344, 58.70000000000000995, 27.64615127144129403 ) ) ;
#30049 = ORIENTED_EDGE ( 'NONE', *, *, #11361, .T. ) ;
#30050 = CARTESIAN_POINT ( 'NONE',  ( 6.486482029760649416E-15, 39.87500000273119127, 35.31076352940723240 ) ) ;
#30051 = CARTESIAN_POINT ( 'NONE',  ( -15.00000000000000000, 81.12500000273121259, 0.000000000000000000 ) ) ;
#30052 = CARTESIAN_POINT ( 'NONE',  ( 6.277390505771533514E-15, 29.00000000546237189, 34.17252228774368916 ) ) ;
#30053 = VERTEX_POINT ( 'NONE', #26707 ) ;
#30054 = CARTESIAN_POINT ( 'NONE',  ( 15.01150461594596308, 29.90364583333332504, -26.00068869287367335 ) ) ;
#30055 = EDGE_LOOP ( 'NONE', ( #8783, #11389 ) ) ;
#30056 = CARTESIAN_POINT ( 'NONE',  ( -20.08610463437157989, 55.69999999999998863, -27.64615127144129758 ) ) ;
#30057 = CARTESIAN_POINT ( 'NONE',  ( -20.75514604977248823, 50.82500000273116569, -28.56700777964554305 ) ) ;
#30058 = CARTESIAN_POINT ( 'NONE',  ( -28.01184896238304134, 59.83854166666666430, -7.505752307972844761 ) ) ;
#30059 = CARTESIAN_POINT ( 'NONE',  ( 26.29305231718578995, 11.70000000546239605, -19.10302069950538240 ) ) ;
#30060 = CARTESIAN_POINT ( 'NONE',  ( 33.58253175000000113, 66.12500000273118417, -4.112674001490185761E-15 ) ) ;
#30061 = CARTESIAN_POINT ( 'NONE',  ( -23.41746824999999887, 12.12499999726882116, -2.867812753649727150E-15 ) ) ;
#30062 = CARTESIAN_POINT ( 'NONE',  ( -32.50000000000000000, 55.90000000000000568, -10.55989012756945478 ) ) ;
#30063 = CARTESIAN_POINT ( 'NONE',  ( 33.58253175000000113, 26.37500000273118417, -4.112674001490185761E-15 ) ) ;
#30064 = CARTESIAN_POINT ( 'NONE',  ( 0.000000000000000000, -20.99999999999998934, 0.000000000000000000 ) ) ;
#30065 = CARTESIAN_POINT ( 'NONE',  ( 24.22776226481265383, 19.01263916574269075, 13.94119854578893580 ) ) ;
#30066 = CARTESIAN_POINT ( 'NONE',  ( 8.601468415847520532, 75.57500000273120122, 11.83890561707634781 ) ) ;
#30067 = CARTESIAN_POINT ( 'NONE',  ( 4.635254915624209993, 75.65000000546237402, -14.26584774442730463 ) ) ;
#30068 = CARTESIAN_POINT ( 'NONE',  ( -33.58253175000000113, 1.375000002731191495, 0.000000000000000000 ) ) ;
#30069 = CARTESIAN_POINT ( 'NONE',  ( -26.29305231718578995, 6.199999999999997513, 19.10302069950538595 ) ) ;
#30070 = VERTEX_POINT ( 'NONE', #16251 ) ;
#30071 = CARTESIAN_POINT ( 'NONE',  ( -23.41746825000000598, 10.22499999726881903, 7.608796670333726198 ) ) ;
#30072 = CARTESIAN_POINT ( 'NONE',  ( 20.08610463437158344, 71.20000000546237118, 27.64615127144129403 ) ) ;
#30073 = CARTESIAN_POINT ( 'NONE',  ( -2.428612866367529427E-13, 43.36718749999999289, -27.95245687107222921 ) ) ;
#30074 = CARTESIAN_POINT ( 'NONE',  ( 27.16883889988624290, 63.92500000273120264, 19.73931689729373673 ) ) ;
#30075 = CARTESIAN_POINT ( 'NONE',  ( 6.486482029760649416E-15, 27.87500000273120193, 35.31076352940723240 ) ) ;
#30076 = CARTESIAN_POINT ( 'NONE',  ( 10.37757302488624767, 17.97500000273118204, 31.93888565452638417 ) ) ;
#30077 = CARTESIAN_POINT ( 'NONE',  ( 20.75514604977248467, 10.67500000273119021, -28.56700777964554305 ) ) ;
#30078 = CARTESIAN_POINT ( 'NONE',  ( 20.53372385742072481, 10.85975666759064318, -20.47846945139902175 ) ) ;
#30079 = CARTESIAN_POINT ( 'NONE',  ( -2.584737979205441561E-13, 53.67968750000000000, -30.02300923189239512 ) ) ;
#30080 = CARTESIAN_POINT ( 'NONE',  ( -13.91746824999999532, 77.47500000273120691, 4.522059556121122093 ) ) ;
#30081 = CARTESIAN_POINT ( 'NONE',  ( 20.08610463437158344, 48.70000000000000284, 27.64615127144129403 ) ) ;
#30082 = CARTESIAN_POINT ( 'NONE',  ( 32.50000000000000000, 57.60000000546236976, -10.55989012756945833 ) ) ;
#30083 = CARTESIAN_POINT ( 'NONE',  ( -20.75514604977248112, 51.42500000273118133, 28.56700777964554661 ) ) ;
#30084 = CARTESIAN_POINT ( 'NONE',  ( 18.94512977948576093, 2.824999997268817786, -13.76444248337722875 ) ) ;
#30085 = ORIENTED_EDGE ( 'NONE', *, *, #15671, .F. ) ;
#30086 = CARTESIAN_POINT ( 'NONE',  ( -10.37757302488624411, 62.97500000273119269, -31.93888565452638417 ) ) ;
#30087 = CARTESIAN_POINT ( 'NONE',  ( 0.000000000000000000, 80.00000000000001421, 0.000000000000000000 ) ) ;
#30088 = CARTESIAN_POINT ( 'NONE',  ( -23.41746825000000243, 11.52499999726880553, -7.608796670333730638 ) ) ;
#30089 = CARTESIAN_POINT ( 'NONE',  ( -26.09010956794232428, 33.48996500092397355, 6.950374756619732253 ) ) ;
#30090 = ORIENTED_EDGE ( 'NONE', *, *, #22577, .T. ) ;
#30091 = CARTESIAN_POINT ( 'NONE',  ( 27.16883889988624290, 27.92500000273119554, 19.73931689729373673 ) ) ;
#30092 = DIRECTION ( 'NONE',  ( 0.000000000000000000, 0.000000000000000000, -1.000000000000000000 ) ) ;
#30093 = ORIENTED_EDGE ( 'NONE', *, *, #30099, .T. ) ;
#30094 = CARTESIAN_POINT ( 'NONE',  ( -26.00068869287368756, 56.54427083333332149, -15.01150461594595775 ) ) ;
#30095 = CARTESIAN_POINT ( 'NONE',  ( -20.75514604977248112, 57.67500000273118133, 28.56700777964554661 ) ) ;
#30096 = CARTESIAN_POINT ( 'NONE',  ( -32.50000000000000000, 36.50000000546238255, 0.000000000000000000 ) ) ;
#30097 = CARTESIAN_POINT ( 'NONE',  ( -33.58253175000000113, 65.02500000273118985, -10.91162601494193218 ) ) ;
#30098 = CARTESIAN_POINT ( 'NONE',  ( -20.50609665440969209, 28.32812499999999645, 20.50609665441005092 ) ) ;
#30099 = EDGE_CURVE ( 'NONE', #4064, #5214, #5433, .T. ) ;
#30100 = CARTESIAN_POINT ( 'NONE',  ( 24.50000000000000000, 8.000000000000007105, 0.000000000000000000 ) ) ;
#30101 = DIRECTION ( 'NONE',  ( 0.000000000000000000, 0.000000000000000000, -1.000000000000000000 ) ) ;
#30102 = CARTESIAN_POINT ( 'NONE',  ( 27.16883889988623935, 16.32500000273118346, -19.73931689729374384 ) ) ;
#30103 = CARTESIAN_POINT ( 'NONE',  ( 8.601468415847520532, 73.57500000273117280, 11.83890561707634603 ) ) ;
#30104 = CARTESIAN_POINT ( 'NONE',  ( 20.47846945139867003, 45.79649333240935505, -20.53372385742107653 ) ) ;
#30105 = CARTESIAN_POINT ( 'NONE',  ( -13.91746824999999887, 71.37500000273119838, 0.000000000000000000 ) ) ;
#30106 = CARTESIAN_POINT ( 'NONE',  ( 26.00068869287367690, 61.70052083333332860, 15.01150461594596486 ) ) ;
#30107 = EDGE_CURVE ( 'NONE', #1345, #19609, #13504, .T. ) ;
#30108 = EDGE_CURVE ( 'NONE', #1221, #2261, #7577, .T. ) ;
#30109 = FACE_BOUND ( 'NONE', #15531, .T. ) ;
#30110 = CARTESIAN_POINT ( 'NONE',  ( 19.82091636218621389, 5.949999994537630066, -14.40073868116559197 ) ) ;
#30111 = CARTESIAN_POINT ( 'NONE',  ( 4.635254915624209993, 79.65000000546237402, -14.26584774442730463 ) ) ;
#30112 = CARTESIAN_POINT ( 'NONE',  ( -2.428612866367529427E-13, 12.42968749999999289, -27.95245687107222921 ) ) ;
#30113 = CARTESIAN_POINT ( 'NONE',  ( -10.37757302488623701, 39.52500000273118275, 31.93888565452638417 ) ) ;
#30114 = CARTESIAN_POINT ( 'NONE',  ( 8.601468415847516980, 72.17500000273116711, -11.83890561707634781 ) ) ;
#30115 = CARTESIAN_POINT ( 'NONE',  ( -27.16883889988623935, 47.57500000273119412, 19.73931689729374739 ) ) ;
#30116 = CARTESIAN_POINT ( 'NONE',  ( -33.58253175000000113, 27.37500000273118772, 0.000000000000000000 ) ) ;
#30117 = CARTESIAN_POINT ( 'NONE',  ( -32.50000000000000000, 68.00000000000000000, 0.000000000000000000 ) ) ;
#30118 = ADVANCED_FACE ( 'NONE', ( #20794, #2418 ), #336, .F. ) ;
#30119 = CARTESIAN_POINT ( 'NONE',  ( 27.95245687107223276, 27.03906250000000000, -2.463307335887066074E-13 ) ) ;
#30120 = CARTESIAN_POINT ( 'NONE',  ( -20.08610463437156923, 18.30000000000000426, 27.64615127144130113 ) ) ;
#30121 = LINE ( 'NONE', #27562, #31071 ) ;
#30122 = CARTESIAN_POINT ( 'NONE',  ( -32.50000000000000000, 69.99999999999998579, 0.000000000000000000 ) ) ;
#30123 = CARTESIAN_POINT ( 'NONE',  ( -14.47279130897152299, 13.92499999726881654, 19.92008829642072243 ) ) ;
#30124 = CARTESIAN_POINT ( 'NONE',  ( 20.47846945139867003, 21.73399333240935505, -20.53372385742107653 ) ) ;
#30125 = CARTESIAN_POINT ( 'NONE',  ( 1.507698388325705758E-15, 3.624999997268822938, -24.62258325217400312 ) ) ;
#30126 = CARTESIAN_POINT ( 'NONE',  ( -27.95245687107223986, 34.19493083240935505, 0.04044903255043252877 ) ) ;
#30127 = CARTESIAN_POINT ( 'NONE',  ( -20.75514604977248112, 77.67500000273119554, 28.56700777964554661 ) ) ;
#30128 = CARTESIAN_POINT ( 'NONE',  ( 33.58253175000000823, 16.02500000273119340, 10.91162601494192685 ) ) ;
#30129 = CARTESIAN_POINT ( 'NONE',  ( 18.94512977948575738, 2.924999997268806773, 13.76444248337723408 ) ) ;
#30130 = CARTESIAN_POINT ( 'NONE',  ( -13.97622843553588901, 59.12239583333333570, 24.20753774853756823 ) ) ;
#30131 = VERTEX_POINT ( 'NONE', #13056 ) ;
#30132 = CARTESIAN_POINT ( 'NONE',  ( 33.58253175000000823, 52.02500000273118985, 10.91162601494192863 ) ) ;
#30133 = CARTESIAN_POINT ( 'NONE',  ( 20.75514604977248467, 22.67500000273119198, -28.56700777964554305 ) ) ;
#30134 = ORIENTED_EDGE ( 'NONE', *, *, #13556, .T. ) ;
#30135 = CARTESIAN_POINT ( 'NONE',  ( -7.505752307972844761, 21.16666666666666430, 28.01184896238304134 ) ) ;
#30136 = CARTESIAN_POINT ( 'NONE',  ( 20.53372385742072481, 28.04725666759063429, -20.47846945139902175 ) ) ;
#30137 = CARTESIAN_POINT ( 'NONE',  ( 5.779280353836490358E-15, 38.50000000000000000, 32.49999999999999289 ) ) ;
#30138 = CARTESIAN_POINT ( 'NONE',  ( 15.14183272437241889, 17.44999999453764516, 20.84094480462498211 ) ) ;
#30139 = CARTESIAN_POINT ( 'NONE',  ( 7.236395654485760609, 5.024999997268825069, -22.27133577429736633 ) ) ;
#30140 = CARTESIAN_POINT ( 'NONE',  ( 33.58253175000000113, 20.37500000273118062, -4.112674001490185761E-15 ) ) ;
#30141 = CARTESIAN_POINT ( 'NONE',  ( 20.08610463437157279, 25.80000000546239036, -27.64615127144129758 ) ) ;
#30142 = CARTESIAN_POINT ( 'NONE',  ( -10.04305231718578462, 72.40000000000001990, 30.90933677959249337 ) ) ;
#30143 = CARTESIAN_POINT ( 'NONE',  ( 10.04305231718579705, 33.10000000546236976, 30.90933677959248982 ) ) ;
#30144 = CARTESIAN_POINT ( 'NONE',  ( -30.20345010595928059, 66.99999999999998579, -14.84467937978526564 ) ) ;
#30145 = CARTESIAN_POINT ( 'NONE',  ( 28.00173670424549499, 56.12017333425732346, 7.543491769121417612 ) ) ;
#30146 = CARTESIAN_POINT ( 'NONE',  ( -20.75514604977248112, 35.67500000273118843, 28.56700777964554661 ) ) ;
#30147 = CARTESIAN_POINT ( 'NONE',  ( 33.58253175000000113, 54.22500000273117848, -10.91162601494193574 ) ) ;
#30148 = PRODUCT_DEFINITION_FORMATION_WITH_SPECIFIED_SOURCE ( 'ANY', '', #18127, .NOT_KNOWN. ) ;
#30149 = CARTESIAN_POINT ( 'NONE',  ( 2.740863092043355209E-13, 31.33593749999999289, 30.02300923189239867 ) ) ;
#30150 = CARTESIAN_POINT ( 'NONE',  ( 14.47279130897151767, 9.424999997268814766, -19.92008829642072598 ) ) ;
#30151 = CARTESIAN_POINT ( 'NONE',  ( -26.29305231718579350, 17.79999999999998295, -19.10302069950537884 ) ) ;
#30152 = CARTESIAN_POINT ( 'NONE',  ( -4.732186688966233175E-15, 15.50000000000000533, 25.76082449383753925 ) ) ;
#30153 = CARTESIAN_POINT ( 'NONE',  ( -19.06425588902558133, 40.64024333240936215, 19.11951029504797006 ) ) ;
#30154 = CARTESIAN_POINT ( 'NONE',  ( 33.58253175000000113, 58.22500000273116427, -10.91162601494193751 ) ) ;
#30155 = CARTESIAN_POINT ( 'NONE',  ( 27.16883889988624290, 48.17500000273117422, 19.73931689729373673 ) ) ;
#30156 = CARTESIAN_POINT ( 'NONE',  ( -7.236395654485757944, 13.22499999726881015, -22.27133577429736988 ) ) ;
#30157 = DIRECTION ( 'NONE',  ( 1.000000000000000000, 0.000000000000000000, -0.000000000000000000 ) ) ;
#30158 = CARTESIAN_POINT ( 'NONE',  ( -5.147494310547430452, 5.551254281546842861, -32.49999999999999289 ) ) ;
#30159 = CARTESIAN_POINT ( 'NONE',  ( 24.18731323226247554, 45.95090250092398065, 14.01125832528285997 ) ) ;
#30160 = EDGE_CURVE ( 'NONE', #11531, #33874, #18387, .T. ) ;
#30161 = CARTESIAN_POINT ( 'NONE',  ( 32.50000000000000000, 63.60000000546238397, -10.55989012756945833 ) ) ;
#30162 = DIRECTION ( 'NONE',  ( -1.224646799147353454E-16, 1.000000000000000000, -0.000000000000000000 ) ) ;
#30163 = CARTESIAN_POINT ( 'NONE',  ( 20.75514604977248467, 20.42500000273120619, -28.56700777964554305 ) ) ;
#30164 = CARTESIAN_POINT ( 'NONE',  ( -15.00000000000000000, 81.12500000273121259, 0.000000000000000000 ) ) ;
#30165 = CARTESIAN_POINT ( 'NONE',  ( 26.29305231718579350, 55.30000000546237970, 19.10302069950537529 ) ) ;
#30166 = CARTESIAN_POINT ( 'NONE',  ( 26.29305231718578995, 41.70000000546237118, -19.10302069950538240 ) ) ;
#30167 = CARTESIAN_POINT ( 'NONE',  ( -20.53372385742107653, 62.12461833240934794, -20.47846945139867003 ) ) ;
#30168 = CARTESIAN_POINT ( 'NONE',  ( 10.04305231718579705, 45.10000000546236976, 30.90933677959248982 ) ) ;
#30169 = CARTESIAN_POINT ( 'NONE',  ( 32.50000000000000711, 34.89999999999999858, 10.55989012756945122 ) ) ;
#30170 = CARTESIAN_POINT ( 'NONE',  ( -2.162160676586882350E-15, 32.62500000273119838, -35.31076352940722529 ) ) ;
#30171 = VECTOR ( 'NONE', #14549, 1000.000000000000000 ) ;
#30172 = CARTESIAN_POINT ( 'NONE',  ( -27.95245687107222921, 25.32031250000000000, 2.498001805406602216E-13 ) ) ;
#30173 = EDGE_LOOP ( 'NONE', ( #29218, #16573, #29388, #18105 ) ) ;
#30174 = CARTESIAN_POINT ( 'NONE',  ( -33.58253175000000113, 77.12500000273118417, 0.000000000000000000 ) ) ;
#30175 = CARTESIAN_POINT ( 'NONE',  ( 26.00068869287367335, 41.07552083333331439, 15.01150461594596308 ) ) ;
#30176 = FACE_OUTER_BOUND ( 'NONE', #16906, .T. ) ;
#30177 = VERTEX_POINT ( 'NONE', #5500 ) ;
#30178 = CARTESIAN_POINT ( 'NONE',  ( 0.04044903254992426173, 51.68006916759063785, -30.02300923189239867 ) ) ;
#30179 = CARTESIAN_POINT ( 'NONE',  ( -32.50000000000000000, 10.60000000546237331, 10.55989012756946366 ) ) ;
#30180 = CARTESIAN_POINT ( 'NONE',  ( -2.584737979205441561E-13, 60.55468749999999289, -30.02300923189239512 ) ) ;
#30181 = CARTESIAN_POINT ( 'NONE',  ( -10.37757302488624411, 42.97500000273119269, -31.93888565452638417 ) ) ;
#30182 = CONICAL_SURFACE ( 'NONE', #16520, 12.11607355459420354, 0.8042044335707554392 ) ;
#30183 = CARTESIAN_POINT ( 'NONE',  ( 26.29305231718578995, 41.70000000546237118, -19.10302069950538240 ) ) ;
#30184 = CARTESIAN_POINT ( 'NONE',  ( -4.300734207923759378, 72.97500000273122112, -13.23629886949340495 ) ) ;
#30185 = CARTESIAN_POINT ( 'NONE',  ( -27.16883889988624290, 26.92500000273118133, -19.73931689729374028 ) ) ;
#30186 = LINE ( 'NONE', #4286, #31305 ) ;
#30187 = CARTESIAN_POINT ( 'NONE',  ( -10.37757302488623701, 53.77500000273119696, 31.93888565452638417 ) ) ;
#30188 =( LENGTH_UNIT ( ) NAMED_UNIT ( * ) SI_UNIT ( .MILLI., .METRE. ) );
#30189 = CARTESIAN_POINT ( 'NONE',  ( -10.04305231718579172, 37.60000000000000853, -30.90933677959248982 ) ) ;
#30190 = CARTESIAN_POINT ( 'NONE',  ( 10.04305231718579705, 34.59999999999999432, 30.90933677959248982 ) ) ;
#30191 = CARTESIAN_POINT ( 'NONE',  ( -4.523095164977116484E-15, 12.12499999726881406, 24.62258325217400312 ) ) ;
#30192 = CARTESIAN_POINT ( 'NONE',  ( -20.75514604977248823, 72.82500000273118701, -28.56700777964554305 ) ) ;
#30193 = CARTESIAN_POINT ( 'NONE',  ( 0.000000000000000000, 0.000000000000000000, 24.50000000000000000 ) ) ;
#30194 = AXIS2_PLACEMENT_3D ( 'NONE', #2878, #31357, #7513 ) ;
#30195 = AXIS2_PLACEMENT_3D ( 'NONE', #22639, #26366, #28931 ) ;
#30196 = CARTESIAN_POINT ( 'NONE',  ( -4.300734207923755825, 77.77500000273118985, 13.23629886949340673 ) ) ;
#30197 = CARTESIAN_POINT ( 'NONE',  ( -20.75514604977248112, 63.67500000273117422, 28.56700777964554661 ) ) ;
#30198 = CARTESIAN_POINT ( 'NONE',  ( -4.635254915624211769, 75.85000000546237686, -14.26584774442730286 ) ) ;
#30199 = EDGE_LOOP ( 'NONE', ( #30956, #31508 ) ) ;
#30200 = CARTESIAN_POINT ( 'NONE',  ( 7.570916362186213000, 6.149999994537635573, -23.30088464923126423 ) ) ;
#30201 = CARTESIAN_POINT ( 'NONE',  ( -7.025853678916393008, 22.60454833425730925, 26.06988505166735592 ) ) ;
#30202 =( BOUNDED_CURVE ( )  B_SPLINE_CURVE ( 2, ( #22626, #19718, #12504, #9402, #15082, #14569, #30678, #4433, #30165, #25550, #14402, #17489, #6834 ),
 .UNSPECIFIED., .F., .T. ) 
 B_SPLINE_CURVE_WITH_KNOTS ( ( 3, 2, 2, 2, 2, 2, 3 ),
 ( 0.2884615384615384914, 0.2897435897435897689, 0.2923076923076923239, 0.2948717948717948789, 0.2974358974358974339, 0.2999999999999999889, 0.3012820512820512664 ),
 .UNSPECIFIED. ) 
 CURVE ( )  GEOMETRIC_REPRESENTATION_ITEM ( )  RATIONAL_B_SPLINE_CURVE ( ( 0.9755282581475768211, 0.9755282581475772652, 1.000000000000000000, 0.9510565162951535312, 1.000000000000000000, 0.9510565162951535312, 1.000000000000000000, 0.9510565162951535312, 1.000000000000000000, 0.9510565162951535312, 1.000000000000000000, 0.9755282581475768211, 0.9755282581475768211 ) ) 
 REPRESENTATION_ITEM ( '' )  );
#30203 = CARTESIAN_POINT ( 'NONE',  ( 24.50000000000000000, 7.849999994537627757, -7.960532557706203605 ) ) ;
#30204 = CARTESIAN_POINT ( 'NONE',  ( -20.75514604977248823, 38.82500000273120122, -28.56700777964554305 ) ) ;
#30205 = CARTESIAN_POINT ( 'NONE',  ( -20.75514604977248112, 5.675000002731189319, 28.56700777964554661 ) ) ;
#30206 = CARTESIAN_POINT ( 'NONE',  ( 6.486482029760648627E-15, 57.87500000273117706, 35.31076352940722529 ) ) ;
#30207 = CARTESIAN_POINT ( 'NONE',  ( -19.09188309203660694, 55.82812499999999289, 19.09188309203694800 ) ) ;
#30208 = CARTESIAN_POINT ( 'NONE',  ( -30.02300923189239867, 40.50819416759064495, -0.04044903254991731589 ) ) ;
#30209 = ADVANCED_FACE ( 'NONE', ( #23696 ), #5331, .F. ) ;
#30210 = CARTESIAN_POINT ( 'NONE',  ( -7.543491769121917656, 38.34857666574267654, -28.00173670424536354 ) ) ;
#30211 = CARTESIAN_POINT ( 'NONE',  ( -32.50000000000000000, 66.50000000546239676, 0.000000000000000000 ) ) ;
#30212 = CARTESIAN_POINT ( 'NONE',  ( 13.91746825000000065, 80.27500000273120406, 4.522059556121114987 ) ) ;
#30213 = CARTESIAN_POINT ( 'NONE',  ( -13.94119854578892514, 54.24701416574269075, 24.22776226481266448 ) ) ;
#30214 = CARTESIAN_POINT ( 'NONE',  ( 0.000000000000000000, 0.000000000000000000, 0.000000000000000000 ) ) ;
#30215 = CARTESIAN_POINT ( 'NONE',  ( 26.29305231718579350, 58.80000000000001847, 19.10302069950537529 ) ) ;
#30216 = ORIENTED_EDGE ( 'NONE', *, *, #20645, .T. ) ;
#30217 = CARTESIAN_POINT ( 'NONE',  ( 27.16883889988623935, 42.57500000273119412, -19.73931689729374384 ) ) ;
#30218 = CARTESIAN_POINT ( 'NONE',  ( -23.41746824999999887, 2.024999997268815299, -7.608796670333730638 ) ) ;
#30219 = VECTOR ( 'NONE', #23468, 1000.000000000000000 ) ;
#30220 = CARTESIAN_POINT ( 'NONE',  ( -32.50000000000000000, 28.50000000546236478, 0.000000000000000000 ) ) ;
#30221 = ORIENTED_EDGE ( 'NONE', *, *, #17841, .T. ) ;
#30222 = CARTESIAN_POINT ( 'NONE',  ( 26.00068869287367335, 30.76302083333332504, 15.01150461594596308 ) ) ;
#30223 = ORIENTED_EDGE ( 'NONE', *, *, #10518, .F. ) ;
#30224 = CARTESIAN_POINT ( 'NONE',  ( -5.147494310547418017, 74.05125428700922896, -32.50000000000000000 ) ) ;
#30225 = CARTESIAN_POINT ( 'NONE',  ( -33.58253175000000113, 51.22500000273119269, 10.91162601494193929 ) ) ;
#30226 = CARTESIAN_POINT ( 'NONE',  ( 28.01184896238304134, 61.55729166666666430, 7.505752307972846538 ) ) ;
#30227 = CARTESIAN_POINT ( 'NONE',  ( 10.04305231718578817, 11.90000000546237402, -30.90933677959249337 ) ) ;
#30228 = CARTESIAN_POINT ( 'NONE',  ( 18.94512977948575738, 16.92499999726882010, 13.76444248337723408 ) ) ;
#30229 = CARTESIAN_POINT ( 'NONE',  ( 32.50000000000000000, 52.99999999999999289, -3.980102097228898626E-15 ) ) ;
#30230 = CARTESIAN_POINT ( 'NONE',  ( 2.205017735002230837E-13, 56.00000000546238255, -32.50000000000000000 ) ) ;
#30231 = CARTESIAN_POINT ( 'NONE',  ( 33.58253175000000113, 14.37500000273117529, -4.112674001490185761E-15 ) ) ;
#30232 = CARTESIAN_POINT ( 'NONE',  ( 14.01125832528330051, 26.17409749907601935, 24.18731323226221974 ) ) ;
#30233 = CARTESIAN_POINT ( 'NONE',  ( -11.25946833292375793, 76.67500000273119554, -8.180482586598733619 ) ) ;
#30234 = CARTESIAN_POINT ( 'NONE',  ( 24.50000000000000000, 8.100000000000006750, -7.960532557706203605 ) ) ;
#30235 = CARTESIAN_POINT ( 'NONE',  ( 14.93337011119343671, 52.00000000000000711, 30.15969763299871786 ) ) ;
#30236 = CARTESIAN_POINT ( 'NONE',  ( 20.75514604977248467, 78.67500000273116711, -28.56700777964554305 ) ) ;
#30237 = ORIENTED_EDGE ( 'NONE', *, *, #337, .T. ) ;
#30238 = CARTESIAN_POINT ( 'NONE',  ( -4.523095164977116484E-15, 8.624999997268810503, 24.62258325217400312 ) ) ;
#30239 = CARTESIAN_POINT ( 'NONE',  ( 11.54700538379251107, 86.00000000000001421, -19.99999999999999645 ) ) ;
#30240 = CARTESIAN_POINT ( 'NONE',  ( -13.97622843553588901, 45.37239583333333570, 24.20753774853756823 ) ) ;
#30241 = CARTESIAN_POINT ( 'NONE',  ( 27.16883889988623935, 66.32500000273118701, -19.73931689729374384 ) ) ;
#30242 = CARTESIAN_POINT ( 'NONE',  ( -27.16883889988624290, 23.17500000273119198, -19.73931689729374028 ) ) ;
#30243 = CARTESIAN_POINT ( 'NONE',  ( -27.16883889988623935, 7.575000002731188786, 19.73931689729374739 ) ) ;
#30244 = CARTESIAN_POINT ( 'NONE',  ( 20.75514604977249178, 12.07500000273120477, 28.56700777964553950 ) ) ;
#30245 = CARTESIAN_POINT ( 'NONE',  ( 30.02300923189239867, 14.72694416759064318, 0.04044903254992252006 ) ) ;
#30246 = EDGE_CURVE ( 'NONE', #5684, #7233, #8401, .T. ) ;
#30247 = CARTESIAN_POINT ( 'NONE',  ( 20.50609665441005092, 51.53124999999999289, 20.50609665440969209 ) ) ;
#30248 = EDGE_CURVE ( 'NONE', #33045, #14454, #5160, .T. ) ;
#30249 = CARTESIAN_POINT ( 'NONE',  ( 4.300734207923761154, 71.97500000273119269, 13.23629886949340495 ) ) ;
#30250 = CARTESIAN_POINT ( 'NONE',  ( 26.29305231718578995, 47.20000000000000284, -19.10302069950538240 ) ) ;
#30251 = CARTESIAN_POINT ( 'NONE',  ( 20.08610463437158344, 57.20000000546237828, 27.64615127144129403 ) ) ;
#30252 = CARTESIAN_POINT ( 'NONE',  ( 33.58253175000000113, 54.22500000273117848, -10.91162601494193574 ) ) ;
#30253 = CARTESIAN_POINT ( 'NONE',  ( -23.41746824999999887, 5.624999997268814944, -2.867812753649727150E-15 ) ) ;
#30254 = ORIENTED_EDGE ( 'NONE', *, *, #9790, .T. ) ;
#30255 = CARTESIAN_POINT ( 'NONE',  ( 33.58253175000000823, 62.27500000273118275, 10.91162601494192863 ) ) ;
#30256 = CARTESIAN_POINT ( 'NONE',  ( 26.29305231718578995, 17.19999999999999218, -19.10302069950538240 ) ) ;
#30257 = AXIS2_PLACEMENT_3D ( 'NONE', #8570, #16313, #19218 ) ;
#30258 = VECTOR ( 'NONE', #22454, 1000.000000000000000 ) ;
#30259 = CARTESIAN_POINT ( 'NONE',  ( -23.41746825000000243, 13.52499999726880198, -7.608796670333730638 ) ) ;
#30260 = CARTESIAN_POINT ( 'NONE',  ( -19.06425588902591173, 30.62538166759064495, -19.11951029504763611 ) ) ;
#30261 = VERTEX_POINT ( 'NONE', #31239 ) ;
#30262 = CARTESIAN_POINT ( 'NONE',  ( 10.37757302488624767, 33.72500000273119269, 31.93888565452638417 ) ) ;
#30263 = VECTOR ( 'NONE', #24960, 1000.000000000000000 ) ;
#30264 = DIRECTION ( 'NONE',  ( -0.000000000000000000, 1.000000000000000000, -0.000000000000000000 ) ) ;
#30265 = ADVANCED_FACE ( 'NONE', ( #33822 ), #8233, .T. ) ;
#30266 = ORIENTED_EDGE ( 'NONE', *, *, #12946, .F. ) ;
#30267 = CARTESIAN_POINT ( 'NONE',  ( -28.01184896238304134, 59.83854166666666430, -7.505752307972844761 ) ) ;
#30268 = CARTESIAN_POINT ( 'NONE',  ( 27.16883889988623935, 60.57500000273119412, -19.73931689729374384 ) ) ;
#30269 = CARTESIAN_POINT ( 'NONE',  ( 5.779280353836490358E-15, 37.00000000546237544, 32.49999999999999289 ) ) ;
#30270 = CARTESIAN_POINT ( 'NONE',  ( 20.75514604977249178, 67.82500000273120122, 28.56700777964553950 ) ) ;
#30271 = CARTESIAN_POINT ( 'NONE',  ( 7.505752307973351023, 34.63020833333332860, 28.01184896238290278 ) ) ;
#30272 = CARTESIAN_POINT ( 'NONE',  ( -19.82091636218621389, 15.19999999999999218, 14.40073868116558842 ) ) ;
#30273 = CARTESIAN_POINT ( 'NONE',  ( 20.75514604977249178, 4.075000002731195892, 28.56700777964553950 ) ) ;
#30274 = CARTESIAN_POINT ( 'NONE',  ( -33.58253175000000113, 7.125000002731196602, 0.000000000000000000 ) ) ;
#30275 = CARTESIAN_POINT ( 'NONE',  ( -11.25946833292375793, 75.07500000273120122, 8.180482586598737171 ) ) ;
#30276 = CARTESIAN_POINT ( 'NONE',  ( -30.02300923189239867, 44.50743083240935505, 0.04044903255044988294 ) ) ;
#30277 = CARTESIAN_POINT ( 'NONE',  ( 15.00000000000000355, 76.89999999999999147, 4.873795443493592394 ) ) ;
#30278 = CARTESIAN_POINT ( 'NONE',  ( 28.01184896238290278, 57.83333333333333570, -7.505752307973347470 ) ) ;
#30279 = CARTESIAN_POINT ( 'NONE',  ( 5.779280353836490358E-15, 67.00000000546236834, 32.49999999999999289 ) ) ;
#30280 = CARTESIAN_POINT ( 'NONE',  ( -15.14183272437241889, 6.449999994537612302, -20.84094480462497856 ) ) ;
#30281 = CARTESIAN_POINT ( 'NONE',  ( -4.635254915624208216, 78.65000000546237402, 14.26584774442730463 ) ) ;
#30282 = CARTESIAN_POINT ( 'NONE',  ( 24.20753774853756113, 17.01302083333332504, 13.97622843553589789 ) ) ;
#30283 = CARTESIAN_POINT ( 'NONE',  ( -33.58253175000000113, 39.02500000273118985, -10.91162601494193218 ) ) ;
#30284 = VECTOR ( 'NONE', #5105, 1000.000000000000000 ) ;
#30285 = CARTESIAN_POINT ( 'NONE',  ( -4.300734207923755825, 77.27500000273118985, 13.23629886949340673 ) ) ;
#30286 = CARTESIAN_POINT ( 'NONE',  ( -10.37757302488624411, 40.97500000273117138, -31.93888565452638417 ) ) ;
#30287 = CARTESIAN_POINT ( 'NONE',  ( 27.16883889988624290, 28.17500000273118133, 19.73931689729373673 ) ) ;
#30288 = CARTESIAN_POINT ( 'NONE',  ( -32.50000000000000000, 67.89999999999997726, -10.55989012756945300 ) ) ;
#30289 = CARTESIAN_POINT ( 'NONE',  ( 6.001560367445586717E-15, 1.500000000000005995, 24.50000000000000000 ) ) ;
#30290 = CARTESIAN_POINT ( 'NONE',  ( 32.50000000000000711, 78.89999999999997726, 10.55989012756945122 ) ) ;
#30291 = CARTESIAN_POINT ( 'NONE',  ( 20.08610463437158344, 66.69999999999997442, 27.64615127144129403 ) ) ;
#30292 = CARTESIAN_POINT ( 'NONE',  ( 23.41746824999999887, 10.72499999726880127, -7.608796670333727974 ) ) ;
#30293 = CARTESIAN_POINT ( 'NONE',  ( -15.04653450569338524, 24.45534749907602290, -25.98046417659831775 ) ) ;
#30294 = CARTESIAN_POINT ( 'NONE',  ( -8.891200544363830713E-16, 77.49999999999998579, -15.00000000000000000 ) ) ;
#30295 = CARTESIAN_POINT ( 'NONE',  ( -24.18731323226221974, 33.90847249907601935, 14.01125832528330406 ) ) ;
#30296 = CYLINDRICAL_SURFACE ( 'NONE', #28805, 32.50000000000000000 ) ;
#30297 = CARTESIAN_POINT ( 'NONE',  ( 27.16883889988623935, 16.32500000273118346, -19.73931689729374384 ) ) ;
#30298 = CARTESIAN_POINT ( 'NONE',  ( 18.94512977948575738, 10.92499999726881299, 13.76444248337723408 ) ) ;
#30299 = CARTESIAN_POINT ( 'NONE',  ( -24.20753774853730889, 59.40885416666666430, 13.97622843553633842 ) ) ;
#30300 = ADVANCED_FACE ( 'NONE', ( #15470 ), #18727, .T. ) ;
#30301 = ORIENTED_EDGE ( 'NONE', *, *, #18121, .T. ) ;
#30302 = CARTESIAN_POINT ( 'NONE',  ( -20.75514604977248112, 49.42500000273118133, 28.56700777964554661 ) ) ;
#30303 = EDGE_CURVE ( 'NONE', #10039, #7495, #15645, .T. ) ;
#30304 = CARTESIAN_POINT ( 'NONE',  ( -20.75514604977248823, 21.07500000273118346, -28.56700777964554305 ) ) ;
#30305 = EDGE_LOOP ( 'NONE', ( #25338, #21355 ) ) ;
#30306 = CARTESIAN_POINT ( 'NONE',  ( -15.01150461594642138, 32.76822916666666430, -26.00068869287340334 ) ) ;
#30307 = CARTESIAN_POINT ( 'NONE',  ( 26.02091320914851025, 31.62798583425730925, -14.97647472619946463 ) ) ;
#30308 = CARTESIAN_POINT ( 'NONE',  ( -19.82091636218621034, 2.799999999999997158, -14.40073868116559552 ) ) ;
#30309 = CARTESIAN_POINT ( 'NONE',  ( 15.14183272437241889, 15.44999999453761852, 20.84094480462498211 ) ) ;
#30310 = AXIS2_PLACEMENT_3D ( 'NONE', #11243, #23955, #924 ) ;
#30311 = EDGE_CURVE ( 'NONE', #8544, #3811, #1279, .T. ) ;
#30312 = CARTESIAN_POINT ( 'NONE',  ( -18.94512977948575738, 11.42499999726881477, -13.76444248337723231 ) ) ;
#30313 = CARTESIAN_POINT ( 'NONE',  ( -2.162160676586881955E-15, 22.87500000273118062, -35.31076352940723240 ) ) ;
#30314 = CARTESIAN_POINT ( 'NONE',  ( 32.50000000000000711, 23.40000000546237047, 10.55989012756945122 ) ) ;
#30315 = CARTESIAN_POINT ( 'NONE',  ( 10.04305231718579705, 72.59999999999999432, 30.90933677959248982 ) ) ;
#30316 = CARTESIAN_POINT ( 'NONE',  ( -32.50000000000000000, 6.400000005462388231, -10.55989012756945300 ) ) ;
#30317 = CARTESIAN_POINT ( 'NONE',  ( -20.50609665441004736, 11.99999999999999645, -20.50609665440969565 ) ) ;
#30318 = CARTESIAN_POINT ( 'NONE',  ( 28.02196122052045268, 59.27121500092397355, -7.468012846824774620 ) ) ;
#30319 = CARTESIAN_POINT ( 'NONE',  ( 33.58253175000000113, 34.37500000273119127, -4.112674001490185761E-15 ) ) ;
#30320 = CARTESIAN_POINT ( 'NONE',  ( 10.37757302488624767, 57.72500000273118559, 31.93888565452638417 ) ) ;
#30321 = CARTESIAN_POINT ( 'NONE',  ( 20.50609665440969565, 30.04687500000000000, -20.50609665441004736 ) ) ;
#30322 = DIRECTION ( 'NONE',  ( 0.000000000000000000, 0.000000000000000000, 1.000000000000000000 ) ) ;
#30323 = CARTESIAN_POINT ( 'NONE',  ( 7.236395654485760609, 11.52499999726880375, -22.27133577429736633 ) ) ;
#30324 = CARTESIAN_POINT ( 'NONE',  ( -32.50000000000000000, 14.00000000000001243, 0.000000000000000000 ) ) ;
#30325 = CARTESIAN_POINT ( 'NONE',  ( 26.29305231718578995, 9.700000005462394270, -19.10302069950538240 ) ) ;
#30326 = CARTESIAN_POINT ( 'NONE',  ( 0.04044903255044120238, 40.21055583240935505, 27.95245687107223276 ) ) ;
#30327 = CARTESIAN_POINT ( 'NONE',  ( 10.37757302488624056, 58.52500000273119696, -31.93888565452638417 ) ) ;
#30328 = CARTESIAN_POINT ( 'NONE',  ( -20.75514604977248112, 49.67500000273118133, 28.56700777964554661 ) ) ;
#30329 = CARTESIAN_POINT ( 'NONE',  ( 23.41746824999999887, 16.52499999726882152, 7.608796670333735079 ) ) ;
#30330 = DIRECTION ( 'NONE',  ( -0.000000000000000000, -1.000000000000000000, -0.000000000000000000 ) ) ;
#30331 = CARTESIAN_POINT ( 'NONE',  ( -20.08610463437157989, 5.699999999999993960, -27.64615127144129758 ) ) ;
#30332 = CARTESIAN_POINT ( 'NONE',  ( -14.01125832528285109, 46.81027750092398776, 24.18731323226248264 ) ) ;
#30333 = CARTESIAN_POINT ( 'NONE',  ( -16.62822907945918871, 16.99999999999998934, -17.41050465759853694 ) ) ;
#30334 = CARTESIAN_POINT ( 'NONE',  ( 23.95873412499999944, 1.437499995903229744, 0.000000000000000000 ) ) ;
#30335 = CARTESIAN_POINT ( 'NONE',  ( 10.37757302488624056, 24.52500000273118275, -31.93888565452638417 ) ) ;
#30336 = CARTESIAN_POINT ( 'NONE',  ( 3.735172737399427541E-15, 0.000000000000000000, 30.50000000000000000 ) ) ;
#30337 = AXIS2_PLACEMENT_3D ( 'NONE', #18213, #13050, #26089 ) ;
#30338 = CIRCLE ( 'NONE', #13923, 15.00000000000000000 ) ;
#30339 = CARTESIAN_POINT ( 'NONE',  ( 32.50000000000000711, 41.40000000546238823, 10.55989012756945122 ) ) ;
#30340 = CARTESIAN_POINT ( 'NONE',  ( -26.02091320914878025, 68.85638916574269786, -14.97647472619899389 ) ) ;
#30341 = CARTESIAN_POINT ( 'NONE',  ( -26.29305231718578995, 40.70000000546237828, 19.10302069950538595 ) ) ;
#30342 = CARTESIAN_POINT ( 'NONE',  ( -10.37757302488624411, 30.72500000273117848, -31.93888565452638417 ) ) ;
#30343 = CARTESIAN_POINT ( 'NONE',  ( 26.07999730980477437, 37.20833333333332860, -6.988114217768290004 ) ) ;
#30344 = ORIENTED_EDGE ( 'NONE', *, *, #8175, .F. ) ;
#30345 = CARTESIAN_POINT ( 'NONE',  ( -2.162160676586881955E-15, 66.62500000273118417, -35.31076352940723240 ) ) ;
#30346 = CARTESIAN_POINT ( 'NONE',  ( -15.01150461594642138, 39.64322916666667140, -26.00068869287340334 ) ) ;
#30347 = CARTESIAN_POINT ( 'NONE',  ( 0.000000000000000000, 0.000000000000000000, 0.000000000000000000 ) ) ;
#30348 = ORIENTED_EDGE ( 'NONE', *, *, #31376, .T. ) ;
#30349 = CARTESIAN_POINT ( 'NONE',  ( -0.04044903254990864921, 60.27381916759065206, 30.02300923189239867 ) ) ;
#30350 = CARTESIAN_POINT ( 'NONE',  ( -27.95245687107223986, 64.57069416759065916, -0.04044903254993292840 ) ) ;
#30351 = CARTESIAN_POINT ( 'NONE',  ( 20.75514604977248467, 8.425000002731186655, -28.56700777964554305 ) ) ;
#30352 = CARTESIAN_POINT ( 'NONE',  ( -15.01150461594642138, 60.26822916666665009, -26.00068869287340334 ) ) ;
#30353 = CARTESIAN_POINT ( 'NONE',  ( -32.50000000000000000, 64.40000000546238823, -10.55989012756945300 ) ) ;
#30354 = CARTESIAN_POINT ( 'NONE',  ( -33.58253175000000113, 43.47500000273117138, 10.91162601494193929 ) ) ;
#30355 = CARTESIAN_POINT ( 'NONE',  ( -32.50000000000000000, 42.40000000546238823, -10.55989012756945478 ) ) ;
#30356 = CARTESIAN_POINT ( 'NONE',  ( 11.25946833292375793, 74.57500000273120122, -8.180482586598735395 ) ) ;
#30357 = CARTESIAN_POINT ( 'NONE',  ( 20.75514604977249178, 27.82500000273116925, 28.56700777964553950 ) ) ;
#30358 = CARTESIAN_POINT ( 'NONE',  ( -26.29305231718579350, 23.79999999999998650, -19.10302069950537884 ) ) ;
#30359 = CARTESIAN_POINT ( 'NONE',  ( -2.162160676586881955E-15, 54.87500000273119127, -35.31076352940723240 ) ) ;
#30360 = FILL_AREA_STYLE_COLOUR ( '', #1920 ) ;
#30361 = CARTESIAN_POINT ( 'NONE',  ( -2.092463501923844636E-15, 37.50000000000000711, -34.17252228774368916 ) ) ;
#30362 = CARTESIAN_POINT ( 'NONE',  ( -20.08610463437156923, 34.29999999999998295, 27.64615127144130113 ) ) ;
#30363 = CARTESIAN_POINT ( 'NONE',  ( 23.41746824999999887, 16.62499999726882294, 0.000000000000000000 ) ) ;
#30364 = CARTESIAN_POINT ( 'NONE',  ( 20.75514604977248467, 78.42500000273116711, -28.56700777964554305 ) ) ;
#30365 = CARTESIAN_POINT ( 'NONE',  ( 26.29305231718578995, 63.20000000000001705, -19.10302069950538240 ) ) ;
#30366 = CARTESIAN_POINT ( 'NONE',  ( -13.91746824999999532, 79.27500000273117564, -4.522059556121115875 ) ) ;
#30367 = CARTESIAN_POINT ( 'NONE',  ( -10.37757302488624411, 66.97500000273117848, -31.93888565452638417 ) ) ;
#30368 = CARTESIAN_POINT ( 'NONE',  ( -9.270509831248421762, 76.55000000546237970, 12.75976212528060039 ) ) ;
#30369 = ORIENTED_EDGE ( 'NONE', *, *, #9396, .F. ) ;
#30370 = CARTESIAN_POINT ( 'NONE',  ( -15.14183272437242600, 9.049999994537618164, 20.84094480462497856 ) ) ;
#30371 = CARTESIAN_POINT ( 'NONE',  ( -24.22776226481240514, 19.59673583425730925, 13.94119854578937812 ) ) ;
#30372 = CARTESIAN_POINT ( 'NONE',  ( -10.04305231718579172, 25.60000000000001208, -30.90933677959248982 ) ) ;
#30373 = CARTESIAN_POINT ( 'NONE',  ( -27.16883889988624290, 42.92500000273118133, -19.73931689729374028 ) ) ;
#30374 = CARTESIAN_POINT ( 'NONE',  ( 27.16883889988623935, 2.575000002731184345, -19.73931689729374384 ) ) ;
#30375 = CARTESIAN_POINT ( 'NONE',  ( -27.16883889988624290, 53.17500000273118843, -19.73931689729374028 ) ) ;
#30376 = CARTESIAN_POINT ( 'NONE',  ( -28.02196122052045268, 47.23996500092398065, 7.468012846824790607 ) ) ;
#30377 = CARTESIAN_POINT ( 'NONE',  ( 0.04044903255045854962, 36.77305583240936215, 30.02300923189239867 ) ) ;
#30378 = CARTESIAN_POINT ( 'NONE',  ( 32.50000000000000711, 61.40000000546237402, 10.55989012756945122 ) ) ;
#30379 =( GEOMETRIC_REPRESENTATION_CONTEXT ( 3 ) GLOBAL_UNCERTAINTY_ASSIGNED_CONTEXT ( ( #7438 ) ) GLOBAL_UNIT_ASSIGNED_CONTEXT ( ( #12529, #33973, #13555 ) ) REPRESENTATION_CONTEXT ( 'NONE', 'WORKASPACE' ) );
#30380 = CARTESIAN_POINT ( 'NONE',  ( -4.300734207923759378, 80.97500000273122112, -13.23629886949340495 ) ) ;
#30381 = CARTESIAN_POINT ( 'NONE',  ( 7.025853678916867295, 60.69232666574269075, 26.06988505166722803 ) ) ;
#30382 = CARTESIAN_POINT ( 'NONE',  ( -32.50000000000000000, 57.99999999999999289, 0.000000000000000000 ) ) ;
#30383 = CARTESIAN_POINT ( 'NONE',  ( -2.092463501923844636E-15, 74.00000000546236834, -34.17252228774368916 ) ) ;
#30384 = CARTESIAN_POINT ( 'NONE',  ( 15.00000000000000355, 78.90000000000000568, 4.873795443493592394 ) ) ;
#30385 = CARTESIAN_POINT ( 'NONE',  ( -10.37757302488623701, 41.77500000273119696, 31.93888565452638417 ) ) ;
#30386 = CARTESIAN_POINT ( 'NONE',  ( 5.779280353836490358E-15, 76.49999999999998579, 32.49999999999999289 ) ) ;
#30387 = ORIENTED_EDGE ( 'NONE', *, *, #11880, .T. ) ;
#30388 = CARTESIAN_POINT ( 'NONE',  ( 20.08610463437157279, 29.80000000546237970, -27.64615127144129758 ) ) ;
#30389 = ORIENTED_EDGE ( 'NONE', *, *, #6000, .T. ) ;
#30390 = CARTESIAN_POINT ( 'NONE',  ( 28.01184896238290278, 33.77083333333333570, -7.505752307973347470 ) ) ;
#30391 = CARTESIAN_POINT ( 'NONE',  ( -10.04305231718579172, 62.10000000546239818, -30.90933677959248982 ) ) ;
#30393 = ORIENTED_EDGE ( 'NONE', *, *, #32495, .T. ) ;
#30392 = EDGE_CURVE ( 'NONE', #7411, #28529, #29250, .T. ) ;
#30394 = CARTESIAN_POINT ( 'NONE',  ( 32.50000000000000000, 27.09999999999998721, -10.55989012756945833 ) ) ;
#30395 = CARTESIAN_POINT ( 'NONE',  ( 10.37757302488624767, 45.72500000273119269, 31.93888565452638417 ) ) ;
#30396 = CARTESIAN_POINT ( 'NONE',  ( 4.635254915624209993, 73.65000000546240244, -14.26584774442730463 ) ) ;
#30397 = CARTESIAN_POINT ( 'NONE',  ( 7.505752307973351023, 65.56770833333332860, 28.01184896238290278 ) ) ;
#30398 = EDGE_CURVE ( 'NONE', #26987, #5934, #14589, .T. ) ;
#30399 = CARTESIAN_POINT ( 'NONE',  ( 10.04305231718579705, 7.100000005462375974, 30.90933677959248982 ) ) ;
#30400 = CARTESIAN_POINT ( 'NONE',  ( 10.37757302488624056, 66.52500000273118985, -31.93888565452638417 ) ) ;
#30401 = CARTESIAN_POINT ( 'NONE',  ( -18.94512977948576093, 12.32499999726882578, 13.76444248337722698 ) ) ;
#30402 = CIRCLE ( 'NONE', #18926, 31.38736896855613523 ) ;
#30403 = CARTESIAN_POINT ( 'NONE',  ( -10.04305231718579172, 51.60000000000000853, -30.90933677959248982 ) ) ;
#30404 = DIRECTION ( 'NONE',  ( 1.000000000000000000, 0.000000000000000000, 1.224646799147353454E-16 ) ) ;
#30405 =( BOUNDED_CURVE ( )  B_SPLINE_CURVE ( 2, ( #33477, #11905, #1085, #24944, #11733, #17883, #32493, #23191, #9316, #16898, #28166, #25761, #19803 ),
 .UNSPECIFIED., .F., .T. ) 
 B_SPLINE_CURVE_WITH_KNOTS ( ( 3, 2, 2, 2, 2, 2, 3 ),
 ( 0.02777777777777777624, 0.03333333333333333287, 0.04444444444444444614, 0.05555555555555555247, 0.06666666666666667962, 0.07777777777777777901, 0.08333333333333334259 ),
 .UNSPECIFIED. ) 
 CURVE ( )  GEOMETRIC_REPRESENTATION_ITEM ( )  RATIONAL_B_SPLINE_CURVE ( ( 0.9755282581475768211, 0.9755282581475768211, 1.000000000000000000, 0.9510565162951535312, 1.000000000000000000, 0.9510565162951535312, 1.000000000000000000, 0.9510565162951535312, 1.000000000000000000, 0.9510565162951535312, 1.000000000000000000, 0.9755282581475767101, 0.9755282581475768211 ) ) 
 REPRESENTATION_ITEM ( '' )  );
#30406 = CARTESIAN_POINT ( 'NONE',  ( 33.58253175000000113, 18.37500000273117706, -4.112674001490185761E-15 ) ) ;
#30407 = CARTESIAN_POINT ( 'NONE',  ( -5.147494310547423346, 74.44874571845315359, 32.50000000000000000 ) ) ;
#30408 = CARTESIAN_POINT ( 'NONE',  ( 19.11951029504797006, 29.46836833240935505, 19.06425588902558133 ) ) ;
#30409 = CARTESIAN_POINT ( 'NONE',  ( 8.601468415847520532, 71.57500000273118701, 11.83890561707634781 ) ) ;
#30410 = CARTESIAN_POINT ( 'NONE',  ( -5.147494310547423346, 44.44874571845313938, 32.50000000000000000 ) ) ;
#30411 = CARTESIAN_POINT ( 'NONE',  ( 33.58253175000000113, 78.47500000273116427, -10.91162601494193751 ) ) ;
#30412 = VERTEX_POINT ( 'NONE', #8737 ) ;
#30413 = CARTESIAN_POINT ( 'NONE',  ( -23.41746824999999887, 6.124999997268814944, -2.867812753649727150E-15 ) ) ;
#30414 = CARTESIAN_POINT ( 'NONE',  ( 0.000000000000000000, 80.00000000000001421, -32.50000000000000000 ) ) ;
#30415 = CARTESIAN_POINT ( 'NONE',  ( 13.97622843553589966, 50.52864583333333570, -24.20753774853756113 ) ) ;
#30416 = CARTESIAN_POINT ( 'NONE',  ( -33.58253175000000113, 61.02500000273118985, -10.91162601494193218 ) ) ;
#30417 = CARTESIAN_POINT ( 'NONE',  ( 20.75514604977248467, 26.67500000273118133, -28.56700777964554305 ) ) ;
#30418 = CARTESIAN_POINT ( 'NONE',  ( 27.16883889988624290, 8.175000002731177773, 19.73931689729373673 ) ) ;
#30419 = DIRECTION ( 'NONE',  ( 0.000000000000000000, 0.000000000000000000, -1.000000000000000000 ) ) ;
#30420 = CARTESIAN_POINT ( 'NONE',  ( -14.97647472619946285, 20.45611083425730925, -26.02091320914851025 ) ) ;
#30421 = CARTESIAN_POINT ( 'NONE',  ( 28.01184896238304134, 61.55729166666666430, 7.505752307972846538 ) ) ;
#30422 = CARTESIAN_POINT ( 'NONE',  ( -27.16883889988623935, 1.325000002731183013, 19.73931689729374739 ) ) ;
#30423 = CARTESIAN_POINT ( 'NONE',  ( 20.08610463437157279, 69.29999999999999716, -27.64615127144129758 ) ) ;
#30424 = CARTESIAN_POINT ( 'NONE',  ( 10.04305231718578817, 41.40000000000000568, -30.90933677959249337 ) ) ;
#30425 = CARTESIAN_POINT ( 'NONE',  ( 27.16883889988623935, 50.32500000273118701, -19.73931689729374384 ) ) ;
#30426 = CARTESIAN_POINT ( 'NONE',  ( 7.236395654485760609, 1.024999997268821739, -22.27133577429736633 ) ) ;
#30427 = CARTESIAN_POINT ( 'NONE',  ( 26.29305231718578995, 21.70000000546237828, -19.10302069950538240 ) ) ;
#30428 = VECTOR ( 'NONE', #13331, 1000.000000000000000 ) ;
#30429 = ORIENTED_EDGE ( 'NONE', *, *, #15361, .F. ) ;
#30430 = CARTESIAN_POINT ( 'NONE',  ( 10.37757302488624767, 59.97500000273119269, 31.93888565452638417 ) ) ;
#30431 = CARTESIAN_POINT ( 'NONE',  ( -32.50000000000000000, 2.000000000000001776, 0.000000000000000000 ) ) ;
#30432 = CARTESIAN_POINT ( 'NONE',  ( -14.47279130897152122, 9.924999997268825425, 19.92008829642072243 ) ) ;
#30433 = CARTESIAN_POINT ( 'NONE',  ( 7.025853678916403666, 34.63579833425730925, -26.06988505166735237 ) ) ;
#30434 = ORIENTED_EDGE ( 'NONE', *, *, #19726, .T. ) ;
#30435 = CARTESIAN_POINT ( 'NONE',  ( -10.37757302488623701, 31.52500000273118630, 31.93888565452638417 ) ) ;
#30436 = CARTESIAN_POINT ( 'NONE',  ( -32.50000000000000000, 34.40000000546237402, -10.55989012756945300 ) ) ;
#30437 = EDGE_CURVE ( 'NONE', #17976, #28529, #18856, .T. ) ;
#30438 = VERTEX_POINT ( 'NONE', #32245 ) ;
#30439 = CARTESIAN_POINT ( 'NONE',  ( -26.00068869287340334, 59.40885416666666430, 15.01150461594643382 ) ) ;
#30440 = VECTOR ( 'NONE', #31100, 1000.000000000000000 ) ;
#30441 = CARTESIAN_POINT ( 'NONE',  ( -12.13525491562421088, 75.80000000000003979, -8.816778784387096835 ) ) ;
#30442 = CARTESIAN_POINT ( 'NONE',  ( -33.58253175000000113, 67.02500000273117564, -10.91162601494193218 ) ) ;
#30443 = CARTESIAN_POINT ( 'NONE',  ( 26.00068869287367335, 41.07552083333331439, 15.01150461594596308 ) ) ;
#30444 = CARTESIAN_POINT ( 'NONE',  ( 19.82091636218621389, 12.19999999999998863, -14.40073868116559197 ) ) ;
#30445 = CARTESIAN_POINT ( 'NONE',  ( 20.75514604977248467, 4.675000002731176885, -28.56700777964554305 ) ) ;
#30446 = CARTESIAN_POINT ( 'NONE',  ( -2.162160676586881955E-15, 10.62500000273119127, -35.31076352940723240 ) ) ;
#30447 = CARTESIAN_POINT ( 'NONE',  ( 2.688165632520823219E-15, 73.37500000273118417, 14.63369212191046209 ) ) ;
#30448 = CARTESIAN_POINT ( 'NONE',  ( 26.02091320914876960, 53.38763916574269786, 14.97647472619900455 ) ) ;
#30449 = CARTESIAN_POINT ( 'NONE',  ( 12.13525491562420910, 77.19999999999998863, -8.816778784387098611 ) ) ;
#30450 = CARTESIAN_POINT ( 'NONE',  ( -7.505752307973343918, 56.97395833333333570, -28.01184896238290989 ) ) ;
#30451 = CARTESIAN_POINT ( 'NONE',  ( 0.000000000000000000, -23.00000000000000000, 0.000000000000000000 ) ) ;
#30452 = CARTESIAN_POINT ( 'NONE',  ( 20.08610463437158344, 61.20000000546237118, 27.64615127144129403 ) ) ;
#30453 = CARTESIAN_POINT ( 'NONE',  ( -7.570916362186210335, 6.349999994537613546, -23.30088464923126779 ) ) ;
#30454 = CARTESIAN_POINT ( 'NONE',  ( -4.635254915624208216, 74.65000000546240244, 14.26584774442730463 ) ) ;
#30455 = CARTESIAN_POINT ( 'NONE',  ( 26.07999730980477437, 26.89583333333332860, -6.988114217768290004 ) ) ;
#30456 = CARTESIAN_POINT ( 'NONE',  ( -2.162160676586881955E-15, 36.62500000273119127, -35.31076352940723240 ) ) ;
#30457 = CARTESIAN_POINT ( 'NONE',  ( 4.300734207923761154, 71.47500000273116427, 13.23629886949340495 ) ) ;
#30458 = CARTESIAN_POINT ( 'NONE',  ( 33.58253175000000113, 44.37500000273119127, -4.112674001490185761E-15 ) ) ;
#30459 = CARTESIAN_POINT ( 'NONE',  ( -10.37757302488624411, 22.97500000273117138, -31.93888565452638417 ) ) ;
#30460 = CARTESIAN_POINT ( 'NONE',  ( -20.08610463437157989, 12.20000000546237828, -27.64615127144129758 ) ) ;
#30461 = CYLINDRICAL_SURFACE ( 'NONE', #25599, 24.50000000000000000 ) ;
#30462 = CARTESIAN_POINT ( 'NONE',  ( 12.13525491562420910, 81.19999999999998863, -8.816778784387098611 ) ) ;
#30463 = CARTESIAN_POINT ( 'NONE',  ( 26.29305231718579350, 66.80000000000001137, 19.10302069950537529 ) ) ;
#30464 = CARTESIAN_POINT ( 'NONE',  ( -7.236395654485763274, 8.024999997268800200, 22.27133577429736633 ) ) ;
#30465 = CARTESIAN_POINT ( 'NONE',  ( 7.543491769121922985, 22.87982666574268720, 28.00173670424535644 ) ) ;
#30466 = CARTESIAN_POINT ( 'NONE',  ( 10.17814985357209245, -45.51763809020504681, 1.246463863941915697E-15 ) ) ;
#30467 = CARTESIAN_POINT ( 'NONE',  ( -19.06425588902558133, 37.20274333240935505, 19.11951029504797006 ) ) ;
#30468 = CARTESIAN_POINT ( 'NONE',  ( 33.58253175000000823, 78.27500000273116143, 10.91162601494192863 ) ) ;
#30469 = CARTESIAN_POINT ( 'NONE',  ( 33.58253175000000113, 10.12500000273119838, -4.112674001490185761E-15 ) ) ;
#30470 = CARTESIAN_POINT ( 'NONE',  ( 14.47279130897151767, 15.42499999726882898, -19.92008829642072598 ) ) ;
#30471 = CARTESIAN_POINT ( 'NONE',  ( 24.20753774853731244, 64.56510416666667140, -13.97622843553632599 ) ) ;
#30472 = ORIENTED_EDGE ( 'NONE', *, *, #19118, .F. ) ;
#30473 = CARTESIAN_POINT ( 'NONE',  ( -10.37757302488624411, 46.72500000273120691, -31.93888565452638417 ) ) ;
#30474 = CARTESIAN_POINT ( 'NONE',  ( 6.486482029760649416E-15, 23.87500000273117706, 35.31076352940723240 ) ) ;
#30475 = ORIENTED_EDGE ( 'NONE', *, *, #6564, .T. ) ;
#30476 = CARTESIAN_POINT ( 'NONE',  ( 30.02300923189239512, 37.35156249999997868, -2.619432448724977703E-13 ) ) ;
#30477 = CARTESIAN_POINT ( 'NONE',  ( -14.97647472619946285, 30.76861083425731280, -26.02091320914851025 ) ) ;
#30478 = CARTESIAN_POINT ( 'NONE',  ( -19.82091636218621389, 8.949999994537632730, 14.40073868116558842 ) ) ;
#30479 = CARTESIAN_POINT ( 'NONE',  ( 15.14183272437241889, 13.44999999453762385, 20.84094480462498211 ) ) ;
#30480 = CARTESIAN_POINT ( 'NONE',  ( 23.41746824999999887, 10.62499999726881938, 0.000000000000000000 ) ) ;
#30481 = CARTESIAN_POINT ( 'NONE',  ( 33.58253175000000113, 24.47500000273118914, -10.91162601494193751 ) ) ;
#30482 = CARTESIAN_POINT ( 'NONE',  ( -26.29305231718578995, 22.70000000546237828, 19.10302069950538595 ) ) ;
#30483 = CARTESIAN_POINT ( 'NONE',  ( -26.29305231718579350, 67.79999999999999716, -19.10302069950537884 ) ) ;
#30484 = CARTESIAN_POINT ( 'NONE',  ( 5.147494310547434893, 47.05125428700922896, 32.49999999999999289 ) ) ;
#30485 = CARTESIAN_POINT ( 'NONE',  ( -13.62972974288548933, 74.00000000000002842, 5.724431369363315092 ) ) ;
#30486 = CARTESIAN_POINT ( 'NONE',  ( -26.00068869287340334, 14.72135416666666607, 15.01150461594643382 ) ) ;
#30487 = CARTESIAN_POINT ( 'NONE',  ( -20.75514604977248823, 37.07500000273120122, -28.56700777964554305 ) ) ;
#30488 = DIRECTION ( 'NONE',  ( -0.000000000000000000, -1.000000000000000000, -0.000000000000000000 ) ) ;
#30489 = CARTESIAN_POINT ( 'NONE',  ( -26.00068869287368756, 32.48177083333332860, -15.01150461594595775 ) ) ;
#30490 = AXIS2_PLACEMENT_3D ( 'NONE', #8686, #19170, #1973 ) ;
#30491 = CARTESIAN_POINT ( 'NONE',  ( -23.41746825000000598, 16.22499999726880304, 7.608796670333726198 ) ) ;
#30492 = CARTESIAN_POINT ( 'NONE',  ( -32.50000000000000000, 16.10000000000001563, 10.55989012756946366 ) ) ;
#30493 = CARTESIAN_POINT ( 'NONE',  ( -19.82091636218621389, 15.19999999999999218, 14.40073868116558842 ) ) ;
#30494 = CARTESIAN_POINT ( 'NONE',  ( 19.06425588902558133, 42.35899333240935505, -19.11951029504797006 ) ) ;
#30495 = CARTESIAN_POINT ( 'NONE',  ( -20.75514604977248823, 54.82500000273118701, -28.56700777964554305 ) ) ;
#30496 = CARTESIAN_POINT ( 'NONE',  ( -33.58253175000000113, 63.27500000273118985, -10.91162601494193218 ) ) ;
#30497 = CARTESIAN_POINT ( 'NONE',  ( 6.486482029760648627E-15, 45.87500000273118417, 35.31076352940722529 ) ) ;
#30498 = CARTESIAN_POINT ( 'NONE',  ( 0.000000000000000000, 16.99999999999998579, -24.50000000000000000 ) ) ;
#30499 = CARTESIAN_POINT ( 'NONE',  ( 32.50000000000000000, 67.60000000546237686, -10.55989012756945833 ) ) ;
#30500 = CARTESIAN_POINT ( 'NONE',  ( 4.349545668204547685E-15, -58.51673569255127205, 0.000000000000000000 ) ) ;
#30501 = CARTESIAN_POINT ( 'NONE',  ( -6.950374756619716266, 48.09934000092398065, -26.09010956794232428 ) ) ;
#30502 =( BOUNDED_CURVE ( )  B_SPLINE_CURVE ( 2, ( #33070, #22446, #7518, #27770, #9392, #28448, #12144, #25021, #19876, #14901, #22617, #9576, #20053 ),
 .UNSPECIFIED., .F., .F. ) 
 B_SPLINE_CURVE_WITH_KNOTS ( ( 3, 2, 2, 2, 2, 2, 3 ),
 ( 0.4423076923076922906, 0.4435897435897435681, 0.4461538461538461786, 0.4487179487179487336, 0.4512820512820512886, 0.4538461538461538436, 0.4551282051282051211 ),
 .UNSPECIFIED. ) 
 CURVE ( )  GEOMETRIC_REPRESENTATION_ITEM ( )  RATIONAL_B_SPLINE_CURVE ( ( 0.9755282581475768211, 0.9755282581475768211, 1.000000000000000000, 0.9510565162951535312, 1.000000000000000000, 0.9510565162951535312, 1.000000000000000000, 0.9510565162951535312, 1.000000000000000000, 0.9510565162951535312, 1.000000000000000000, 0.9755282581475768211, 0.9755282581475768211 ) ) 
 REPRESENTATION_ITEM ( '' )  );
#30503 = CARTESIAN_POINT ( 'NONE',  ( 32.50000000000000711, 63.40000000546236691, 10.55989012756945122 ) ) ;
#30504 = CARTESIAN_POINT ( 'NONE',  ( -32.50000000000000000, 42.00000000000000711, 0.000000000000000000 ) ) ;
#30505 = CARTESIAN_POINT ( 'NONE',  ( 27.16883889988623935, 24.32500000273117635, -19.73931689729374384 ) ) ;
#30506 = CARTESIAN_POINT ( 'NONE',  ( 5.147494310547481966, 67.44874571845315359, -32.49999999999998579 ) ) ;
#30507 = CARTESIAN_POINT ( 'NONE',  ( 5.147494310547426899, 53.44874571845314648, -32.50000000000000000 ) ) ;
#30508 = CARTESIAN_POINT ( 'NONE',  ( -32.50000000000000000, 78.50000000546236834, 0.000000000000000000 ) ) ;
#30509 = CARTESIAN_POINT ( 'NONE',  ( 15.04653450569339945, 60.54909749907603356, 25.98046417659831775 ) ) ;
#30510 = CARTESIAN_POINT ( 'NONE',  ( 32.50000000000000000, 43.50000000546237544, -3.980102097228898626E-15 ) ) ;
#30511 = LINE ( 'NONE', #7180, #5760 ) ;
#30512 = CARTESIAN_POINT ( 'NONE',  ( 27.16883889988624290, 31.92500000273118488, 19.73931689729373673 ) ) ;
#30513 = CARTESIAN_POINT ( 'NONE',  ( 33.58253175000000113, 64.47500000273120691, -10.91162601494193751 ) ) ;
#30514 = CARTESIAN_POINT ( 'NONE',  ( -26.07999730980490583, 39.21354166666666430, -6.988114217767815717 ) ) ;
#30515 = ORIENTED_EDGE ( 'NONE', *, *, #13660, .F. ) ;
#30516 = CARTESIAN_POINT ( 'NONE',  ( -33.58253175000000113, 69.02500000273118985, -10.91162601494193218 ) ) ;
#30517 = CARTESIAN_POINT ( 'NONE',  ( -26.00068869287340334, 38.78385416666665719, 15.01150461594643382 ) ) ;
#30518 = CARTESIAN_POINT ( 'NONE',  ( 5.878266837044421923E-15, -70.99969134886156041, 0.000000000000000000 ) ) ;
#30519 = ORIENTED_EDGE ( 'NONE', *, *, #23725, .T. ) ;
#30520 = CARTESIAN_POINT ( 'NONE',  ( -20.47846945139902175, 58.12538166759063785, -20.53372385742072481 ) ) ;
#30521 = CARTESIAN_POINT ( 'NONE',  ( -20.47846945139902175, 10.00038166759064140, -20.53372385742072481 ) ) ;
#30522 = CARTESIAN_POINT ( 'NONE',  ( -20.75514604977248112, 11.42500000273117955, 28.56700777964554661 ) ) ;
#30523 = AXIS2_PLACEMENT_3D ( 'NONE', #17538, #4657, #9808 ) ;
#30524 = CARTESIAN_POINT ( 'NONE',  ( -26.02091320914878025, 17.29388916574268720, -14.97647472619899389 ) ) ;
#30525 = CARTESIAN_POINT ( 'NONE',  ( 9.270509831248421762, 79.55000000546240813, -12.75976212528059861 ) ) ;
#30526 = CARTESIAN_POINT ( 'NONE',  ( -33.58253175000000113, 39.27500000273118275, -10.91162601494193218 ) ) ;
#30527 = CARTESIAN_POINT ( 'NONE',  ( -10.04305231718579172, 46.10000000546238397, -30.90933677959248982 ) ) ;
#30528 = EDGE_CURVE ( 'NONE', #29627, #1345, #18113, .T. ) ;
#30529 = CARTESIAN_POINT ( 'NONE',  ( 4.635254915624209993, 81.39999999999997726, -14.26584774442730463 ) ) ;
#30530 = CARTESIAN_POINT ( 'NONE',  ( 33.58253175000000823, 28.02500000273119340, 10.91162601494192863 ) ) ;
#30531 = CARTESIAN_POINT ( 'NONE',  ( 20.08610463437158344, 31.20000000546238894, 27.64615127144129403 ) ) ;
#30532 = CARTESIAN_POINT ( 'NONE',  ( -33.58253175000000113, 57.47500000273119269, 10.91162601494193929 ) ) ;
#30533 = EDGE_CURVE ( 'NONE', #22307, #17621, #8903, .T. ) ;
#30534 = CARTESIAN_POINT ( 'NONE',  ( -26.29305231718579350, 37.79999999999998295, -19.10302069950537884 ) ) ;
#30535 = CARTESIAN_POINT ( 'NONE',  ( 26.29305231718578995, 35.20000000000000995, -19.10302069950538240 ) ) ;
#30536 = CARTESIAN_POINT ( 'NONE',  ( -7.236395654485763274, 18.02499999726880731, 22.27133577429736633 ) ) ;
#30537 = CARTESIAN_POINT ( 'NONE',  ( -33.58253175000000113, 75.02500000273117564, -10.91162601494193218 ) ) ;
#30538 = DIRECTION ( 'NONE',  ( -1.000000000000000000, -1.224646799147353454E-16, 0.000000000000000000 ) ) ;
#30539 = CARTESIAN_POINT ( 'NONE',  ( -32.50000000000000000, 20.40000000546238468, -10.55989012756945300 ) ) ;
#30540 = CARTESIAN_POINT ( 'NONE',  ( 33.58253175000000113, 66.37500000273119838, -4.112674001490185761E-15 ) ) ;
#30541 = CARTESIAN_POINT ( 'NONE',  ( 9.270509831248423538, 77.55000000546233707, -12.75976212528059861 ) ) ;
#30542 = EDGE_CURVE ( 'NONE', #25648, #20029, #28690, .T. ) ;
#30543 = VERTEX_POINT ( 'NONE', #5999 ) ;
#30544 = CARTESIAN_POINT ( 'NONE',  ( 10.37757302488624767, 17.72500000273119625, 31.93888565452638417 ) ) ;
#30545 = CARTESIAN_POINT ( 'NONE',  ( -24.50000000000000355, 10.64999999453762491, -7.960532557706207157 ) ) ;
#30546 = CARTESIAN_POINT ( 'NONE',  ( -24.18731323226248264, 16.73215250092398065, -14.01125832528284931 ) ) ;
#30547 = CARTESIAN_POINT ( 'NONE',  ( -5.147494310547423346, 26.44874571845315714, 32.50000000000000000 ) ) ;
#30548 = CARTESIAN_POINT ( 'NONE',  ( -2.162160676586881955E-15, 40.62500000273120548, -35.31076352940723240 ) ) ;
#30549 = CARTESIAN_POINT ( 'NONE',  ( 27.16883889988624290, 4.175000002731188431, 19.73931689729373673 ) ) ;
#30550 = CARTESIAN_POINT ( 'NONE',  ( -20.75514604977248823, 55.07500000273117990, -28.56700777964554305 ) ) ;
#30551 = CARTESIAN_POINT ( 'NONE',  ( -28.02196122052045268, 50.67746500092398065, 7.468012846824790607 ) ) ;
#30552 = CARTESIAN_POINT ( 'NONE',  ( -8.601468415847518756, 80.57500000273120122, -11.83890561707634603 ) ) ;
#30553 = CARTESIAN_POINT ( 'NONE',  ( -28.00173670424535644, 40.92670166574268364, 7.543491769121936308 ) ) ;
#30554 = CARTESIAN_POINT ( 'NONE',  ( -32.50000000000000000, 60.50000000546238965, 0.000000000000000000 ) ) ;
#30555 = CARTESIAN_POINT ( 'NONE',  ( 4.300734207923757602, 74.27500000273118985, -13.23629886949340673 ) ) ;
#30556 = CARTESIAN_POINT ( 'NONE',  ( -27.95245687107223986, 65.13243083240935505, 0.04044903255043252877 ) ) ;
#30557 = LINE ( 'NONE', #1555, #19262 ) ;
#30558 = CARTESIAN_POINT ( 'NONE',  ( -32.50000000000000000, 74.50000000546236834, 0.000000000000000000 ) ) ;
#30559 = CARTESIAN_POINT ( 'NONE',  ( -7.505752307972844761, 14.29166666666666430, 28.01184896238304134 ) ) ;
#30560 = CARTESIAN_POINT ( 'NONE',  ( 33.58253175000000823, 40.27500000273118985, 10.91162601494192863 ) ) ;
#30561 = CARTESIAN_POINT ( 'NONE',  ( -18.94512977948576093, 10.32499999726882400, 13.76444248337722698 ) ) ;
#30562 = VERTEX_POINT ( 'NONE', #24528 ) ;
#30563 = CARTESIAN_POINT ( 'NONE',  ( 10.37757302488624767, 77.97500000273119269, 31.93888565452638417 ) ) ;
#30564 = CARTESIAN_POINT ( 'NONE',  ( -32.50000000000000000, 26.60000000546239107, 10.55989012756946366 ) ) ;
#30565 = ORIENTED_EDGE ( 'NONE', *, *, #4418, .F. ) ;
#30566 = CARTESIAN_POINT ( 'NONE',  ( 28.01184896238304134, 30.61979166666666075, 7.505752307972846538 ) ) ;
#30567 = CARTESIAN_POINT ( 'NONE',  ( 20.08610463437157279, 63.80000000546237970, -27.64615127144129758 ) ) ;
#30568 = ORIENTED_EDGE ( 'NONE', *, *, #27898, .T. ) ;
#30569 = DIRECTION ( 'NONE',  ( 0.000000000000000000, -0.000000000000000000, -1.000000000000000000 ) ) ;
#30570 = CARTESIAN_POINT ( 'NONE',  ( -20.75514604977248112, 51.42500000273118133, 28.56700777964554661 ) ) ;
#30571 = CARTESIAN_POINT ( 'NONE',  ( -23.41746825000000243, 17.52499999726881796, -7.608796670333730638 ) ) ;
#30572 = CARTESIAN_POINT ( 'NONE',  ( -26.29305231718579350, 8.300000005462383257, -19.10302069950537884 ) ) ;
#30573 = CARTESIAN_POINT ( 'NONE',  ( -9.270509831248419985, 78.29999999999999716, 12.75976212528060039 ) ) ;
#30574 = CARTESIAN_POINT ( 'NONE',  ( 30.02300923189239867, 13.28906249999999467, -2.619432448724978208E-13 ) ) ;
#30575 = AXIS2_PLACEMENT_3D ( 'NONE', #21694, #32638, #29896 ) ;
#30576 = CARTESIAN_POINT ( 'NONE',  ( 10.04305231718579705, 50.60000000000000853, 30.90933677959248982 ) ) ;
#30577 = DIRECTION ( 'NONE',  ( 0.000000000000000000, 0.000000000000000000, -1.000000000000000000 ) ) ;
#30578 = CARTESIAN_POINT ( 'NONE',  ( 6.486482029760649416E-15, 17.87500000273119838, 35.31076352940723240 ) ) ;
#30579 = DIRECTION ( 'NONE',  ( 0.8660254037844399289, -0.4999999999999977240, 0.000000000000000000 ) ) ;
#30580 = CARTESIAN_POINT ( 'NONE',  ( -14.01125832528328985, 27.89284749907601935, -24.18731323226223040 ) ) ;
#30581 = CARTESIAN_POINT ( 'NONE',  ( 13.91746824999999887, 76.37500000273116996, -1.704398294459741270E-15 ) ) ;
#30582 = CARTESIAN_POINT ( 'NONE',  ( -32.50000000000000000, 56.10000000000000142, 10.55989012756946366 ) ) ;
#30583 = DIRECTION ( 'NONE',  ( -0.5000000000000001110, 0.000000000000000000, 0.8660254037844387076 ) ) ;
#30584 = CARTESIAN_POINT ( 'NONE',  ( -26.29305231718578995, 4.199999999999995737, 19.10302069950538595 ) ) ;
#30585 = VERTEX_POINT ( 'NONE', #13900 ) ;
#30586 = CARTESIAN_POINT ( 'NONE',  ( -7.236395654485763274, 10.52499999726880198, 22.27133577429736633 ) ) ;
#30587 = CARTESIAN_POINT ( 'NONE',  ( 5.147494310547453544, 71.94874572391553613, -32.49999999999999289 ) ) ;
#30588 = CARTESIAN_POINT ( 'NONE',  ( -6.988114217768288228, 53.53645833333332860, -26.07999730980477437 ) ) ;
#30589 = CARTESIAN_POINT ( 'NONE',  ( 27.16883889988623935, 62.32500000273120833, -19.73931689729374384 ) ) ;
#30590 = CARTESIAN_POINT ( 'NONE',  ( 33.58253175000000823, 22.27500000273116854, 10.91162601494192863 ) ) ;
#30591 = CARTESIAN_POINT ( 'NONE',  ( 20.75514604977248467, 10.67500000273119021, -28.56700777964554305 ) ) ;
#30592 = FACE_OUTER_BOUND ( 'NONE', #15825, .T. ) ;
#30593 = CARTESIAN_POINT ( 'NONE',  ( 26.02091320914851025, 17.87798583425730570, -14.97647472619946463 ) ) ;
#30594 = CARTESIAN_POINT ( 'NONE',  ( -15.01150461594595775, 65.99739583333334281, 26.00068869287368756 ) ) ;
#30595 = CARTESIAN_POINT ( 'NONE',  ( 20.08610463437158344, 77.20000000546238539, 27.64615127144129403 ) ) ;
#30596 = EDGE_CURVE ( 'NONE', #5893, #20206, #26723, .T. ) ;
#30597 = LINE ( 'NONE', #7092, #33023 ) ;
#30598 = CARTESIAN_POINT ( 'NONE',  ( -10.04305231718579172, 43.60000000000001563, -30.90933677959248982 ) ) ;
#30599 = CARTESIAN_POINT ( 'NONE',  ( 10.37757302488624767, 43.72500000273119269, 31.93888565452638417 ) ) ;
#30600 = CARTESIAN_POINT ( 'NONE',  ( 23.41746824999999887, 2.624999997268812280, 0.000000000000000000 ) ) ;
#30601 = CARTESIAN_POINT ( 'NONE',  ( -8.891200544363830713E-16, 79.50000000000001421, -15.00000000000000000 ) ) ;
#30602 = ORIENTED_EDGE ( 'NONE', *, *, #23499, .T. ) ;
#30603 = CARTESIAN_POINT ( 'NONE',  ( 33.58253175000000113, 60.37500000273120548, -4.112674001490185761E-15 ) ) ;
#30604 = CARTESIAN_POINT ( 'NONE',  ( -20.08610463437157989, 4.200000005462371178, -27.64615127144129758 ) ) ;
#30605 = CARTESIAN_POINT ( 'NONE',  ( 23.41746824999999887, 12.62499999726882116, 0.000000000000000000 ) ) ;
#30606 = CARTESIAN_POINT ( 'NONE',  ( 27.95245687107223986, 35.35194416759064495, 0.04044903254993640479 ) ) ;
#30607 = EDGE_LOOP ( 'NONE', ( #32459, #2900, #22460, #6539 ) ) ;
#30608 = CARTESIAN_POINT ( 'NONE',  ( -27.16883889988623935, 31.32500000273118346, 19.73931689729374739 ) ) ;
#30609 = CARTESIAN_POINT ( 'NONE',  ( -1.778240108872766143E-15, 70.00000000546238255, -32.49999999999999289 ) ) ;
#30610 = VERTEX_POINT ( 'NONE', #19387 ) ;
#30611 = DIRECTION ( 'NONE',  ( 0.000000000000000000, -0.000000000000000000, 1.000000000000000000 ) ) ;
#30612 = CARTESIAN_POINT ( 'NONE',  ( 20.75514604977248467, 68.42500000273120975, -28.56700777964554305 ) ) ;
#30613 = CARTESIAN_POINT ( 'NONE',  ( -26.00068869287340334, 38.78385416666665719, 15.01150461594643382 ) ) ;
#30614 = CARTESIAN_POINT ( 'NONE',  ( 15.14183272437242245, 12.29999999999999183, -20.84094480462497856 ) ) ;
#30615 = CARTESIAN_POINT ( 'NONE',  ( 1.507698388325705758E-15, 1.624999997268798735, -24.62258325217400312 ) ) ;
#30616 = CARTESIAN_POINT ( 'NONE',  ( 33.58253175000000113, 12.22500000273120158, -10.91162601494193751 ) ) ;
#30617 =( NAMED_UNIT ( * ) SI_UNIT ( $, .STERADIAN. ) SOLID_ANGLE_UNIT ( ) );
#30618 = CARTESIAN_POINT ( 'NONE',  ( 7.543491769121922985, 57.25482666574269075, 28.00173670424535644 ) ) ;
#30619 = CARTESIAN_POINT ( 'NONE',  ( 9.270509831248423538, 75.30000000000001137, -12.75976212528059861 ) ) ;
#30620 = CARTESIAN_POINT ( 'NONE',  ( -30.02300923189239867, 59.69531250000000711, 2.654126918244514854E-13 ) ) ;
#30621 = DIRECTION ( 'NONE',  ( -1.224646799147353454E-16, 1.000000000000000000, -0.000000000000000000 ) ) ;
#30622 = CARTESIAN_POINT ( 'NONE',  ( -12.13525491562420910, 74.45000000546237118, 8.816778784387098611 ) ) ;
#30623 = CARTESIAN_POINT ( 'NONE',  ( -4.732186688966233175E-15, 15.24999999453762811, 25.76082449383753925 ) ) ;
#30624 = CARTESIAN_POINT ( 'NONE',  ( -4.635254915624211769, 75.85000000546237686, -14.26584774442730286 ) ) ;
#30625 = CARTESIAN_POINT ( 'NONE',  ( -19.09188309203694445, 18.87499999999999645, -19.09188309203661049 ) ) ;
#30626 = CARTESIAN_POINT ( 'NONE',  ( -27.16883889988624290, 34.92500000273118843, -19.73931689729374028 ) ) ;
#30627 = CARTESIAN_POINT ( 'NONE',  ( 15.00000000000000355, 74.90000000000001990, 4.873795443493592394 ) ) ;
#30628 = CARTESIAN_POINT ( 'NONE',  ( 20.75514604977249178, 44.07500000273117990, 28.56700777964553950 ) ) ;
#30629 = CARTESIAN_POINT ( 'NONE',  ( 20.75514604977249178, 22.07500000273117990, 28.56700777964553950 ) ) ;
#30630 = DIRECTION ( 'NONE',  ( -1.224646799147353454E-16, 1.000000000000000000, -0.000000000000000000 ) ) ;
#30631 = CARTESIAN_POINT ( 'NONE',  ( 1.555960095263670572E-15, 14.24999999453762278, -24.50000000000000000 ) ) ;
#30632 = ADVANCED_FACE ( 'NONE', ( #29836 ), #505, .T. ) ;
#30633 = CARTESIAN_POINT ( 'NONE',  ( 20.08610463437158344, 32.69999999999998863, 27.64615127144129403 ) ) ;
#30634 = CARTESIAN_POINT ( 'NONE',  ( 10.04305231718578817, 57.39999999999999147, -30.90933677959249337 ) ) ;
#30635 = CARTESIAN_POINT ( 'NONE',  ( 18.94512977948576093, 10.82499999726882578, -13.76444248337722875 ) ) ;
#30636 = CARTESIAN_POINT ( 'NONE',  ( 20.75514604977249178, 63.82500000273119412, 28.56700777964553950 ) ) ;
#30637 = ADVANCED_FACE ( 'NONE', ( #27270 ), #29336, .T. ) ;
#30638 = CARTESIAN_POINT ( 'NONE',  ( 2.667360163309149608E-15, 79.50000000000000000, -32.50000000000000000 ) ) ;
#30639 = CARTESIAN_POINT ( 'NONE',  ( -27.95245687107223986, 41.06993083240934794, 0.04044903255043252877 ) ) ;
#30640 = CARTESIAN_POINT ( 'NONE',  ( 33.58253175000000113, 12.22500000273119980, -10.91162601494193574 ) ) ;
#30641 = CARTESIAN_POINT ( 'NONE',  ( 7.236395654485760609, 9.524999997268801977, -22.27133577429736633 ) ) ;
#30642 = CARTESIAN_POINT ( 'NONE',  ( -26.07999730980490583, 66.71354166666665719, -6.988114217767815717 ) ) ;
#30643 = ORIENTED_EDGE ( 'NONE', *, *, #18179, .F. ) ;
#30644 = CARTESIAN_POINT ( 'NONE',  ( 20.75514604977249178, 47.82500000273117990, 28.56700777964553950 ) ) ;
#30645 = CARTESIAN_POINT ( 'NONE',  ( -2.162160676586881955E-15, 22.87500000273118062, -35.31076352940723240 ) ) ;
#30646 = VERTEX_POINT ( 'NONE', #14235 ) ;
#30647 = CARTESIAN_POINT ( 'NONE',  ( 15.01150461594596308, 33.34114583333332860, -26.00068869287367335 ) ) ;
#30648 = CARTESIAN_POINT ( 'NONE',  ( 20.47846945139902530, 32.34413166759064495, 20.53372385742071771 ) ) ;
#30649 = FACE_OUTER_BOUND ( 'NONE', #6519, .T. ) ;
#30650 = CARTESIAN_POINT ( 'NONE',  ( -3.880418787951136483, 8.301254276084460315, -24.50000000000000000 ) ) ;
#30651 = CARTESIAN_POINT ( 'NONE',  ( -14.47279130897151589, 1.824999997268821339, -19.92008829642072598 ) ) ;
#30652 = CARTESIAN_POINT ( 'NONE',  ( 14.47279130897151767, 10.92499999726882365, -19.92008829642072598 ) ) ;
#30653 = CARTESIAN_POINT ( 'NONE',  ( 27.16883889988623935, 20.57500000273118701, -19.73931689729374384 ) ) ;
#30654 = CARTESIAN_POINT ( 'NONE',  ( 20.08610463437157279, 23.80000000546235839, -27.64615127144129758 ) ) ;
#30655 = CARTESIAN_POINT ( 'NONE',  ( -20.08610463437157989, 63.69999999999998863, -27.64615127144129758 ) ) ;
#30656 = CARTESIAN_POINT ( 'NONE',  ( -7.570916362186210335, 4.599999999999992539, -23.30088464923126779 ) ) ;
#30657 = CARTESIAN_POINT ( 'NONE',  ( -13.75194420523858341, 74.00000000000004263, 5.454580986648785768 ) ) ;
#30658 = CARTESIAN_POINT ( 'NONE',  ( -26.02091320914849959, 60.84673583425731636, 14.97647472619947528 ) ) ;
#30659 = CARTESIAN_POINT ( 'NONE',  ( 10.37757302488624767, 27.97500000273117493, 31.93888565452638417 ) ) ;
#30660 = CARTESIAN_POINT ( 'NONE',  ( -13.91746824999999532, 81.27500000273120406, -4.522059556121115875 ) ) ;
#30661 = CARTESIAN_POINT ( 'NONE',  ( 7.505752307973351023, 34.63020833333332860, 28.01184896238290278 ) ) ;
#30662 =( NAMED_UNIT ( * ) SI_UNIT ( $, .STERADIAN. ) SOLID_ANGLE_UNIT ( ) );
#30663 = CARTESIAN_POINT ( 'NONE',  ( -3.880418787951136039, 0.5512542815468468582, -24.50000000000000000 ) ) ;
#30664 = CARTESIAN_POINT ( 'NONE',  ( 20.08610463437157279, 11.29999999999999361, -27.64615127144129758 ) ) ;
#30665 = CARTESIAN_POINT ( 'NONE',  ( 10.04305231718578817, 9.900000005462372243, -30.90933677959249337 ) ) ;
#30666 = CARTESIAN_POINT ( 'NONE',  ( -14.01125832528328985, 55.39284749907604066, -24.18731323226223040 ) ) ;
#30667 = CARTESIAN_POINT ( 'NONE',  ( 27.16883889988624290, 57.92500000273120975, 19.73931689729373673 ) ) ;
#30668 = CARTESIAN_POINT ( 'NONE',  ( 33.58253175000000113, 64.47500000273120691, -10.91162601494193751 ) ) ;
#30669 = CARTESIAN_POINT ( 'NONE',  ( 33.58253175000000113, 38.47500000273118559, -10.91162601494193574 ) ) ;
#30670 = CARTESIAN_POINT ( 'NONE',  ( 8.998893468610761559, 16.99999999999998579, -21.61938333025141290 ) ) ;
#30671 = CARTESIAN_POINT ( 'NONE',  ( 20.08610463437157279, 67.80000000546236549, -27.64615127144129758 ) ) ;
#30672 = CARTESIAN_POINT ( 'NONE',  ( -26.29305231718578995, 6.199999999999983302, 19.10302069950538595 ) ) ;
#30673 = CARTESIAN_POINT ( 'NONE',  ( 13.94119854578937812, 49.67486083425730925, 24.22776226481240514 ) ) ;
#30674 = CARTESIAN_POINT ( 'NONE',  ( -24.11383999230005415, 17.00000000000000355, -3.930170939105292138 ) ) ;
#30675 = CARTESIAN_POINT ( 'NONE',  ( -5.147494310547423346, 28.44874571845315714, 32.50000000000000000 ) ) ;
#30676 = CARTESIAN_POINT ( 'NONE',  ( 33.58253175000000823, 24.02500000273117564, 10.91162601494192863 ) ) ;
#30677 = CYLINDRICAL_SURFACE ( 'NONE', #5642, 32.50000000000000000 ) ;
#30678 = CARTESIAN_POINT ( 'NONE',  ( 32.50000000000000000, 55.50000000546238965, -3.980102097228898626E-15 ) ) ;
#30679 = DIRECTION ( 'NONE',  ( -0.000000000000000000, -1.000000000000000000, -0.000000000000000000 ) ) ;
#30680 = CARTESIAN_POINT ( 'NONE',  ( -28.00173670424535644, 68.42670166574269786, 7.543491769121936308 ) ) ;
#30681 = CARTESIAN_POINT ( 'NONE',  ( -32.50000000000000000, 42.40000000546238823, -10.55989012756945478 ) ) ;
#30682 = CARTESIAN_POINT ( 'NONE',  ( 10.04305231718578817, 11.39999999999999325, -30.90933677959249337 ) ) ;
#30683 = CARTESIAN_POINT ( 'NONE',  ( 20.75514604977249178, 29.82500000273119767, 28.56700777964553950 ) ) ;
#30684 = CARTESIAN_POINT ( 'NONE',  ( -10.37757302488623701, 63.77500000273117564, 31.93888565452638417 ) ) ;
#30685 = CARTESIAN_POINT ( 'NONE',  ( -26.07999730980490583, 35.77604166666666430, -6.988114217767815717 ) ) ;
#30686 = VERTEX_POINT ( 'NONE', #19555 ) ;
#30687 =( REPRESENTATION_RELATIONSHIP ('NONE','NONE', #5873, #15301 ) REPRESENTATION_RELATIONSHIP_WITH_TRANSFORMATION ( #13166 )SHAPE_REPRESENTATION_RELATIONSHIP( ) );
#30688 = CARTESIAN_POINT ( 'NONE',  ( 20.75514604977248467, 70.42500000273119554, -28.56700777964554305 ) ) ;
#30689 = CARTESIAN_POINT ( 'NONE',  ( 20.50609665440969565, 36.92187499999999289, -20.50609665441004736 ) ) ;
#30690 = DIRECTION ( 'NONE',  ( -0.000000000000000000, 1.000000000000000000, -0.000000000000000000 ) ) ;
#30691 = ORIENTED_EDGE ( 'NONE', *, *, #26853, .T. ) ;
#30692 = CARTESIAN_POINT ( 'NONE',  ( -25.98046417659859486, 57.98215250092397355, -15.04653450569291628 ) ) ;
#30693 = CARTESIAN_POINT ( 'NONE',  ( -13.94119854578936923, 58.26861083425732346, -24.22776226481241224 ) ) ;
#30694 = CARTESIAN_POINT ( 'NONE',  ( 33.58253175000000113, 14.12500000273118950, -4.112674001490185761E-15 ) ) ;
#30695 = EDGE_CURVE ( 'NONE', #30610, #13948, #2781, .T. ) ;
#30696 = CARTESIAN_POINT ( 'NONE',  ( 7.543491769121922985, 19.44232666574268364, 28.00173670424535644 ) ) ;
#30697 = CARTESIAN_POINT ( 'NONE',  ( 0.000000000000000000, 80.00000000000001421, -32.50000000000000000 ) ) ;
#30698 = CARTESIAN_POINT ( 'NONE',  ( -33.58253175000000113, 39.37500000273119838, 0.000000000000000000 ) ) ;
#30699 = CARTESIAN_POINT ( 'NONE',  ( 32.50000000000000711, 41.40000000546238823, 10.55989012756945122 ) ) ;
#30700 = EDGE_CURVE ( 'NONE', #25961, #29507, #7321, .T. ) ;
#30701 = CARTESIAN_POINT ( 'NONE',  ( -15.00000000000000000, 79.89999999999997726, -4.873795443493594171 ) ) ;
#30702 = CARTESIAN_POINT ( 'NONE',  ( -33.58253175000000113, 23.22500000273117138, 10.91162601494193929 ) ) ;
#30703 = CARTESIAN_POINT ( 'NONE',  ( 1.555960095263670572E-15, 16.24999999453762101, -24.50000000000000000 ) ) ;
#30704 = CARTESIAN_POINT ( 'NONE',  ( 10.37757302488624767, 55.97500000273119980, 31.93888565452638417 ) ) ;
#30705 = PRODUCT_CONTEXT ( 'NONE', #6790, 'mechanical' ) ;
#30706 = CARTESIAN_POINT ( 'NONE',  ( 20.08610463437158344, 26.70000000000000284, 27.64615127144129403 ) ) ;
#30707 = CARTESIAN_POINT ( 'NONE',  ( 32.50000000000000000, 27.09999999999999076, -10.55989012756945833 ) ) ;
#30708 = CARTESIAN_POINT ( 'NONE',  ( -7.236395654485763274, 16.02499999726880731, 22.27133577429736633 ) ) ;
#30709 =( BOUNDED_CURVE ( )  B_SPLINE_CURVE ( 2, ( #14027, #963, #3888, #11444, #14360, #21920, #469, #6296, #10952, #16772, #8363, #28249, #4226 ),
 .UNSPECIFIED., .F., .T. ) 
 B_SPLINE_CURVE_WITH_KNOTS ( ( 3, 2, 2, 2, 2, 2, 3 ),
 ( 0.4722222222222222654, 0.4777777777777778012, 0.4888888888888888729, 0.5000000000000000000, 0.5111111111111110716, 0.5222222222222222543, 0.5277777777777777901 ),
 .UNSPECIFIED. ) 
 CURVE ( )  GEOMETRIC_REPRESENTATION_ITEM ( )  RATIONAL_B_SPLINE_CURVE ( ( 0.9755282581475767101, 0.9755282581475768211, 1.000000000000000000, 0.9510565162951535312, 1.000000000000000000, 0.9510565162951535312, 1.000000000000000000, 0.9510565162951535312, 1.000000000000000000, 0.9510565162951535312, 1.000000000000000000, 0.9755282581475768211, 0.9755282581475768211 ) ) 
 REPRESENTATION_ITEM ( '' )  );
#30710 = CARTESIAN_POINT ( 'NONE',  ( 20.75514604977248467, 76.42500000273118133, -28.56700777964554305 ) ) ;
#30711 = CARTESIAN_POINT ( 'NONE',  ( -20.08610463437157989, 70.20000000546237118, -27.64615127144129758 ) ) ;
#30712 = CARTESIAN_POINT ( 'NONE',  ( -15.14183272437242067, 14.70000000000000107, -20.84094480462497856 ) ) ;
#30713 = CARTESIAN_POINT ( 'NONE',  ( -33.58253175000000113, 61.37500000273119127, 0.000000000000000000 ) ) ;
#30714 = CARTESIAN_POINT ( 'NONE',  ( -9.657523855033125146E-16, 77.75000000546233991, -15.77193336357400710 ) ) ;
#30715 = ORIENTED_EDGE ( 'NONE', *, *, #549, .F. ) ;
#30716 = CARTESIAN_POINT ( 'NONE',  ( 33.58253175000000113, 18.22500000273118559, -10.91162601494193751 ) ) ;
#30717 = CARTESIAN_POINT ( 'NONE',  ( 7.570916362186213000, 8.149999994537637349, -23.30088464923126423 ) ) ;
#30718 = CARTESIAN_POINT ( 'NONE',  ( 19.11951029504763611, 17.73475666759064140, -19.06425588902591173 ) ) ;
#30719 = CARTESIAN_POINT ( 'NONE',  ( 5.147494310547426899, 47.44874571845313938, -32.50000000000000000 ) ) ;
#30720 = CARTESIAN_POINT ( 'NONE',  ( -27.16883889988624290, 40.92500000273118133, -19.73931689729374028 ) ) ;
#30721 = CARTESIAN_POINT ( 'NONE',  ( 27.16883889988624290, 6.175000002731190207, 19.73931689729373673 ) ) ;
#30722 = CARTESIAN_POINT ( 'NONE',  ( 20.75514604977248467, 58.67500000273118843, -28.56700777964554305 ) ) ;
#30723 = CARTESIAN_POINT ( 'NONE',  ( 28.02196122052045268, 45.52121500092397355, -7.468012846824774620 ) ) ;
#30724 = CARTESIAN_POINT ( 'NONE',  ( 24.50000000000000000, 6.100000000000011191, -7.960532557706203605 ) ) ;
#30725 = CARTESIAN_POINT ( 'NONE',  ( 15.04653450569339945, 39.92409749907602645, 25.98046417659831775 ) ) ;
#30726 = CARTESIAN_POINT ( 'NONE',  ( -26.29305231718579350, 60.30000000546238681, -19.10302069950537884 ) ) ;
#30727 = CARTESIAN_POINT ( 'NONE',  ( -13.91746824999999887, 74.87500000273116996, 0.000000000000000000 ) ) ;
#30728 = CARTESIAN_POINT ( 'NONE',  ( -6.950374756619247307, 67.85378499907602645, 26.09010956794245217 ) ) ;
#30729 = CARTESIAN_POINT ( 'NONE',  ( -23.41746825000000243, 2.024999997268815299, -7.608796670333730638 ) ) ;
#30730 = EDGE_CURVE ( 'NONE', #4339, #15184, #32575, .T. ) ;
#30731 = CARTESIAN_POINT ( 'NONE',  ( -33.58253175000000113, 1.225000002731198467, 10.91162601494193929 ) ) ;
#30732 = CARTESIAN_POINT ( 'NONE',  ( -30.02300923189239512, 15.00781249999999467, 2.654126918244515359E-13 ) ) ;
#30733 = CARTESIAN_POINT ( 'NONE',  ( -27.16883889988624290, 35.17500000273120264, -19.73931689729374028 ) ) ;
#30734 = CARTESIAN_POINT ( 'NONE',  ( 14.47279130897151767, 10.82499999726882756, 19.92008829642072953 ) ) ;
#30735 = EDGE_LOOP ( 'NONE', ( #18650, #32003, #6086, #29434 ) ) ;
#30736 = CARTESIAN_POINT ( 'NONE',  ( -27.16883889988624290, 77.17500000273119554, -19.73931689729374028 ) ) ;
#30737 = CARTESIAN_POINT ( 'NONE',  ( -32.50000000000000000, 20.40000000546238113, -10.55989012756945478 ) ) ;
#30738 = EDGE_CURVE ( 'NONE', #30951, #13542, #26773, .T. ) ;
#30739 = CARTESIAN_POINT ( 'NONE',  ( 30.02300923189239512, 44.22656249999997868, -2.619432448724977703E-13 ) ) ;
#30740 = CARTESIAN_POINT ( 'NONE',  ( -26.29305231718579350, 62.30000000546237260, -19.10302069950537884 ) ) ;
#30741 = VERTEX_POINT ( 'NONE', #17316 ) ;
#30742 = CARTESIAN_POINT ( 'NONE',  ( -7.570916362186215665, 13.14999999453761426, 23.30088464923126423 ) ) ;
#30743 = CARTESIAN_POINT ( 'NONE',  ( -33.58253175000000113, 49.12500000273117706, 0.000000000000000000 ) ) ;
#30744 = CARTESIAN_POINT ( 'NONE',  ( -18.94512977948576093, 15.82499999726880091, 13.76444248337722698 ) ) ;
#30745 = CIRCLE ( 'NONE', #32408, 30.00000000000004974 ) ;
#30746 = CARTESIAN_POINT ( 'NONE',  ( -32.50000000000000000, 4.500000005462356789, 0.000000000000000000 ) ) ;
#30747 = EDGE_CURVE ( 'NONE', #30034, #24911, #29117, .T. ) ;
#30748 = CARTESIAN_POINT ( 'NONE',  ( 7.890940483122900408E-14, 12.24999999453763166, -24.50000000000000000 ) ) ;
#30749 = CARTESIAN_POINT ( 'NONE',  ( 20.50609665440969565, 16.29687499999999645, -20.50609665441004736 ) ) ;
#30750 = CARTESIAN_POINT ( 'NONE',  ( -20.08610463437156923, 50.30000000000001137, 27.64615127144130113 ) ) ;
#30751 = CARTESIAN_POINT ( 'NONE',  ( -32.50000000000000000, 14.00000000000001243, 0.000000000000000000 ) ) ;
#30752 = CARTESIAN_POINT ( 'NONE',  ( -27.16883889988623935, 15.57500000273118168, 19.73931689729374739 ) ) ;
#30753 = CARTESIAN_POINT ( 'NONE',  ( -1.778240108872766143E-15, 24.00000000546237899, -32.49999999999999289 ) ) ;
#30754 = CARTESIAN_POINT ( 'NONE',  ( -6.950374756619247307, 26.60378499907601579, 26.09010956794245217 ) ) ;
#30755 = CARTESIAN_POINT ( 'NONE',  ( 13.91746824999999532, 76.47500000273117848, -4.522059556121118540 ) ) ;
#30756 = CARTESIAN_POINT ( 'NONE',  ( 2.375766604868043252, 75.69874572391552192, -14.99999999999999822 ) ) ;
#30757 = CARTESIAN_POINT ( 'NONE',  ( -20.08610463437156923, 44.29999999999999716, 27.64615127144130113 ) ) ;
#30758 = CARTESIAN_POINT ( 'NONE',  ( 32.50000000000000000, 5.000000000000004441, -3.980102097228898626E-15 ) ) ;
#30759 = ORIENTED_EDGE ( 'NONE', *, *, #9981, .T. ) ;
#30760 = CARTESIAN_POINT ( 'NONE',  ( 7.236395654485755280, 12.72499999726881015, 22.27133577429736988 ) ) ;
#30761 = CARTESIAN_POINT ( 'NONE',  ( 7.236395654485755280, 4.224999997268802154, 22.27133577429736988 ) ) ;
#30762 = CARTESIAN_POINT ( 'NONE',  ( 13.97622843553633665, 48.23697916666665719, 24.20753774853730889 ) ) ;
#30763 = CARTESIAN_POINT ( 'NONE',  ( 6.486482029760649416E-15, 59.62500000273118417, 35.31076352940723240 ) ) ;
#30764 = CARTESIAN_POINT ( 'NONE',  ( 10.37757302488624767, 23.97500000273118559, 31.93888565452638417 ) ) ;
#30765 = CARTESIAN_POINT ( 'NONE',  ( 6.486482029760649416E-15, 9.875000002731187720, 35.31076352940723240 ) ) ;
#30766 = CARTESIAN_POINT ( 'NONE',  ( -27.95245687107223276, 32.19531250000000000, 2.498001805406602216E-13 ) ) ;
#30767 = CARTESIAN_POINT ( 'NONE',  ( 10.37757302488624767, 3.975000002731182924, 31.93888565452638417 ) ) ;
#30768 = CARTESIAN_POINT ( 'NONE',  ( 20.47846945139902530, 18.59413166759064140, 20.53372385742071771 ) ) ;
#30769 = CARTESIAN_POINT ( 'NONE',  ( 15.01150461594596308, 64.27864583333332860, -26.00068869287367335 ) ) ;
#30770 = CARTESIAN_POINT ( 'NONE',  ( 10.04305231718578817, 77.90000000546235981, -30.90933677959249337 ) ) ;
#30771 = CARTESIAN_POINT ( 'NONE',  ( -1.778240108872766143E-15, 3.500000000000004441, -32.49999999999999289 ) ) ;
#30772 = CARTESIAN_POINT ( 'NONE',  ( -10.04305231718579172, 39.60000000000000853, -30.90933677959248982 ) ) ;
#30773 = CIRCLE ( 'NONE', #18726, 30.50000000000000000 ) ;
#30774 = CARTESIAN_POINT ( 'NONE',  ( 33.58253175000000113, 42.22500000273118559, -10.91162601494193574 ) ) ;
#30775 = CARTESIAN_POINT ( 'NONE',  ( 23.41746825000000243, 8.724999997268806595, -7.608796670333727974 ) ) ;
#30776 = DIRECTION ( 'NONE',  ( 1.224646799147353454E-16, -1.000000000000000000, 0.000000000000000000 ) ) ;
#30777 = ORIENTED_EDGE ( 'NONE', *, *, #32304, .F. ) ;
#30778 = CARTESIAN_POINT ( 'NONE',  ( 33.58253175000000113, 54.47500000273117138, -10.91162601494193751 ) ) ;
#30779 = CARTESIAN_POINT ( 'NONE',  ( -26.29305231718578995, 4.700000005462390718, 19.10302069950538595 ) ) ;
#30780 = CARTESIAN_POINT ( 'NONE',  ( -27.95245687107223986, 33.63319416759063785, -0.04044903254993292840 ) ) ;
#30781 = CARTESIAN_POINT ( 'NONE',  ( 33.58253175000000823, 78.27500000273116143, 10.91162601494192863 ) ) ;
#30782 = ORIENTED_EDGE ( 'NONE', *, *, #23495, .F. ) ;
#30783 = CARTESIAN_POINT ( 'NONE',  ( -33.58253175000000113, 29.12500000273120193, 0.000000000000000000 ) ) ;
#30784 = CARTESIAN_POINT ( 'NONE',  ( 26.00068869287367335, 17.01302083333332504, 15.01150461594596308 ) ) ;
#30785 = EDGE_LOOP ( 'NONE', ( #19273, #4356, #15439, #5000 ) ) ;
#30786 = CYLINDRICAL_SURFACE ( 'NONE', #11656, 24.50000000000000000 ) ;
#30787 = CARTESIAN_POINT ( 'NONE',  ( -33.58253175000000113, 69.12500000273119838, 0.000000000000000000 ) ) ;
#30788 = CARTESIAN_POINT ( 'NONE',  ( 28.01184896238304134, 37.49479166666666430, 7.505752307972846538 ) ) ;
#30789 = CARTESIAN_POINT ( 'NONE',  ( 15.14183272437241889, 9.700000000000013500, 20.84094480462498211 ) ) ;
#30790 = CARTESIAN_POINT ( 'NONE',  ( 14.47279130897151944, 5.424999997268823648, -19.92008829642072598 ) ) ;
#30791 = CARTESIAN_POINT ( 'NONE',  ( 6.486482029760649416E-15, 11.62500000273118950, 35.31076352940723240 ) ) ;
#30792 = CARTESIAN_POINT ( 'NONE',  ( 32.50000000000000000, 28.99999999999999645, -3.980102097228898626E-15 ) ) ;
#30793 = CARTESIAN_POINT ( 'NONE',  ( 28.00173670424535644, 49.52045166574269075, -7.543491769121920321 ) ) ;
#30794 = CARTESIAN_POINT ( 'NONE',  ( -15.00000000000000000, 72.00000000000001421, 0.000000000000000000 ) ) ;
#30795 = CARTESIAN_POINT ( 'NONE',  ( -26.00068869287368756, 66.85677083333332860, -15.01150461594595775 ) ) ;
#30796 = CARTESIAN_POINT ( 'NONE',  ( 32.50000000000000711, 19.40000000546238468, 10.55989012756945122 ) ) ;
#30797 = CARTESIAN_POINT ( 'NONE',  ( -1.778240108872766143E-15, 23.49999999999999645, -32.49999999999999289 ) ) ;
#30798 = CARTESIAN_POINT ( 'NONE',  ( -24.50000000000001066, 14.84999999453764019, 7.960532557706201828 ) ) ;
#30799 = CARTESIAN_POINT ( 'NONE',  ( 9.270509831248423538, 77.55000000546236549, -12.75976212528059861 ) ) ;
#30800 = CARTESIAN_POINT ( 'NONE',  ( -26.07999730980490583, 18.58854166666666430, -6.988114217767815717 ) ) ;
#30801 = CARTESIAN_POINT ( 'NONE',  ( -10.37757302488623701, 33.52500000273117564, 31.93888565452638417 ) ) ;
#30802 = CARTESIAN_POINT ( 'NONE',  ( -8.891200544363830713E-16, 73.75000000546239676, -15.00000000000000000 ) ) ;
#30803 = CARTESIAN_POINT ( 'NONE',  ( -33.58253175000000113, 45.27500000273116854, -10.91162601494193218 ) ) ;
#30804 = CARTESIAN_POINT ( 'NONE',  ( 33.58253175000000823, 22.27500000273117209, 10.91162601494192685 ) ) ;
#30805 = CARTESIAN_POINT ( 'NONE',  ( 33.58253175000000823, 74.02500000273120406, 10.91162601494192685 ) ) ;
#30806 = CARTESIAN_POINT ( 'NONE',  ( -32.50000000000000000, 26.50000000546237544, 0.000000000000000000 ) ) ;
#30807 = CARTESIAN_POINT ( 'NONE',  ( -32.50000000000000000, 61.89999999999999147, -10.55989012756945478 ) ) ;
#30808 = VECTOR ( 'NONE', #21381, 1000.000000000000000 ) ;
#30809 = CARTESIAN_POINT ( 'NONE',  ( 14.47279130897151944, 14.92499999726881477, -19.92008829642072598 ) ) ;
#30810 = CARTESIAN_POINT ( 'NONE',  ( -33.58253175000000113, 67.02500000273117564, -10.91162601494193041 ) ) ;
#30811 =( BOUNDED_CURVE ( )  B_SPLINE_CURVE ( 2, ( #9707, #25152, #1628, #4047, #22753, #7129, #14521, #24980, #12106, #1464, #32528, #20014, #17609 ),
 .UNSPECIFIED., .F., .T. ) 
 B_SPLINE_CURVE_WITH_KNOTS ( ( 3, 2, 2, 2, 2, 2, 3 ),
 ( 0.8910256410256410797, 0.8923076923076923572, 0.8948717948717949122, 0.8974358974358974672, 0.9000000000000000222, 0.9025641025641025772, 0.9038461538461538547 ),
 .UNSPECIFIED. ) 
 CURVE ( )  GEOMETRIC_REPRESENTATION_ITEM ( )  RATIONAL_B_SPLINE_CURVE ( ( 0.9755282581475768211, 0.9755282581475778203, 1.000000000000000000, 0.9510565162951535312, 1.000000000000000000, 0.9510565162951535312, 1.000000000000000000, 0.9510565162951535312, 1.000000000000000000, 0.9510565162951535312, 1.000000000000000000, 0.9755282581475768211, 0.9755282581475768211 ) ) 
 REPRESENTATION_ITEM ( '' )  );
#30812 = CARTESIAN_POINT ( 'NONE',  ( 18.94512977948576093, 3.324999997268818230, -13.76444248337722875 ) ) ;
#30813 = CARTESIAN_POINT ( 'NONE',  ( -27.95245687107223986, 44.50743083240935505, 0.04044903255043252877 ) ) ;
#30814 = CARTESIAN_POINT ( 'NONE',  ( -27.16883889988623935, 77.57500000273120122, 19.73931689729374739 ) ) ;
#30815 =( BOUNDED_CURVE ( )  B_SPLINE_CURVE ( 2, ( #9128, #27665, #25438, #14628, #24915, #30394, #9289, #22019, #19610, #24748, #22689, #1224, #19773 ),
 .UNSPECIFIED., .F., .T. ) 
 B_SPLINE_CURVE_WITH_KNOTS ( ( 3, 2, 2, 2, 2, 2, 3 ),
 ( 0.6730769230769231282, 0.6743589743589744057, 0.6769230769230769607, 0.6794871794871795156, 0.6820512820512820706, 0.6846153846153846256, 0.6858974358974359031 ),
 .UNSPECIFIED. ) 
 CURVE ( )  GEOMETRIC_REPRESENTATION_ITEM ( )  RATIONAL_B_SPLINE_CURVE ( ( 0.9755282581475768211, 0.9755282581475778203, 1.000000000000000000, 0.9510565162951535312, 1.000000000000000000, 0.9510565162951535312, 1.000000000000000000, 0.9510565162951535312, 1.000000000000000000, 0.9510565162951535312, 1.000000000000000000, 0.9755282581475768211, 0.9755282581475768211 ) ) 
 REPRESENTATION_ITEM ( '' )  );
#30816 = CARTESIAN_POINT ( 'NONE',  ( 27.16883889988624290, 3.925000002731188431, 19.73931689729373673 ) ) ;
#30817 = CARTESIAN_POINT ( 'NONE',  ( 1.507698388325705758E-15, 13.62499999726882827, -24.62258325217400312 ) ) ;
#30818 = CARTESIAN_POINT ( 'NONE',  ( -26.07999730980490583, 59.83854166666666430, -6.988114217767815717 ) ) ;
#30819 = ORIENTED_EDGE ( 'NONE', *, *, #33551, .F. ) ;
#30820 = CARTESIAN_POINT ( 'NONE',  ( -10.37757302488624411, 52.72500000273121401, -31.93888565452638417 ) ) ;
#30821 = ORIENTED_EDGE ( 'NONE', *, *, #16507, .T. ) ;
#30822 = CARTESIAN_POINT ( 'NONE',  ( 28.01184896238290278, 30.33333333333332860, -7.505752307973347470 ) ) ;
#30823 = CARTESIAN_POINT ( 'NONE',  ( 0.04044903254992426173, 34.49256916759064495, -30.02300923189239867 ) ) ;
#30824 = CARTESIAN_POINT ( 'NONE',  ( 19.82091636218621389, 10.20000000000001528, -14.40073868116559197 ) ) ;
#30825 = CARTESIAN_POINT ( 'NONE',  ( -20.08610463437157989, 8.200000005462374730, -27.64615127144129758 ) ) ;
#30826 = CARTESIAN_POINT ( 'NONE',  ( -7.570916362186215665, 9.149999994537639125, 23.30088464923126423 ) ) ;
#30827 = CARTESIAN_POINT ( 'NONE',  ( 18.94512977948575738, 6.924999997268810326, 13.76444248337723408 ) ) ;
#30828 = CARTESIAN_POINT ( 'NONE',  ( 23.41746825000000243, 10.72499999726880127, -7.608796670333727974 ) ) ;
#30829 = CARTESIAN_POINT ( 'NONE',  ( 27.16883889988624290, 16.17500000273119909, 19.73931689729373673 ) ) ;
#30830 = CARTESIAN_POINT ( 'NONE',  ( 20.08610463437157279, 27.80000000546238326, -27.64615127144129758 ) ) ;
#30831 = EDGE_CURVE ( 'NONE', #8605, #21926, #23218, .T. ) ;
#30832 = CIRCLE ( 'NONE', #676, 24.49999999999999645 ) ;
#30833 = CARTESIAN_POINT ( 'NONE',  ( -10.04305231718579172, 65.59999999999999432, -30.90933677959248982 ) ) ;
#30834 = CARTESIAN_POINT ( 'NONE',  ( 24.50000000000000000, 11.64999999453762314, 7.960532557706212486 ) ) ;
#30835 = CARTESIAN_POINT ( 'NONE',  ( -13.22843218963023837, 74.00000000000005684, 6.523198192541685536 ) ) ;
#30836 = CARTESIAN_POINT ( 'NONE',  ( -20.53372385742071771, 60.70350666759063785, 20.47846945139902530 ) ) ;
#30837 = CARTESIAN_POINT ( 'NONE',  ( -10.37757302488623701, 31.77500000273120051, 31.93888565452638417 ) ) ;
#30838 = CARTESIAN_POINT ( 'NONE',  ( -11.25946833292375793, 81.17500000273119554, -8.180482586598733619 ) ) ;
#30839 = CARTESIAN_POINT ( 'NONE',  ( 7.505752307973351023, 38.06770833333332860, 28.01184896238290278 ) ) ;
#30840 = DIRECTION ( 'NONE',  ( 1.000000000000000000, 0.000000000000000000, 0.000000000000000000 ) ) ;
#30841 = EDGE_CURVE ( 'NONE', #7039, #7405, #4037, .T. ) ;
#30842 = CARTESIAN_POINT ( 'NONE',  ( -4.523095164977116484E-15, 14.62499999726882649, 24.62258325217400312 ) ) ;
#30843 = CARTESIAN_POINT ( 'NONE',  ( -32.50000000000000000, 6.000000000000005329, 0.000000000000000000 ) ) ;
#30844 = CARTESIAN_POINT ( 'NONE',  ( -7.570916362186210335, 16.60000000000000497, -23.30088464923126779 ) ) ;
#30845 = CARTESIAN_POINT ( 'NONE',  ( 19.11951029504797006, 50.09336833240935505, 19.06425588902558133 ) ) ;
#30846 = CARTESIAN_POINT ( 'NONE',  ( 20.75514604977249178, 51.82500000273120122, 28.56700777964553950 ) ) ;
#30847 = CARTESIAN_POINT ( 'NONE',  ( 27.16883889988623935, 62.57500000273117990, -19.73931689729374384 ) ) ;
#30848 = CARTESIAN_POINT ( 'NONE',  ( -20.75514604977248823, 41.07500000273119412, -28.56700777964554305 ) ) ;
#30849 = CARTESIAN_POINT ( 'NONE',  ( -14.47279130897151767, 15.32499999726880269, -19.92008829642072598 ) ) ;
#30850 = DIRECTION ( 'NONE',  ( -0.000000000000000000, 1.000000000000000000, -0.000000000000000000 ) ) ;
#30851 = CARTESIAN_POINT ( 'NONE',  ( -20.75514604977248112, 1.425000002731191984, 28.56700777964554661 ) ) ;
#30852 = CARTESIAN_POINT ( 'NONE',  ( 23.23218422517957293, 16.99999999999997868, 3.037944173731645936 ) ) ;
#30853 = CARTESIAN_POINT ( 'NONE',  ( -26.29305231718579350, 79.79999999999999716, -19.10302069950537884 ) ) ;
#30854 = CARTESIAN_POINT ( 'NONE',  ( 10.37757302488624767, 23.72500000273118559, 31.93888565452638417 ) ) ;
#30855 = DIRECTION ( 'NONE',  ( 0.000000000000000000, 0.000000000000000000, -1.000000000000000000 ) ) ;
#30856 = CARTESIAN_POINT ( 'NONE',  ( 0.000000000000000000, -20.99999999999998934, 0.000000000000000000 ) ) ;
#30857 = CARTESIAN_POINT ( 'NONE',  ( -30.02300923189239867, 68.56993083240934084, 0.04044903255044988294 ) ) ;
#30858 = CARTESIAN_POINT ( 'NONE',  ( -32.50000000000000000, 44.60000000546237686, 10.55989012756946366 ) ) ;
#30859 = CARTESIAN_POINT ( 'NONE',  ( -5.147494310547423346, 60.94874572391552192, 32.50000000000000000 ) ) ;
#30860 = CARTESIAN_POINT ( 'NONE',  ( -33.58253175000000113, 27.12500000273118772, 0.000000000000000000 ) ) ;
#30861 = CARTESIAN_POINT ( 'NONE',  ( 27.95245687107222921, 33.91406249999997158, -2.463307335887066074E-13 ) ) ;
#30862 = VECTOR ( 'NONE', #4712, 1000.000000000000000 ) ;
#30863 = ORIENTED_EDGE ( 'NONE', *, *, #10848, .T. ) ;
#30864 = CARTESIAN_POINT ( 'NONE',  ( -27.16883889988624290, 66.92500000273119554, -19.73931689729374028 ) ) ;
#30865 = CARTESIAN_POINT ( 'NONE',  ( 7.505752307972854531, 40.07291666666666430, -28.01184896238303423 ) ) ;
#30866 = CARTESIAN_POINT ( 'NONE',  ( 2.694222958124179176E-15, -45.00000000000001421, 0.000000000000000000 ) ) ;
#30867 = ORIENTED_EDGE ( 'NONE', *, *, #223, .T. ) ;
#30868 = CARTESIAN_POINT ( 'NONE',  ( -7.543491769121417612, 56.97954833425730925, 28.00173670424549499 ) ) ;
#30869 = CARTESIAN_POINT ( 'NONE',  ( 7.025853678916403666, 62.13579833425730925, -26.06988505166735237 ) ) ;
#30870 = CARTESIAN_POINT ( 'NONE',  ( 6.486482029760649416E-15, 13.62500000273118417, 35.31076352940723240 ) ) ;
#30871 = CARTESIAN_POINT ( 'NONE',  ( 14.97647472619900455, 14.71576416574268720, -26.02091320914876960 ) ) ;
#30872 = CARTESIAN_POINT ( 'NONE',  ( 3.306546357697853733E-15, 11.99999999999999645, -27.00000000000000000 ) ) ;
#30873 = CARTESIAN_POINT ( 'NONE',  ( -33.58253175000000113, 33.37500000273119127, 0.000000000000000000 ) ) ;
#30874 = CARTESIAN_POINT ( 'NONE',  ( -10.04305231718578462, 40.90000000546237402, 30.90933677959249337 ) ) ;
#30875 = CARTESIAN_POINT ( 'NONE',  ( -9.270509831248425314, 75.69999999999998863, -12.75976212528059861 ) ) ;
#30876 = CARTESIAN_POINT ( 'NONE',  ( 20.75514604977248467, 24.42500000273119554, -28.56700777964554305 ) ) ;
#30877 = CARTESIAN_POINT ( 'NONE',  ( -32.50000000000000000, 23.90000000000000213, -10.55989012756945300 ) ) ;
#30878 = CARTESIAN_POINT ( 'NONE',  ( -33.58253175000000113, 49.27500000273118985, -10.91162601494193218 ) ) ;
#30879 =( LENGTH_UNIT ( ) NAMED_UNIT ( * ) SI_UNIT ( .MILLI., .METRE. ) );
#30880 = CARTESIAN_POINT ( 'NONE',  ( 10.04305231718578817, 31.39999999999999858, -30.90933677959249337 ) ) ;
#30881 = EDGE_CURVE ( 'NONE', #22505, #52, #30202, .T. ) ;
#30882 = CARTESIAN_POINT ( 'NONE',  ( -20.08610463437156923, 30.30000000000000426, 27.64615127144130113 ) ) ;
#30883 = CARTESIAN_POINT ( 'NONE',  ( 15.14183272437242245, 0.2999999999999904965, -20.84094480462497856 ) ) ;
#30884 = CARTESIAN_POINT ( 'NONE',  ( -2.162160676586881955E-15, 68.62500000273119838, -35.31076352940723240 ) ) ;
#30885 = CARTESIAN_POINT ( 'NONE',  ( -32.63512777199724724, -24.47487373415291501, 0.000000000000000000 ) ) ;
#30886 = CARTESIAN_POINT ( 'NONE',  ( 0.000000000000000000, 0.000000000000000000, -30.50000000000000000 ) ) ;
#30887 = CARTESIAN_POINT ( 'NONE',  ( 27.16883889988624290, 58.17500000273118133, 19.73931689729373673 ) ) ;
#30888 = CARTESIAN_POINT ( 'NONE',  ( 12.13525491562420910, 79.45000000546237118, -8.816778784387098611 ) ) ;
#30889 = AXIS2_PLACEMENT_3D ( 'NONE', #9883, #8321, #11080 ) ;
#30890 = CARTESIAN_POINT ( 'NONE',  ( -10.04305231718578462, 40.90000000546237402, 30.90933677959249337 ) ) ;
#30891 = CARTESIAN_POINT ( 'NONE',  ( 33.58253175000000113, 20.22500000273117848, -10.91162601494193751 ) ) ;
#30892 = CARTESIAN_POINT ( 'NONE',  ( 19.82091636218621034, 9.549999994537621717, 14.40073868116559730 ) ) ;
#30893 = CARTESIAN_POINT ( 'NONE',  ( 26.09010956794232428, 24.89621500092397710, -6.950374756619718042 ) ) ;
#30894 = CARTESIAN_POINT ( 'NONE',  ( -1.778240108872766143E-15, 47.49999999999999289, -32.49999999999999289 ) ) ;
#30895 = CARTESIAN_POINT ( 'NONE',  ( 27.16883889988624290, 43.92500000273118133, 19.73931689729373673 ) ) ;
#30896 = DIRECTION ( 'NONE',  ( 0.000000000000000000, 1.000000000000000000, 0.000000000000000000 ) ) ;
#30897 = CARTESIAN_POINT ( 'NONE',  ( -33.58253175000000113, 55.37500000273119838, 0.000000000000000000 ) ) ;
#30898 = CARTESIAN_POINT ( 'NONE',  ( -28.00173670424549499, 47.52642333425731636, -7.543491769121417612 ) ) ;
#30899 = EDGE_CURVE ( 'NONE', #21772, #11003, #18305, .T. ) ;
#30900 = DIRECTION ( 'NONE',  ( 0.000000000000000000, 1.000000000000000000, 0.000000000000000000 ) ) ;
#30901 = CARTESIAN_POINT ( 'NONE',  ( 25.98046417659831775, 35.62722249907602645, -15.04653450569338879 ) ) ;
#30902 = CARTESIAN_POINT ( 'NONE',  ( -32.50000000000000000, 60.60000000546239107, 10.55989012756946366 ) ) ;
#30903 = CARTESIAN_POINT ( 'NONE',  ( -8.601468415847515203, 75.17500000273118133, 11.83890561707634959 ) ) ;
#30904 = CARTESIAN_POINT ( 'NONE',  ( 5.147494310547426899, 57.94874572391552903, -32.50000000000000000 ) ) ;
#30905 = CARTESIAN_POINT ( 'NONE',  ( -19.06425588902558133, 68.14024333240935505, 19.11951029504797006 ) ) ;
#30906 = CARTESIAN_POINT ( 'NONE',  ( -14.47279130897152122, 2.424999997268802332, 19.92008829642072243 ) ) ;
#30907 = CARTESIAN_POINT ( 'NONE',  ( -32.50000000000000000, 76.40000000546235981, -10.55989012756945478 ) ) ;
#30908 = CARTESIAN_POINT ( 'NONE',  ( 15.00000000000000000, 79.10000000000000853, -4.873795443493596835 ) ) ;
#30909 = CARTESIAN_POINT ( 'NONE',  ( -10.37757302488623701, 33.77500000273118985, 31.93888565452638417 ) ) ;
#30910 = CARTESIAN_POINT ( 'NONE',  ( -7.236395654485757944, 7.724999997268805707, -22.27133577429736988 ) ) ;
#30911 = ORIENTED_EDGE ( 'NONE', *, *, #3287, .F. ) ;
#30912 = CARTESIAN_POINT ( 'NONE',  ( 6.486482029760649416E-15, 75.87500000273119838, 35.31076352940723240 ) ) ;
#30913 = CARTESIAN_POINT ( 'NONE',  ( 32.50000000000000000, 21.50000000546238610, -3.980102097228898626E-15 ) ) ;
#30914 = CARTESIAN_POINT ( 'NONE',  ( 20.50609665440969565, 43.79687500000000000, -20.50609665441004736 ) ) ;
#30915 = CARTESIAN_POINT ( 'NONE',  ( 27.16883889988624290, 60.17500000273118133, 19.73931689729373673 ) ) ;
#30916 = CARTESIAN_POINT ( 'NONE',  ( -10.04305231718578462, 60.90000000546235981, 30.90933677959249337 ) ) ;
#30917 = ORIENTED_EDGE ( 'NONE', *, *, #15759, .F. ) ;
#30918 =( BOUNDED_CURVE ( )  B_SPLINE_CURVE ( 2, ( #17445, #25153, #27906, #1805, #6959, #27394, #14695, #30290, #16937, #33030, #22755, #17270, #4560 ),
 .UNSPECIFIED., .F., .T. ) 
 B_SPLINE_CURVE_WITH_KNOTS ( ( 3, 2, 2, 2, 2, 2, 3 ),
 ( 0.006410256410256410901, 0.007692307692307692735, 0.01025641025641025640, 0.01282051282051282007, 0.01538461538461538547, 0.01794871794871794740, 0.01923076923076923184 ),
 .UNSPECIFIED. ) 
 CURVE ( )  GEOMETRIC_REPRESENTATION_ITEM ( )  RATIONAL_B_SPLINE_CURVE ( ( 0.9755282581475768211, 0.9755282581475768211, 1.000000000000000000, 0.9510565162951535312, 1.000000000000000000, 0.9510565162951535312, 1.000000000000000000, 0.9510565162951535312, 1.000000000000000000, 0.9510565162951535312, 1.000000000000000000, 0.9755282581475767101, 0.9755282581475768211 ) ) 
 REPRESENTATION_ITEM ( '' )  );
#30919 = CYLINDRICAL_SURFACE ( 'NONE', #25924, 32.50000000000000000 ) ;
#30920 = CARTESIAN_POINT ( 'NONE',  ( 27.16883889988624290, 41.92500000273119554, 19.73931689729373673 ) ) ;
#30921 = CARTESIAN_POINT ( 'NONE',  ( 23.41746824999999887, 16.62499999726882294, 0.000000000000000000 ) ) ;
#30922 = CARTESIAN_POINT ( 'NONE',  ( 33.58253175000000113, 66.37500000273119838, -4.112674001490185761E-15 ) ) ;
#30923 = CARTESIAN_POINT ( 'NONE',  ( 10.04305231718578817, 3.900000005462367358, -30.90933677959249337 ) ) ;
#30924 = CARTESIAN_POINT ( 'NONE',  ( -10.37757302488624411, 58.72500000273119269, -31.93888565452638417 ) ) ;
#30925 = DIRECTION ( 'NONE',  ( -0.000000000000000000, -1.000000000000000000, -0.000000000000000000 ) ) ;
#30926 = CARTESIAN_POINT ( 'NONE',  ( 32.50000000000000000, 47.10000000000000142, -10.55989012756945833 ) ) ;
#30927 = CARTESIAN_POINT ( 'NONE',  ( 15.14183272437242422, 2.299999999999985612, -20.84094480462497856 ) ) ;
#30928 = CARTESIAN_POINT ( 'NONE',  ( 6.486482029760649416E-15, 19.87500000273119483, 35.31076352940723240 ) ) ;
#30929 = CARTESIAN_POINT ( 'NONE',  ( 24.50000000000000000, 0.09999999999999682754, -7.960532557706203605 ) ) ;
#30930 = CARTESIAN_POINT ( 'NONE',  ( 19.06425588902558133, 28.60899333240935150, -19.11951029504797006 ) ) ;
#30931 = CARTESIAN_POINT ( 'NONE',  ( -13.91746824999999887, 79.37500000273118417, 0.000000000000000000 ) ) ;
#30932 = CARTESIAN_POINT ( 'NONE',  ( -10.37757302488623701, 77.77500000273118985, 31.93888565452638417 ) ) ;
#30933 = CARTESIAN_POINT ( 'NONE',  ( 32.50000000000000000, 53.50000000546237544, -3.980102097228898626E-15 ) ) ;
#30934 = CARTESIAN_POINT ( 'NONE',  ( -2.162160676586881955E-15, 72.87500000273115575, -35.31076352940723240 ) ) ;
#30935 = ORIENTED_EDGE ( 'NONE', *, *, #11534, .F. ) ;
#30936 = CARTESIAN_POINT ( 'NONE',  ( -14.47279130897152122, 12.42499999726880766, 19.92008829642072243 ) ) ;
#30937 = CARTESIAN_POINT ( 'NONE',  ( -23.41746825000000243, 1.724999997268824581, 7.608796670333725309 ) ) ;
#30938 = CARTESIAN_POINT ( 'NONE',  ( -19.09188309203660694, 48.95312500000000000, 19.09188309203694800 ) ) ;
#30939 = CARTESIAN_POINT ( 'NONE',  ( 20.75514604977249178, 57.82500000273118701, 28.56700777964553950 ) ) ;
#30940 = CARTESIAN_POINT ( 'NONE',  ( 27.16883889988623935, 20.57500000273120122, -19.73931689729374384 ) ) ;
#30941 = CARTESIAN_POINT ( 'NONE',  ( -20.75514604977248112, 11.67500000273118843, 28.56700777964554661 ) ) ;
#30942 = CARTESIAN_POINT ( 'NONE',  ( 2.584737979205442066E-13, 31.33593749999999289, 27.95245687107223276 ) ) ;
#30943 = CARTESIAN_POINT ( 'NONE',  ( -0.04044903254990864921, 22.46131916759064850, 30.02300923189239867 ) ) ;
#30944 = CARTESIAN_POINT ( 'NONE',  ( 7.505752307972854531, 60.69791666666667140, -28.01184896238303423 ) ) ;
#30945 = CARTESIAN_POINT ( 'NONE',  ( 33.58253175000000823, 2.025000002731187632, 10.91162601494192863 ) ) ;
#30946 = CARTESIAN_POINT ( 'NONE',  ( -4.300734207923755825, 71.77500000273117564, 13.23629886949340673 ) ) ;
#30947 = CARTESIAN_POINT ( 'NONE',  ( -2.092463501923844636E-15, 41.49999999999999289, -34.17252228774368916 ) ) ;
#30948 = CARTESIAN_POINT ( 'NONE',  ( 27.16883889988623935, 48.32500000273117990, -19.73931689729374384 ) ) ;
#30949 = CARTESIAN_POINT ( 'NONE',  ( -18.94512977948576093, 11.82499999726882578, 13.76444248337722698 ) ) ;
#30950 = CARTESIAN_POINT ( 'NONE',  ( 15.00000000000000000, 79.10000000000000853, -4.873795443493596835 ) ) ;
#30951 = VERTEX_POINT ( 'NONE', #9584 ) ;
#30952 = CARTESIAN_POINT ( 'NONE',  ( 20.75514604977248467, 56.67500000273119554, -28.56700777964554305 ) ) ;
#30953 = CARTESIAN_POINT ( 'NONE',  ( 0.000000000000000000, 74.00000000000001421, 0.000000000000000000 ) ) ;
#30954 = CARTESIAN_POINT ( 'NONE',  ( 26.06988505166735592, 45.80767333425730925, 7.025853678916393896 ) ) ;
#30955 = CARTESIAN_POINT ( 'NONE',  ( 33.58253175000000113, 74.37500000273116996, -4.112674001490185761E-15 ) ) ;
#30956 = ORIENTED_EDGE ( 'NONE', *, *, #28553, .F. ) ;
#30957 = CARTESIAN_POINT ( 'NONE',  ( 10.37757302488624767, 23.72500000273118559, 31.93888565452638417 ) ) ;
#30958 = CARTESIAN_POINT ( 'NONE',  ( 28.01184896238290278, 16.58333333333333215, -7.505752307973347470 ) ) ;
#30959 =( BOUNDED_CURVE ( )  B_SPLINE_CURVE ( 2, ( #32567, #1502, #28112, #30671, #16972, #30499, #19547, #1670, #17144, #19877, #29995, #22447, #9577 ),
 .UNSPECIFIED., .F., .T. ) 
 B_SPLINE_CURVE_WITH_KNOTS ( ( 3, 2, 2, 2, 2, 2, 3 ),
 ( 0.1346153846153846090, 0.1358974358974358865, 0.1384615384615384692, 0.1410256410256410242, 0.1435897435897435792, 0.1461538461538461620, 0.1474358974358974395 ),
 .UNSPECIFIED. ) 
 CURVE ( )  GEOMETRIC_REPRESENTATION_ITEM ( )  RATIONAL_B_SPLINE_CURVE ( ( 0.9755282581475768211, 0.9755282581475768211, 1.000000000000000000, 0.9510565162951535312, 1.000000000000000000, 0.9510565162951535312, 1.000000000000000000, 0.9510565162951535312, 1.000000000000000000, 0.9510565162951535312, 1.000000000000000000, 0.9755282581475768211, 0.9755282581475768211 ) ) 
 REPRESENTATION_ITEM ( '' )  );
#30960 = ORIENTED_EDGE ( 'NONE', *, *, #30966, .T. ) ;
#30961 = CARTESIAN_POINT ( 'NONE',  ( -5.147494310547213736, 14.05125428700922541, -32.50000000000007105 ) ) ;
#30962 = CARTESIAN_POINT ( 'NONE',  ( 20.75514604977249178, 59.82500000273117280, 28.56700777964553950 ) ) ;
#30963 = CARTESIAN_POINT ( 'NONE',  ( -28.01184896238290278, 38.92708333333333570, 7.505752307973363457 ) ) ;
#30964 = CARTESIAN_POINT ( 'NONE',  ( -19.82091636218621389, 11.19999999999998863, 14.40073868116558842 ) ) ;
#30965 = CARTESIAN_POINT ( 'NONE',  ( -18.94512977948575738, 3.924999997268807661, -13.76444248337723231 ) ) ;
#30966 = EDGE_CURVE ( 'NONE', #7405, #7039, #20500, .T. ) ;
#30967 = CARTESIAN_POINT ( 'NONE',  ( -10.37757302488623701, 11.52500000273118452, 31.93888565452638417 ) ) ;
#30968 = CARTESIAN_POINT ( 'NONE',  ( -20.53372385742107653, 55.24961833240936926, -20.47846945139867003 ) ) ;
#30969 = CARTESIAN_POINT ( 'NONE',  ( 5.147494310547426899, 37.44874571845314648, -32.50000000000000000 ) ) ;
#30970 = CARTESIAN_POINT ( 'NONE',  ( 15.01150461594643382, 65.42447916666665719, 26.00068869287340334 ) ) ;
#30971 = CARTESIAN_POINT ( 'NONE',  ( 10.04305231718578817, 19.90000000546238113, -30.90933677959249337 ) ) ;
#30972 = CARTESIAN_POINT ( 'NONE',  ( 32.50000000000000000, 17.10000000000001208, -10.55989012756945833 ) ) ;
#30973 = CARTESIAN_POINT ( 'NONE',  ( 15.14183272437241889, 11.44999999453763095, 20.84094480462498211 ) ) ;
#30974 = CARTESIAN_POINT ( 'NONE',  ( 13.91746825000000065, 79.77500000273118985, 4.522059556121114987 ) ) ;
#30975 = CARTESIAN_POINT ( 'NONE',  ( -24.20753774853756823, 25.60677083333332149, -13.97622843553588723 ) ) ;
#30976 = CARTESIAN_POINT ( 'NONE',  ( -10.37757302488624411, 32.72500000273117848, -31.93888565452638417 ) ) ;
#30977 = CONICAL_SURFACE ( 'NONE', #29332, 30.00000000000000711, 0.7665918932241471140 ) ;
#30978 = CARTESIAN_POINT ( 'NONE',  ( -33.58253175000000113, 77.02500000273118985, -10.91162601494193218 ) ) ;
#30979 = CARTESIAN_POINT ( 'NONE',  ( -33.58253175000000113, 41.37500000273118417, 0.000000000000000000 ) ) ;
#30980 = CARTESIAN_POINT ( 'NONE',  ( -20.75514604977248823, 21.07500000273118346, -28.56700777964554305 ) ) ;
#30981 = CARTESIAN_POINT ( 'NONE',  ( -15.00000000000000000, 80.10000000000000853, 4.873795443493597723 ) ) ;
#30982 = CARTESIAN_POINT ( 'NONE',  ( 10.37757302488624767, 75.72500000273119269, 31.93888565452638417 ) ) ;
#30983 = VECTOR ( 'NONE', #13247, 1000.000000000000000 ) ;
#30984 = CARTESIAN_POINT ( 'NONE',  ( 7.570916362186213000, 8.399999999999991473, -23.30088464923126423 ) ) ;
#30985 = CARTESIAN_POINT ( 'NONE',  ( 20.08610463437158344, 62.69999999999999574, 27.64615127144129403 ) ) ;
#30986 = CARTESIAN_POINT ( 'NONE',  ( -18.94512977948576093, 15.82499999726880091, 13.76444248337722698 ) ) ;
#30987 = CARTESIAN_POINT ( 'NONE',  ( -20.75514604977248823, 62.82500000273119412, -28.56700777964554305 ) ) ;
#30988 = CARTESIAN_POINT ( 'NONE',  ( 18.94512977948576093, 11.32499999726882578, -13.76444248337722875 ) ) ;
#30989 = CARTESIAN_POINT ( 'NONE',  ( -27.16883889988624290, 75.17500000273118133, -19.73931689729374028 ) ) ;
#30990 = CARTESIAN_POINT ( 'NONE',  ( 6.486482029760648627E-15, 5.625000002731175286, 35.31076352940722529 ) ) ;
#30991 = AXIS2_PLACEMENT_3D ( 'NONE', #25404, #28149, #1882 ) ;
#30992 = CARTESIAN_POINT ( 'NONE',  ( -18.94512977948575738, 1.424999997268805441, -13.76444248337723231 ) ) ;
#30993 = CARTESIAN_POINT ( 'NONE',  ( -19.06425588902591173, 16.87538166759064140, -19.11951029504763611 ) ) ;
#30994 = AXIS2_PLACEMENT_3D ( 'NONE', #13655, #24120, #13819 ) ;
#30995 = ORIENTED_EDGE ( 'NONE', *, *, #18697, .F. ) ;
#30996 = CARTESIAN_POINT ( 'NONE',  ( -10.37757302488623701, 45.52500000273117564, 31.93888565452638417 ) ) ;
#30997 = ORIENTED_EDGE ( 'NONE', *, *, #22429, .F. ) ;
#30998 = CARTESIAN_POINT ( 'NONE',  ( -15.01150461594595775, 31.62239583333332860, 26.00068869287368756 ) ) ;
#30999 = CARTESIAN_POINT ( 'NONE',  ( -32.50000000000000000, 80.00000000000001421, 0.000000000000000000 ) ) ;
#31000 = CARTESIAN_POINT ( 'NONE',  ( -32.50000000000000000, 2.500000005462382546, 0.000000000000000000 ) ) ;
#31001 = CARTESIAN_POINT ( 'NONE',  ( -32.50000000000000000, 72.60000000546236265, 10.55989012756946366 ) ) ;
#31002 = CARTESIAN_POINT ( 'NONE',  ( -18.94512977948575738, 1.924999997268805885, -13.76444248337723231 ) ) ;
#31003 = CARTESIAN_POINT ( 'NONE',  ( 18.94512977948576093, 12.82499999726882578, -13.76444248337722875 ) ) ;
#31004 = CARTESIAN_POINT ( 'NONE',  ( 10.37757302488624056, 12.77500000273118452, -31.93888565452638417 ) ) ;
#31005 = CARTESIAN_POINT ( 'NONE',  ( 10.04305231718579705, 15.10000000546238219, 30.90933677959248982 ) ) ;
#31006 = CARTESIAN_POINT ( 'NONE',  ( 26.29305231718579350, 62.79999999999999716, 19.10302069950537529 ) ) ;
#31007 = CARTESIAN_POINT ( 'NONE',  ( 15.14183272437242422, 12.04999999453763948, -20.84094480462497856 ) ) ;
#31008 = FACE_OUTER_BOUND ( 'NONE', #25085, .T. ) ;
#31009 = CARTESIAN_POINT ( 'NONE',  ( -25.98046417659859486, 64.85715250092397355, -15.04653450569291628 ) ) ;
#31010 = CARTESIAN_POINT ( 'NONE',  ( 33.58253175000000823, 30.27500000273118630, 10.91162601494192863 ) ) ;
#31011 = CARTESIAN_POINT ( 'NONE',  ( -20.08610463437157989, 32.20000000546238539, -27.64615127144129758 ) ) ;
#31012 = CARTESIAN_POINT ( 'NONE',  ( 20.50609665441005092, 37.78124999999999289, 20.50609665440969209 ) ) ;
#31013 = CARTESIAN_POINT ( 'NONE',  ( -7.236395654485763274, 16.52499999726880731, 22.27133577429736633 ) ) ;
#31014 = CARTESIAN_POINT ( 'NONE',  ( -2.092463501923844636E-15, 7.499999999999995559, -34.17252228774368916 ) ) ;
#31015 = CARTESIAN_POINT ( 'NONE',  ( -9.270509831248419985, 74.30000000000001137, 12.75976212528060039 ) ) ;
#31016 = CARTESIAN_POINT ( 'NONE',  ( 7.025853678916867295, 57.25482666574269075, 26.06988505166722803 ) ) ;
#31017 = CARTESIAN_POINT ( 'NONE',  ( -20.75514604977248112, 51.42500000273118133, 28.56700777964554661 ) ) ;
#31018 = VECTOR ( 'NONE', #25062, 1000.000000000000000 ) ;
#31019 = CARTESIAN_POINT ( 'NONE',  ( -33.58253175000000113, 61.37500000273120548, 0.000000000000000000 ) ) ;
#31020 = CARTESIAN_POINT ( 'NONE',  ( -33.58253175000000113, 41.47500000273117138, 10.91162601494193929 ) ) ;
#31021 =( BOUNDED_CURVE ( )  B_SPLINE_CURVE ( 2, ( #23511, #29478, #27081, #26417, #21780, #5482, #13714, #14047, #487, #5982, #8383, #21283, #11302 ),
 .UNSPECIFIED., .F., .T. ) 
 B_SPLINE_CURVE_WITH_KNOTS ( ( 3, 2, 2, 2, 2, 2, 3 ),
 ( 0.3397435897435897578, 0.3410256410256410353, 0.3435897435897435903, 0.3461538461538461453, 0.3487179487179487003, 0.3512820512820512553, 0.3525641025641025883 ),
 .UNSPECIFIED. ) 
 CURVE ( )  GEOMETRIC_REPRESENTATION_ITEM ( )  RATIONAL_B_SPLINE_CURVE ( ( 0.9755282581475768211, 0.9755282581475768211, 1.000000000000000000, 0.9510565162951535312, 1.000000000000000000, 0.9510565162951535312, 1.000000000000000000, 0.9510565162951535312, 1.000000000000000000, 0.9510565162951535312, 1.000000000000000000, 0.9755282581475762660, 0.9755282581475768211 ) ) 
 REPRESENTATION_ITEM ( '' )  );
#31022 = CARTESIAN_POINT ( 'NONE',  ( 0.000000000000000000, 70.00000000000000000, 26.50000000000000355 ) ) ;
#31023 = CARTESIAN_POINT ( 'NONE',  ( 20.08610463437157279, 15.80000000546237970, -27.64615127144129758 ) ) ;
#31024 = DIRECTION ( 'NONE',  ( 0.000000000000000000, 0.000000000000000000, -1.000000000000000000 ) ) ;
#31025 =( BOUNDED_SURFACE ( )  B_SPLINE_SURFACE ( 1, 2, ( 
 ( #32772, #7037, #9266, #3959, #22486, #14433, #9614, #12188, #30888, #14942, #7209, #33112, #14603, #27981, #25060, #24888, #22831, #9435, #9789, #19920, #12363, #17348, #20096, #33291, #1372, #30714, #1541, #30541, #22327, #12017, #17520, #7384, #1710, #32937, #27811, #11848, #17868, #30368, #17692, #4468, #28152, #19750, #20267, #4295, #30198, #25407, #17182, #22658, #4638, #1885, #14770, #25235, #6699, #15117, #25581, #2061, #12537, #23006, #27640, #33463, #4128, #9963, #20438, #5787, #21082, #18679, #32027, #8690, #8189, #24319, #10775, #13524, #33639, #13853, #5622, #29119, #23987, #3220, #25747, #21581, #26389, #21416, #12706, #2882, #10941, #21751, #26557, #13348, #31696, #4808, #32196, #287, #8524, #31859, #19008, #10604, #24152, #5452, #28320, #29287, #8024 ),
 ( #23821, #18510, #18841, #11112, #21252, #15287, #2229, #792, #16268, #8352, #11275, #29452, #5954, #31531, #16434, #459, #16106, #3053, #23177, #26725, #15933, #13688, #26886, #623, #3383, #28956, #4043, #16596, #22406, #6113, #19505, #29780, #32854, #24639, #24479, #6456, #30285, #16930, #27051, #1113, #9349, #3877, #17097, #9023, #3544, #3713, #14016, #1624, #25148, #6786, #11433, #27555, #953, #12102, #14517, #14183, #21910, #14350, #17264, #22246, #6285, #6618, #24976, #1285, #11598, #29952, #22079, #24807, #32523, #1459, #27388, #11764, #32360, #11937, #8854, #19336, #32690, #19174, #16761, #19832, #27727, #27220, #4215, #22573, #9185, #19669, #14689, #30114, #33024, #29611, #33733, #12967, #15033, #25323, #30457, #9875, #20710, #1798, #20183, #12797, #6954 ) ),
 .UNSPECIFIED., .F., .F., .T. ) 
 B_SPLINE_SURFACE_WITH_KNOTS ( ( 2, 2 ),
 ( 3, 2, 2, 2, 2, 2, 2, 2, 2, 2, 2, 2, 2, 2, 2, 2, 2, 2, 2, 2, 2, 2, 2, 2, 2, 2, 2, 2, 2, 2, 2, 2, 2, 2, 2, 2, 2, 2, 2, 2, 2, 2, 2, 2, 2, 2, 2, 2, 2, 2, 3 ),
 ( 0.000000000000000000, 1.000000000000000000 ),
 ( 0.000000000000000000, 0.02000000000000000042, 0.04000000000000000083, 0.05999999999999999778, 0.08000000000000000167, 0.1000000000000000056, 0.1199999999999999956, 0.1400000000000000133, 0.1600000000000000033, 0.1799999999999999933, 0.2000000000000000111, 0.2200000000000000011, 0.2399999999999999911, 0.2600000000000000089, 0.2800000000000000266, 0.2999999999999999889, 0.3200000000000000067, 0.3400000000000000244, 0.3599999999999999867, 0.3800000000000000044, 0.4000000000000000222, 0.4199999999999999845, 0.4400000000000000022, 0.4600000000000000200, 0.4799999999999999822, 0.5000000000000000000, 0.5200000000000000178, 0.5400000000000000355, 0.5600000000000000533, 0.5799999999999999600, 0.5999999999999999778, 0.6199999999999999956, 0.6400000000000000133, 0.6600000000000000311, 0.6800000000000000488, 0.6999999999999999556, 0.7199999999999999734, 0.7399999999999999911, 0.7600000000000000089, 0.7800000000000000266, 0.8000000000000000444, 0.8199999999999999512, 0.8399999999999999689, 0.8599999999999999867, 0.8800000000000000044, 0.9000000000000000222, 0.9200000000000000400, 0.9399999999999999467, 0.9599999999999999645, 0.9799999999999999822, 1.000000000000000000 ),
 .UNSPECIFIED. ) 
 GEOMETRIC_REPRESENTATION_ITEM ( )  RATIONAL_B_SPLINE_SURFACE ( (
 ( 1.000000000000000000, 0.9510565162951535312, 1.000000000000000000, 0.9510565162951535312, 1.000000000000000000, 0.9510565162951535312, 1.000000000000000000, 0.9510565162951535312, 1.000000000000000000, 0.9510565162951535312, 1.000000000000000000, 0.9510565162951535312, 1.000000000000000000, 0.9510565162951535312, 1.000000000000000000, 0.9510565162951535312, 1.000000000000000000, 0.9510565162951535312, 1.000000000000000000, 0.9510565162951535312, 1.000000000000000000, 0.9510565162951535312, 1.000000000000000000, 0.9510565162951535312, 1.000000000000000000, 0.9510565162951535312, 1.000000000000000000, 0.9510565162951535312, 1.000000000000000000, 0.9510565162951535312, 1.000000000000000000, 0.9510565162951535312, 1.000000000000000000, 0.9510565162951535312, 1.000000000000000000, 0.9510565162951535312, 1.000000000000000000, 0.9510565162951535312, 1.000000000000000000, 0.9510565162951535312, 1.000000000000000000, 0.9510565162951535312, 1.000000000000000000, 0.9510565162951535312, 1.000000000000000000, 0.9510565162951535312, 1.000000000000000000, 0.9510565162951535312, 1.000000000000000000, 0.9510565162951535312, 1.000000000000000000, 0.9510565162951535312, 1.000000000000000000, 0.9510565162951535312, 1.000000000000000000, 0.9510565162951535312, 1.000000000000000000, 0.9510565162951535312, 1.000000000000000000, 0.9510565162951535312, 1.000000000000000000, 0.9510565162951535312, 1.000000000000000000, 0.9510565162951535312, 1.000000000000000000, 0.9510565162951535312, 1.000000000000000000, 0.9510565162951535312, 1.000000000000000000, 0.9510565162951535312, 1.000000000000000000, 0.9510565162951535312, 1.000000000000000000, 0.9510565162951535312, 1.000000000000000000, 0.9510565162951535312, 1.000000000000000000, 0.9510565162951535312, 1.000000000000000000, 0.9510565162951535312, 1.000000000000000000, 0.9510565162951535312, 1.000000000000000000, 0.9510565162951535312, 1.000000000000000000, 0.9510565162951535312, 1.000000000000000000, 0.9510565162951535312, 1.000000000000000000, 0.9510565162951535312, 1.000000000000000000, 0.9510565162951535312, 1.000000000000000000, 0.9510565162951535312, 1.000000000000000000, 0.9510565162951535312, 1.000000000000000000, 0.9510565162951535312, 1.000000000000000000, 0.9510565162951535312, 1.000000000000000000),
 ( 1.000000000000000000, 0.9510565162951535312, 1.000000000000000000, 0.9510565162951535312, 1.000000000000000000, 0.9510565162951535312, 1.000000000000000000, 0.9510565162951535312, 1.000000000000000000, 0.9510565162951535312, 1.000000000000000000, 0.9510565162951535312, 1.000000000000000000, 0.9510565162951535312, 1.000000000000000000, 0.9510565162951535312, 1.000000000000000000, 0.9510565162951535312, 1.000000000000000000, 0.9510565162951535312, 1.000000000000000000, 0.9510565162951535312, 1.000000000000000000, 0.9510565162951535312, 1.000000000000000000, 0.9510565162951535312, 1.000000000000000000, 0.9510565162951535312, 1.000000000000000000, 0.9510565162951535312, 1.000000000000000000, 0.9510565162951535312, 1.000000000000000000, 0.9510565162951535312, 1.000000000000000000, 0.9510565162951535312, 1.000000000000000000, 0.9510565162951535312, 1.000000000000000000, 0.9510565162951535312, 1.000000000000000000, 0.9510565162951535312, 1.000000000000000000, 0.9510565162951535312, 1.000000000000000000, 0.9510565162951535312, 1.000000000000000000, 0.9510565162951535312, 1.000000000000000000, 0.9510565162951535312, 1.000000000000000000, 0.9510565162951535312, 1.000000000000000000, 0.9510565162951535312, 1.000000000000000000, 0.9510565162951535312, 1.000000000000000000, 0.9510565162951535312, 1.000000000000000000, 0.9510565162951535312, 1.000000000000000000, 0.9510565162951535312, 1.000000000000000000, 0.9510565162951535312, 1.000000000000000000, 0.9510565162951535312, 1.000000000000000000, 0.9510565162951535312, 1.000000000000000000, 0.9510565162951535312, 1.000000000000000000, 0.9510565162951535312, 1.000000000000000000, 0.9510565162951535312, 1.000000000000000000, 0.9510565162951535312, 1.000000000000000000, 0.9510565162951535312, 1.000000000000000000, 0.9510565162951535312, 1.000000000000000000, 0.9510565162951535312, 1.000000000000000000, 0.9510565162951535312, 1.000000000000000000, 0.9510565162951535312, 1.000000000000000000, 0.9510565162951535312, 1.000000000000000000, 0.9510565162951535312, 1.000000000000000000, 0.9510565162951535312, 1.000000000000000000, 0.9510565162951535312, 1.000000000000000000, 0.9510565162951535312, 1.000000000000000000, 0.9510565162951535312, 1.000000000000000000, 0.9510565162951535312, 1.000000000000000000) ) ) 
 REPRESENTATION_ITEM ( '' )  SURFACE ( )  );
#31026 = CARTESIAN_POINT ( 'NONE',  ( 26.29305231718579350, 76.80000000000002558, 19.10302069950537529 ) ) ;
#31027 = CARTESIAN_POINT ( 'NONE',  ( -20.75514604977248112, 13.42500000273119198, 28.56700777964554661 ) ) ;
#31028 = CARTESIAN_POINT ( 'NONE',  ( 3.445340210940985210E-14, 5.499999999999997335, 24.50000000000000000 ) ) ;
#31029 = CARTESIAN_POINT ( 'NONE',  ( 0.000000000000000000, 0.000000000000000000, 0.000000000000000000 ) ) ;
#31030 = CARTESIAN_POINT ( 'NONE',  ( -26.29305231718579350, 39.80000000000000426, -19.10302069950537884 ) ) ;
#31031 = CARTESIAN_POINT ( 'NONE',  ( 0.04044903255044120238, 19.58555583240935860, 27.95245687107223276 ) ) ;
#31032 = CARTESIAN_POINT ( 'NONE',  ( 10.04305231718578817, 33.90000000546238113, -30.90933677959249337 ) ) ;
#31033 = EDGE_CURVE ( 'NONE', #17050, #25078, #27951, .T. ) ;
#31034 = CARTESIAN_POINT ( 'NONE',  ( -5.147494310547423346, 66.44874571845315359, 32.50000000000000000 ) ) ;
#31035 = CARTESIAN_POINT ( 'NONE',  ( 27.16883889988623935, 24.32500000273119056, -19.73931689729374384 ) ) ;
#31036 = CARTESIAN_POINT ( 'NONE',  ( -19.09188309203660694, 48.95312500000000000, 19.09188309203694800 ) ) ;
#31037 = ADVANCED_FACE ( 'NONE', ( #4605, #33256 ), #17657, .F. ) ;
#31038 = ORIENTED_EDGE ( 'NONE', *, *, #19026, .F. ) ;
#31039 = CARTESIAN_POINT ( 'NONE',  ( 10.37757302488624056, 68.52500000273118985, -31.93888565452638417 ) ) ;
#31040 = CARTESIAN_POINT ( 'NONE',  ( -15.01150461594595775, 45.37239583333333570, 26.00068869287368756 ) ) ;
#31041 = DIRECTION ( 'NONE',  ( 0.000000000000000000, 1.000000000000000000, 0.000000000000000000 ) ) ;
#31042 = ORIENTED_EDGE ( 'NONE', *, *, #26141, .T. ) ;
#31043 = CARTESIAN_POINT ( 'NONE',  ( 25.98046417659858420, 56.26340250092398065, 15.04653450569292872 ) ) ;
#31044 = CARTESIAN_POINT ( 'NONE',  ( -7.025853678916393008, 63.85454833425732346, 26.06988505166735592 ) ) ;
#31045 = ORIENTED_EDGE ( 'NONE', *, *, #6084, .F. ) ;
#31046 = CARTESIAN_POINT ( 'NONE',  ( -10.37757302488624411, 12.72500000273117671, -31.93888565452638417 ) ) ;
#31047 = CARTESIAN_POINT ( 'NONE',  ( 25.98046417659831775, 15.00222249907602112, -15.04653450569338879 ) ) ;
#31048 = CARTESIAN_POINT ( 'NONE',  ( 0.000000000000000000, 16.99999999999998579, 0.000000000000000000 ) ) ;
#31049 = AXIS2_PLACEMENT_3D ( 'NONE', #12270, #22744, #33547 ) ;
#31050 = CARTESIAN_POINT ( 'NONE',  ( -10.37757302488624411, 34.97500000273118559, -31.93888565452638417 ) ) ;
#31051 = CARTESIAN_POINT ( 'NONE',  ( -32.50000000000000000, 34.50000000546238255, 0.000000000000000000 ) ) ;
#31052 = CARTESIAN_POINT ( 'NONE',  ( -9.270509831248421762, 78.29999999999995453, 12.75976212528060039 ) ) ;
#31053 = CARTESIAN_POINT ( 'NONE',  ( -2.584737979205441561E-13, 63.99218749999997868, -30.02300923189239512 ) ) ;
#31054 = CARTESIAN_POINT ( 'NONE',  ( -33.58253175000000113, 23.02500000273117919, -10.91162601494193218 ) ) ;
#31055 = CARTESIAN_POINT ( 'NONE',  ( 5.147494310547217289, 31.05125428700920764, 32.50000000000007105 ) ) ;
#31056 = CARTESIAN_POINT ( 'NONE',  ( 20.75514604977249178, 48.07500000273120122, 28.56700777964553950 ) ) ;
#31057 = CARTESIAN_POINT ( 'NONE',  ( -26.29305231718578995, 32.19999999999999574, 19.10302069950538595 ) ) ;
#31058 = CARTESIAN_POINT ( 'NONE',  ( -10.04305231718578462, 24.40000000000000568, 30.90933677959249337 ) ) ;
#31059 = CARTESIAN_POINT ( 'NONE',  ( 24.50000000000000355, 1.899999999999998135, 7.960532557706212486 ) ) ;
#31060 = CARTESIAN_POINT ( 'NONE',  ( 20.75514604977248467, 66.42500000273120975, -28.56700777964554305 ) ) ;
#31061 = CARTESIAN_POINT ( 'NONE',  ( 1.836970198721029589E-15, 16.99999999999998579, 15.00000000000000000 ) ) ;
#31062 = CARTESIAN_POINT ( 'NONE',  ( 33.58253175000000113, 62.47500000273118559, -10.91162601494193574 ) ) ;
#31063 = CARTESIAN_POINT ( 'NONE',  ( -27.16883889988624290, 8.925000002731191984, -19.73931689729374028 ) ) ;
#31064 = CARTESIAN_POINT ( 'NONE',  ( -7.570916362186210335, 12.34999999453761887, -23.30088464923126779 ) ) ;
#31065 = CARTESIAN_POINT ( 'NONE',  ( -24.22776226481240514, 29.90923583425730925, 13.94119854578937812 ) ) ;
#31066 = CARTESIAN_POINT ( 'NONE',  ( -7.738208025866914141, 66.99999999999998579, -32.61747650539069099 ) ) ;
#31067 = CARTESIAN_POINT ( 'NONE',  ( -33.58253175000000113, 37.02500000273117564, -10.91162601494193218 ) ) ;
#31068 = CARTESIAN_POINT ( 'NONE',  ( 20.08610463437157279, 57.29999999999999005, -27.64615127144129758 ) ) ;
#31069 = DIRECTION ( 'NONE',  ( 0.000000000000000000, -1.000000000000000000, 0.000000000000000000 ) ) ;
#31070 = CARTESIAN_POINT ( 'NONE',  ( 24.50000000000000000, 6.000000000000005329, 0.000000000000000000 ) ) ;
#31071 = VECTOR ( 'NONE', #12458, 1000.000000000000000 ) ;
#31072 = CARTESIAN_POINT ( 'NONE',  ( -28.02196122052058413, 48.08815999907601935, -7.468012846824272799 ) ) ;
#31073 = CARTESIAN_POINT ( 'NONE',  ( -26.29305231718578995, 58.70000000546237118, 19.10302069950538595 ) ) ;
#31074 = ADVANCED_FACE ( 'NONE', ( #6507, #16980 ), #20919, .T. ) ;
#31075 = CARTESIAN_POINT ( 'NONE',  ( -11.25946833292375793, 79.17500000273119554, -8.180482586598733619 ) ) ;
#31076 = CARTESIAN_POINT ( 'NONE',  ( 24.22776226481265383, 63.70013916574268364, 13.94119854578893580 ) ) ;
#31077 = CARTESIAN_POINT ( 'NONE',  ( 19.82091636218621389, 0.2000000000000057288, -14.40073868116559197 ) ) ;
#31078 = ADVANCED_FACE ( 'NONE', ( #10443 ), #15428, .T. ) ;
#31079 = CARTESIAN_POINT ( 'NONE',  ( 32.50000000000000000, 73.60000000546240528, -10.55989012756945833 ) ) ;
#31080 = CARTESIAN_POINT ( 'NONE',  ( -26.00068869287368756, 25.60677083333332149, -15.01150461594595775 ) ) ;
#31081 = CARTESIAN_POINT ( 'NONE',  ( 27.16883889988623935, 32.57500000273117990, -19.73931689729374384 ) ) ;
#31082 = CARTESIAN_POINT ( 'NONE',  ( 14.47279130897151767, 4.824999997268814234, 19.92008829642072953 ) ) ;
#31083 = ORIENTED_EDGE ( 'NONE', *, *, #14693, .T. ) ;
#31084 = CARTESIAN_POINT ( 'NONE',  ( 20.75514604977249178, 74.07500000273120122, 28.56700777964553950 ) ) ;
#31085 = CARTESIAN_POINT ( 'NONE',  ( 26.29305231718578995, 21.70000000546239249, -19.10302069950538240 ) ) ;
#31086 = CARTESIAN_POINT ( 'NONE',  ( 2.740863092043355209E-13, 45.08593750000000711, 30.02300923189239512 ) ) ;
#31087 = CARTESIAN_POINT ( 'NONE',  ( 28.01184896238290278, 64.70833333333334281, -7.505752307973347470 ) ) ;
#31088 = CARTESIAN_POINT ( 'NONE',  ( -33.58253175000000113, 51.27500000273118275, -10.91162601494193218 ) ) ;
#31089 = CARTESIAN_POINT ( 'NONE',  ( 26.29305231718578995, 63.70000000546238539, -19.10302069950538240 ) ) ;
#31090 = ORIENTED_EDGE ( 'NONE', *, *, #13215, .F. ) ;
#31091 = CARTESIAN_POINT ( 'NONE',  ( -10.37757302488624411, 42.72500000273119269, -31.93888565452638417 ) ) ;
#31092 = CARTESIAN_POINT ( 'NONE',  ( 5.147494310547535257, 55.94874572391552903, -32.49999999999996447 ) ) ;
#31093 = CARTESIAN_POINT ( 'NONE',  ( -2.162160676586881955E-15, 70.87500000273118417, -35.31076352940723240 ) ) ;
#31094 = CARTESIAN_POINT ( 'NONE',  ( 26.29305231718578995, 3.700000005462389385, -19.10302069950538240 ) ) ;
#31095 = CARTESIAN_POINT ( 'NONE',  ( 33.58253175000000823, 64.02500000273118985, 10.91162601494192685 ) ) ;
#31096 = CARTESIAN_POINT ( 'NONE',  ( 0.000000000000000000, 80.00000000000001421, -32.50000000000000000 ) ) ;
#31097 = CARTESIAN_POINT ( 'NONE',  ( -20.08610463437157989, 47.70000000000000995, -27.64615127144129758 ) ) ;
#31098 = CARTESIAN_POINT ( 'NONE',  ( 14.47279130897151767, 0.9249999972688209837, -19.92008829642072598 ) ) ;
#31099 = CARTESIAN_POINT ( 'NONE',  ( 10.37757302488624767, 11.97500000273118914, 31.93888565452638417 ) ) ;
#31100 = DIRECTION ( 'NONE',  ( -3.169619151431772337E-17, -0.9659258262890680902, -0.2588190451025213501 ) ) ;
#31101 = CARTESIAN_POINT ( 'NONE',  ( -6.950374756619247307, 36.91628499907601224, 26.09010956794245217 ) ) ;
#31102 = CARTESIAN_POINT ( 'NONE',  ( 4.300734207923761154, 77.97500000273119269, 13.23629886949340495 ) ) ;
#31103 = CARTESIAN_POINT ( 'NONE',  ( -33.58253175000000113, 77.27500000273118985, -10.91162601494193041 ) ) ;
#31104 = DIRECTION ( 'NONE',  ( 0.4999999999999996114, 0.000000000000000000, -0.8660254037844388186 ) ) ;
#31105 = VECTOR ( 'NONE', #31426, 1000.000000000000000 ) ;
#31106 = CARTESIAN_POINT ( 'NONE',  ( 33.58253175000000113, 74.47500000273116427, -10.91162601494193751 ) ) ;
#31107 = EDGE_LOOP ( 'NONE', ( #10750, #22854 ) ) ;
#31108 = CARTESIAN_POINT ( 'NONE',  ( 1.507698388325705758E-15, 11.62499999726880340, -24.62258325217400312 ) ) ;
#31109 = CARTESIAN_POINT ( 'NONE',  ( -23.41746824999999887, 1.524999997268801755, -7.608796670333730638 ) ) ;
#31110 = CARTESIAN_POINT ( 'NONE',  ( -24.20753774853756823, 46.23177083333331439, -13.97622843553588723 ) ) ;
#31111 = CARTESIAN_POINT ( 'NONE',  ( -10.37757302488623701, 61.52500000273118985, 31.93888565452638417 ) ) ;
#31112 = CARTESIAN_POINT ( 'NONE',  ( -27.16883889988624290, 15.17500000273118488, -19.73931689729374028 ) ) ;
#31113 = CARTESIAN_POINT ( 'NONE',  ( -10.37757302488623701, 1.775000002731188964, 31.93888565452638417 ) ) ;
#31114 = CARTESIAN_POINT ( 'NONE',  ( 24.20753774853731244, 33.62760416666666430, -13.97622843553633132 ) ) ;
#31115 = UNCERTAINTY_MEASURE_WITH_UNIT (LENGTH_MEASURE( 1.000000000000000082E-05 ), #33213, 'distance_accuracy_value', 'NONE');
#31116 = CARTESIAN_POINT ( 'NONE',  ( 0.04044903254992426173, 24.18006916759064140, -30.02300923189239867 ) ) ;
#31117 = CARTESIAN_POINT ( 'NONE',  ( 2.740863092043355209E-13, 65.71093749999997158, 30.02300923189239512 ) ) ;
#31118 = CARTESIAN_POINT ( 'NONE',  ( 27.16883889988624290, 1.925000002731186433, 19.73931689729373673 ) ) ;
#31119 = CARTESIAN_POINT ( 'NONE',  ( -5.147494310547322094, 56.05125428700922896, -32.50000000000003553 ) ) ;
#31120 = CARTESIAN_POINT ( 'NONE',  ( 20.08610463437158344, 40.69999999999999574, 27.64615127144129403 ) ) ;
#31121 = CARTESIAN_POINT ( 'NONE',  ( 27.16883889988623935, 44.32500000273117990, -19.73931689729374384 ) ) ;
#31122 = CARTESIAN_POINT ( 'NONE',  ( -18.94512977948575738, 7.424999997268811214, -13.76444248337723231 ) ) ;
#31123 = CARTESIAN_POINT ( 'NONE',  ( 5.779280353836490358E-15, 33.00000000546238965, 32.49999999999999289 ) ) ;
#31124 = ORIENTED_EDGE ( 'NONE', *, *, #33712, .F. ) ;
#31125 = CARTESIAN_POINT ( 'NONE',  ( 20.75514604977249178, 56.07500000273117990, 28.56700777964553950 ) ) ;
#31126 =( BOUNDED_CURVE ( )  B_SPLINE_CURVE ( 2, ( #13684, #24802, #29947, #24314, #788, #29608, #22240, #27047, #3540, #19004, #5951, #16925, #3872 ),
 .UNSPECIFIED., .F., .T. ) 
 B_SPLINE_CURVE_WITH_KNOTS ( ( 3, 2, 2, 2, 2, 2, 3 ),
 ( 0.3141025641025640969, 0.3153846153846153744, 0.3179487179487179294, 0.3205128205128205399, 0.3230769230769230949, 0.3256410256410256499, 0.3269230769230769273 ),
 .UNSPECIFIED. ) 
 CURVE ( )  GEOMETRIC_REPRESENTATION_ITEM ( )  RATIONAL_B_SPLINE_CURVE ( ( 0.9755282581475768211, 0.9755282581475768211, 1.000000000000000000, 0.9510565162951535312, 1.000000000000000000, 0.9510565162951535312, 1.000000000000000000, 0.9510565162951535312, 1.000000000000000000, 0.9510565162951535312, 1.000000000000000000, 0.9755282581475768211, 0.9755282581475768211 ) ) 
 REPRESENTATION_ITEM ( '' )  );
#31127 = CARTESIAN_POINT ( 'NONE',  ( -20.08610463437156923, 4.800000005462380592, 27.64615127144130113 ) ) ;
#31128 = CARTESIAN_POINT ( 'NONE',  ( -0.04044903254992426173, 46.52381916759065206, 27.95245687107223276 ) ) ;
#31129 = CARTESIAN_POINT ( 'NONE',  ( 10.37757302488624767, 77.97500000273119269, 31.93888565452638417 ) ) ;
#31130 = ORIENTED_EDGE ( 'NONE', *, *, #3857, .F. ) ;
#31131 = CARTESIAN_POINT ( 'NONE',  ( 33.58253175000000113, 26.22500000273119625, -10.91162601494193751 ) ) ;
#31132 = CARTESIAN_POINT ( 'NONE',  ( -26.00068869287368756, 15.29427083333332504, -15.01150461594595775 ) ) ;
#31133 = AXIS2_PLACEMENT_3D ( 'NONE', #26731, #19342, #3549 ) ;
#31134 = EDGE_LOOP ( 'NONE', ( #24234, #25254, #28544, #3898 ) ) ;
#31135 = CARTESIAN_POINT ( 'NONE',  ( -1.778240108872766143E-15, 30.00000000546237189, -32.49999999999999289 ) ) ;
#31136 = CARTESIAN_POINT ( 'NONE',  ( 6.486482029760649416E-15, 61.62500000273118417, 35.31076352940723240 ) ) ;
#31137 = CARTESIAN_POINT ( 'NONE',  ( 26.00068869287367335, 37.63802083333331439, 15.01150461594596308 ) ) ;
#31138 = CARTESIAN_POINT ( 'NONE',  ( -4.732186688966233175E-15, 17.50000000000000000, 25.76082449383753925 ) ) ;
#31139 = CARTESIAN_POINT ( 'NONE',  ( -14.47279130897152299, 2.424999997268802332, 19.92008829642072243 ) ) ;
#31140 = CARTESIAN_POINT ( 'NONE',  ( 10.37757302488624056, 6.525000002731207616, -31.93888565452638417 ) ) ;
#31141 = CARTESIAN_POINT ( 'NONE',  ( 2.067204126564591252E-14, 6.249999994537623671, -24.50000000000000000 ) ) ;
#31142 = CARTESIAN_POINT ( 'NONE',  ( 15.04653450569339945, 57.11159749907603356, 25.98046417659831775 ) ) ;
#31143 = CARTESIAN_POINT ( 'NONE',  ( 33.58253175000000113, 78.47500000273116427, -10.91162601494193751 ) ) ;
#31144 = DIRECTION ( 'NONE',  ( 1.000000000000000000, 0.000000000000000000, 0.000000000000000000 ) ) ;
#31145 = CARTESIAN_POINT ( 'NONE',  ( 32.50000000000000000, 19.60000000546238041, -10.55989012756945833 ) ) ;
#31146 = CARTESIAN_POINT ( 'NONE',  ( -2.092463501923844636E-15, 19.49999999999998934, -34.17252228774368916 ) ) ;
#31147 = CARTESIAN_POINT ( 'NONE',  ( -13.97622843553632777, 63.70572916666667140, -24.20753774853731599 ) ) ;
#31148 = CARTESIAN_POINT ( 'NONE',  ( -7.570916362186215665, 13.14999999453761426, 23.30088464923126423 ) ) ;
#31149 = CARTESIAN_POINT ( 'NONE',  ( -4.635254915624208216, 70.65000000546240244, 14.26584774442730463 ) ) ;
#31150 = CARTESIAN_POINT ( 'NONE',  ( -19.09188309203694445, 22.31250000000000000, -19.09188309203661049 ) ) ;
#31151 = CARTESIAN_POINT ( 'NONE',  ( -33.58253175000000113, 29.02500000273119340, -10.91162601494193218 ) ) ;
#31152 = CARTESIAN_POINT ( 'NONE',  ( 2.375766604868043252, 75.44874571845315359, -14.99999999999999822 ) ) ;
#31153 = CARTESIAN_POINT ( 'NONE',  ( -33.58253175000000113, 37.27500000273119696, -10.91162601494193218 ) ) ;
#31154 = CARTESIAN_POINT ( 'NONE',  ( 33.58253175000000113, 22.47500000273119269, -10.91162601494193574 ) ) ;
#31155 = CARTESIAN_POINT ( 'NONE',  ( -10.18398033115917123, -70.48295565631028126, 0.000000000000000000 ) ) ;
#31156 = CARTESIAN_POINT ( 'NONE',  ( 33.58253175000000113, 76.12500000273119838, -4.112674001490185761E-15 ) ) ;
#31157 = CARTESIAN_POINT ( 'NONE',  ( -26.29305231718578995, 26.70000000546238184, 19.10302069950538595 ) ) ;
#31158 = CARTESIAN_POINT ( 'NONE',  ( -32.50000000000000000, 58.10000000000000142, 10.55989012756946366 ) ) ;
#31159 = CARTESIAN_POINT ( 'NONE',  ( -14.47279130897151767, 15.32499999726880269, -19.92008829642072598 ) ) ;
#31160 = CARTESIAN_POINT ( 'NONE',  ( -2.162160676586882350E-15, 66.62500000273119838, -35.31076352940722529 ) ) ;
#31161 = CARTESIAN_POINT ( 'NONE',  ( -23.41746824999999887, 10.12499999726881938, -2.867812753649727150E-15 ) ) ;
#31162 = CARTESIAN_POINT ( 'NONE',  ( 10.37757302488624767, 73.97500000273120691, 31.93888565452638417 ) ) ;
#31163 = CARTESIAN_POINT ( 'NONE',  ( 20.75514604977249178, 9.825000002731188786, 28.56700777964553950 ) ) ;
#31164 = CARTESIAN_POINT ( 'NONE',  ( -4.523095164977116484E-15, 16.62499999726881583, 24.62258325217400312 ) ) ;
#31165 = CARTESIAN_POINT ( 'NONE',  ( -0.04044903254992426173, 19.02381916759064495, 27.95245687107223276 ) ) ;
#31166 = ADVANCED_FACE ( 'NONE', ( #10104 ), #31202, .T. ) ;
#31167 = ORIENTED_EDGE ( 'NONE', *, *, #5376, .F. ) ;
#31168 = CARTESIAN_POINT ( 'NONE',  ( -27.16883889988624290, 44.92500000273118133, -19.73931689729374028 ) ) ;
#31169 = ORIENTED_EDGE ( 'NONE', *, *, #18312, .F. ) ;
#31170 = CARTESIAN_POINT ( 'NONE',  ( 7.505752307973351023, 38.06770833333332860, 28.01184896238290278 ) ) ;
#31171 = CARTESIAN_POINT ( 'NONE',  ( 20.08610463437158344, 1.200000005462378283, 27.64615127144129403 ) ) ;
#31172 = CARTESIAN_POINT ( 'NONE',  ( 33.58253175000000823, 78.02500000273118985, 10.91162601494192863 ) ) ;
#31173 = CARTESIAN_POINT ( 'NONE',  ( -4.523095164977116484E-15, 4.624999997268820273, 24.62258325217400312 ) ) ;
#31174 = EDGE_CURVE ( 'NONE', #17247, #33874, #13992, .T. ) ;
#31175 = EDGE_CURVE ( 'NONE', #9461, #29890, #11700, .T. ) ;
#31176 = CARTESIAN_POINT ( 'NONE',  ( -23.41746824999999887, 17.62499999726882649, -2.867812753649727150E-15 ) ) ;
#31177 = CARTESIAN_POINT ( 'NONE',  ( 33.58253175000000113, 18.37500000273117706, -4.112674001490185761E-15 ) ) ;
#31178 = CARTESIAN_POINT ( 'NONE',  ( 32.50000000000000000, 17.50000000546236834, -3.980102097228898626E-15 ) ) ;
#31179 = CARTESIAN_POINT ( 'NONE',  ( 10.04305231718578817, 65.40000000000001990, -30.90933677959249337 ) ) ;
#31180 = CARTESIAN_POINT ( 'NONE',  ( 0.000000000000000000, 102.0000000000000284, 0.000000000000000000 ) ) ;
#31181 = CYLINDRICAL_SURFACE ( 'NONE', #17064, 32.50000000000000000 ) ;
#31182 = CARTESIAN_POINT ( 'NONE',  ( 0.04044903254992426173, 61.99256916759065206, -30.02300923189239867 ) ) ;
#31183 = CARTESIAN_POINT ( 'NONE',  ( 1.102182119232617911E-15, 122.0000000000000000, 9.000000000000001776 ) ) ;
#31184 = CARTESIAN_POINT ( 'NONE',  ( -20.50609665441004736, 42.93750000000000000, -20.50609665440969565 ) ) ;
#31185 = PRODUCT_CONTEXT ( 'NONE', #27191, 'mechanical' ) ;
#31186 = EDGE_CURVE ( 'NONE', #14369, #6559, #17832, .T. ) ;
#31187 = LINE ( 'NONE', #10769, #4195 ) ;
#31188 = CARTESIAN_POINT ( 'NONE',  ( -18.94512977948576093, 18.32499999726880446, 13.76444248337722698 ) ) ;
#31189 = CARTESIAN_POINT ( 'NONE',  ( -20.08610463437157989, 5.699999999999993960, -27.64615127144129758 ) ) ;
#31190 = CARTESIAN_POINT ( 'NONE',  ( 32.50000000000000000, 17.50000000546236834, -3.980102097228898626E-15 ) ) ;
#31191 = CARTESIAN_POINT ( 'NONE',  ( -19.11951029504797006, 51.81211833240936215, -19.06425588902558133 ) ) ;
#31192 = CARTESIAN_POINT ( 'NONE',  ( 6.486482029760649416E-15, 49.62500000273117706, 35.31076352940723240 ) ) ;
#31193 = CARTESIAN_POINT ( 'NONE',  ( -27.16883889988624290, 55.17500000273119554, -19.73931689729374028 ) ) ;
#31194 = CARTESIAN_POINT ( 'NONE',  ( -33.58253175000000113, 43.37500000273119838, 0.000000000000000000 ) ) ;
#31195 = CARTESIAN_POINT ( 'NONE',  ( 5.147494310547426899, 23.94874572391553968, -32.50000000000000000 ) ) ;
#31196 = CARTESIAN_POINT ( 'NONE',  ( -6.988114217768288228, 12.28645833333333037, -26.07999730980477437 ) ) ;
#31197 = LINE ( 'NONE', #2370, #21831 ) ;
#31198 = CARTESIAN_POINT ( 'NONE',  ( -32.50000000000000000, 22.40000000546237757, -10.55989012756945300 ) ) ;
#31199 = CARTESIAN_POINT ( 'NONE',  ( -10.04305231718579172, 77.59999999999999432, -30.90933677959248982 ) ) ;
#31200 = CARTESIAN_POINT ( 'NONE',  ( 33.58253175000000113, 14.12500000273118950, -4.112674001490185761E-15 ) ) ;
#31201 = CARTESIAN_POINT ( 'NONE',  ( 3.980102097228898626E-15, 52.00000000000000711, -32.50000000000000000 ) ) ;
#31202 = PLANE ( 'NONE',  #4580 ) ;
#31203 = FACE_OUTER_BOUND ( 'NONE', #32624, .T. ) ;
#31204 = CARTESIAN_POINT ( 'NONE',  ( 27.95245687107223276, 22.16368083240936215, -0.04044903255042905932 ) ) ;
#31205 = CARTESIAN_POINT ( 'NONE',  ( -10.04305231718578462, 36.90000000546238113, 30.90933677959249337 ) ) ;
#31206 = CARTESIAN_POINT ( 'NONE',  ( -24.50000000000000000, 10.64999999453762669, -7.960532557706207157 ) ) ;
#31207 = CARTESIAN_POINT ( 'NONE',  ( -20.75514604977248823, 28.82500000273117280, -28.56700777964554305 ) ) ;
#31208 = CARTESIAN_POINT ( 'NONE',  ( 26.07999730980490227, 40.93229166666666430, 6.988114217767821046 ) ) ;
#31209 = ORIENTED_EDGE ( 'NONE', *, *, #9244, .F. ) ;
#31210 = CARTESIAN_POINT ( 'NONE',  ( 27.16883889988624290, 61.92500000273119554, 19.73931689729373673 ) ) ;
#31211 = CARTESIAN_POINT ( 'NONE',  ( -20.50609665440969209, 45.51562500000000000, 20.50609665441005092 ) ) ;
#31212 = ORIENTED_EDGE ( 'NONE', *, *, #27607, .F. ) ;
#31213 = CARTESIAN_POINT ( 'NONE',  ( -7.505752307973343918, 15.72395833333332860, -28.01184896238290989 ) ) ;
#31214 = CARTESIAN_POINT ( 'NONE',  ( 28.00173670424549499, 18.30767333425730214, 7.543491769121417612 ) ) ;
#31215 = CARTESIAN_POINT ( 'NONE',  ( 33.58253175000000823, 6.025000002731191628, 10.91162601494192863 ) ) ;
#31216 = CARTESIAN_POINT ( 'NONE',  ( 2.375766604868044141, 79.69874572391552192, -14.99999999999999822 ) ) ;
#31217 = CARTESIAN_POINT ( 'NONE',  ( -20.75514604977248823, 37.07500000273120122, -28.56700777964554305 ) ) ;
#31218 = CARTESIAN_POINT ( 'NONE',  ( -32.50000000000000000, 38.60000000546239818, 10.55989012756946366 ) ) ;
#31219 = CARTESIAN_POINT ( 'NONE',  ( -15.00000000000000000, 78.09999999999999432, 4.873795443493597723 ) ) ;
#31220 = CARTESIAN_POINT ( 'NONE',  ( -10.04305231718579172, 47.60000000000000142, -30.90933677959248982 ) ) ;
#31221 = CARTESIAN_POINT ( 'NONE',  ( 33.58253175000000823, 22.02500000273117919, 10.91162601494192863 ) ) ;
#31222 = LINE ( 'NONE', #7715, #22512 ) ;
#31223 = CARTESIAN_POINT ( 'NONE',  ( 10.37757302488624056, 50.77500000273118985, -31.93888565452638417 ) ) ;
#31224 =( BOUNDED_CURVE ( )  B_SPLINE_CURVE ( 2, ( #19236, #29674, #6179, #16661, #27118, #24542, #11496, #21975, #19403, #6352, #16831, #9947, #10295 ),
 .UNSPECIFIED., .F., .T. ) 
 B_SPLINE_CURVE_WITH_KNOTS ( ( 3, 2, 2, 2, 2, 2, 3 ),
 ( 0.4038461538461538547, 0.4051282051282051322, 0.4076923076923076872, 0.4102564102564102422, 0.4128205128205127972, 0.4153846153846154077, 0.4166666666666666852 ),
 .UNSPECIFIED. ) 
 CURVE ( )  GEOMETRIC_REPRESENTATION_ITEM ( )  RATIONAL_B_SPLINE_CURVE ( ( 0.9755282581475768211, 0.9755282581475768211, 1.000000000000000000, 0.9510565162951535312, 1.000000000000000000, 0.9510565162951535312, 1.000000000000000000, 0.9510565162951535312, 1.000000000000000000, 0.9510565162951535312, 1.000000000000000000, 0.9755282581475768211, 0.9755282581475768211 ) ) 
 REPRESENTATION_ITEM ( '' )  );
#31225 = CARTESIAN_POINT ( 'NONE',  ( -20.08610463437157989, 29.69999999999999574, -27.64615127144129758 ) ) ;
#31226 = CARTESIAN_POINT ( 'NONE',  ( 26.29305231718578995, 25.19999999999999929, -19.10302069950538240 ) ) ;
#31227 = CARTESIAN_POINT ( 'NONE',  ( -19.82091636218621389, 3.200000000000008171, 14.40073868116558842 ) ) ;
#31228 = EDGE_CURVE ( 'NONE', #11992, #16018, #2196, .T. ) ;
#31229 = CARTESIAN_POINT ( 'NONE',  ( -27.16883889988623935, 71.32500000273117280, 19.73931689729374739 ) ) ;
#31230 = CARTESIAN_POINT ( 'NONE',  ( -33.35123603814785298, 67.00000000000000000, -2.296425957314693012 ) ) ;
#31231 = CARTESIAN_POINT ( 'NONE',  ( 5.779280353836490358E-15, 38.50000000000000000, 32.49999999999999289 ) ) ;
#31232 = CARTESIAN_POINT ( 'NONE',  ( -10.37757302488623701, 57.77500000273119696, 31.93888565452638417 ) ) ;
#31233 = CYLINDRICAL_SURFACE ( 'NONE', #30337, 32.50000000000000000 ) ;
#31234 = CARTESIAN_POINT ( 'NONE',  ( 27.16883889988623935, 12.32500000273117990, -19.73931689729374384 ) ) ;
#31235 = CARTESIAN_POINT ( 'NONE',  ( -13.94119854578936923, 27.33111083425731280, -24.22776226481241224 ) ) ;
#31236 = FACE_OUTER_BOUND ( 'NONE', #29203, .T. ) ;
#31237 = CARTESIAN_POINT ( 'NONE',  ( 20.75514604977248467, 34.42500000273117422, -28.56700777964554305 ) ) ;
#31238 = CARTESIAN_POINT ( 'NONE',  ( -1.778240108872766143E-15, 46.00000000546238255, -32.49999999999999289 ) ) ;
#31239 = CARTESIAN_POINT ( 'NONE',  ( -1.778240108872766143E-15, 3.500000000000004441, -32.49999999999999289 ) ) ;
#31240 = CARTESIAN_POINT ( 'NONE',  ( 8.601468415847516980, 74.17500000273122396, -11.83890561707634603 ) ) ;
#31241 = CARTESIAN_POINT ( 'NONE',  ( 0.04044903255045854962, 50.52305583240934794, 30.02300923189239867 ) ) ;
#31242 = CARTESIAN_POINT ( 'NONE',  ( -2.092463501923844636E-15, 52.00000000546236834, -34.17252228774368916 ) ) ;
#31243 = CARTESIAN_POINT ( 'NONE',  ( 8.601468415847520532, 76.07500000273115859, 11.83890561707634781 ) ) ;
#31244 = CARTESIAN_POINT ( 'NONE',  ( 32.50000000000000000, 61.00000000000000000, -3.980102097228898626E-15 ) ) ;
#31245 = CARTESIAN_POINT ( 'NONE',  ( -6.988114217768288228, 19.16145833333332860, -26.07999730980477437 ) ) ;
#31246 = CARTESIAN_POINT ( 'NONE',  ( -32.50000000000000000, 54.10000000000000853, 10.55989012756946366 ) ) ;
#31247 = CARTESIAN_POINT ( 'NONE',  ( -26.29305231718579350, 66.30000000546237970, -19.10302069950537884 ) ) ;
#31248 = CARTESIAN_POINT ( 'NONE',  ( 30.02300923189239512, 20.16406249999999645, -2.619432448724977703E-13 ) ) ;
#31249 = CARTESIAN_POINT ( 'NONE',  ( -33.58253175000000113, 37.27500000273119696, -10.91162601494193218 ) ) ;
#31250 = CARTESIAN_POINT ( 'NONE',  ( -23.41746824999999887, 10.12499999726881938, -2.867812753649727150E-15 ) ) ;
#31251 = ORIENTED_EDGE ( 'NONE', *, *, #5665, .F. ) ;
#31252 = CARTESIAN_POINT ( 'NONE',  ( 27.16883889988624290, 74.17500000273119554, 19.73931689729373673 ) ) ;
#31253 = CARTESIAN_POINT ( 'NONE',  ( 32.50000000000000000, 23.60000000546236976, -10.55989012756945833 ) ) ;
#31254 = CARTESIAN_POINT ( 'NONE',  ( -20.50609665440969209, 42.07812499999999289, 20.50609665441005092 ) ) ;
#31255 = CARTESIAN_POINT ( 'NONE',  ( -15.01150461594595775, 62.55989583333332860, 26.00068869287368756 ) ) ;
#31256 = CARTESIAN_POINT ( 'NONE',  ( -27.16883889988624290, 51.17500000273117422, -19.73931689729374028 ) ) ;
#31257 = CARTESIAN_POINT ( 'NONE',  ( -10.04305231718578462, 56.90000000546238823, 30.90933677959249337 ) ) ;
#31258 = CARTESIAN_POINT ( 'NONE',  ( 3.469446951953614189E-15, -57.99999999999999289, 0.000000000000000000 ) ) ;
#31259 = CARTESIAN_POINT ( 'NONE',  ( -20.75514604977248112, 43.42500000273117422, 28.56700777964554661 ) ) ;
#31260 = CARTESIAN_POINT ( 'NONE',  ( -12.13525491562421088, 76.05000000546240813, -8.816778784387096835 ) ) ;
#31261 = CARTESIAN_POINT ( 'NONE',  ( 33.58253175000000113, 70.37500000273119838, -4.112674001490185761E-15 ) ) ;
#31262 = CARTESIAN_POINT ( 'NONE',  ( -10.04305231718579172, 2.100000005462371533, -30.90933677959248982 ) ) ;
#31263 = CARTESIAN_POINT ( 'NONE',  ( 6.486482029760648627E-15, 63.62500000273117706, 35.31076352940722529 ) ) ;
#31264 = CARTESIAN_POINT ( 'NONE',  ( -28.01184896238290278, 14.86458333333333037, 7.505752307973363457 ) ) ;
#31265 = CARTESIAN_POINT ( 'NONE',  ( 10.04305231718579705, 44.60000000000000142, 30.90933677959248982 ) ) ;
#31266 = CARTESIAN_POINT ( 'NONE',  ( -18.94512977948575738, 5.424999997268809437, -13.76444248337723231 ) ) ;
#31267 = ADVANCED_FACE ( 'NONE', ( #2720 ), #13365, .F. ) ;
#31268 = CARTESIAN_POINT ( 'NONE',  ( 20.75514604977249178, 10.07500000273118168, 28.56700777964553950 ) ) ;
#31269 = DIRECTION ( 'NONE',  ( -0.000000000000000000, 1.000000000000000000, -0.000000000000000000 ) ) ;
#31270 = CARTESIAN_POINT ( 'NONE',  ( 27.95245687107223276, 35.91368083240935505, -0.04044903255042905932 ) ) ;
#31271 = CARTESIAN_POINT ( 'NONE',  ( -8.960552108402742093E-16, 76.87500000273115575, -14.63369212191046387 ) ) ;
#31272 = CARTESIAN_POINT ( 'NONE',  ( -27.16883889988624290, 77.17500000273119554, -19.73931689729374028 ) ) ;
#31273 = DIRECTION ( 'NONE',  ( 0.000000000000000000, 0.000000000000000000, -1.000000000000000000 ) ) ;
#31274 = EDGE_CURVE ( 'NONE', #26581, #17842, #28794, .T. ) ;
#31275 = CARTESIAN_POINT ( 'NONE',  ( 33.58253175000000113, 74.37500000273118417, -4.112674001490185761E-15 ) ) ;
#31276 = ORIENTED_EDGE ( 'NONE', *, *, #3708, .F. ) ;
#31277 = CARTESIAN_POINT ( 'NONE',  ( -18.94512977948575738, 15.92499999726881832, -13.76444248337723231 ) ) ;
#31278 = CARTESIAN_POINT ( 'NONE',  ( 19.09188309203694800, 61.84374999999998579, 19.09188309203660694 ) ) ;
#31279 = CARTESIAN_POINT ( 'NONE',  ( -20.75514604977248112, 53.42500000273117422, 28.56700777964554661 ) ) ;
#31280 = CARTESIAN_POINT ( 'NONE',  ( -10.37757302488623701, 17.77500000273117564, 31.93888565452638417 ) ) ;
#31281 = CARTESIAN_POINT ( 'NONE',  ( 33.58253175000000823, 2.275000002731194293, 10.91162601494192863 ) ) ;
#31282 = CARTESIAN_POINT ( 'NONE',  ( 13.97622843553589966, 36.77864583333332860, -24.20753774853756113 ) ) ;
#31283 = CARTESIAN_POINT ( 'NONE',  ( 0.04044903254992426173, 27.61756916759064140, -30.02300923189239867 ) ) ;
#31284 = CARTESIAN_POINT ( 'NONE',  ( -20.47846945139866648, 20.01524333240935505, 20.53372385742108008 ) ) ;
#31285 = CARTESIAN_POINT ( 'NONE',  ( 6.277390505771533514E-15, 75.00000000546238255, 34.17252228774368916 ) ) ;
#31286 = CARTESIAN_POINT ( 'NONE',  ( 33.35123603814782456, 52.00000000000003553, 2.296425957315384458 ) ) ;
#31287 = CARTESIAN_POINT ( 'NONE',  ( -33.58253175000000113, 47.02500000273117564, -10.91162601494193041 ) ) ;
#31288 = CARTESIAN_POINT ( 'NONE',  ( -4.523095164977116484E-15, 6.124999997268802510, 24.62258325217400312 ) ) ;
#31289 = CARTESIAN_POINT ( 'NONE',  ( -5.147494310547423346, 2.948745723915526806, 32.50000000000000000 ) ) ;
#31290 = ORIENTED_EDGE ( 'NONE', *, *, #7894, .T. ) ;
#31291 = CARTESIAN_POINT ( 'NONE',  ( -10.37757302488624411, 56.97500000273118559, -31.93888565452638417 ) ) ;
#31292 = DIRECTION ( 'NONE',  ( 0.6936844842780659492, 0.7202789989107510893, 8.495184832893160525E-17 ) ) ;
#31293 = CIRCLE ( 'NONE', #15978, 9.000000000000001776 ) ;
#31294 = CARTESIAN_POINT ( 'NONE',  ( 19.06425588902592239, 42.65663166759063785, 19.11951029504763611 ) ) ;
#31295 = CARTESIAN_POINT ( 'NONE',  ( 33.58253175000000113, 78.37500000273116996, -4.112674001490185761E-15 ) ) ;
#31296 = ORIENTED_EDGE ( 'NONE', *, *, #4186, .T. ) ;
#31297 = CARTESIAN_POINT ( 'NONE',  ( 33.58253175000000113, 22.12500000273119483, -4.112674001490185761E-15 ) ) ;
#31298 = CARTESIAN_POINT ( 'NONE',  ( 7.505752307973351023, 14.00520833333333215, 28.01184896238290278 ) ) ;
#31299 = ORIENTED_EDGE ( 'NONE', *, *, #32725, .F. ) ;
#31300 = CARTESIAN_POINT ( 'NONE',  ( -32.50000000000000000, 14.40000000546236869, -10.55989012756945300 ) ) ;
#31301 = CARTESIAN_POINT ( 'NONE',  ( 10.37757302488624767, 63.72500000273117848, 31.93888565452638417 ) ) ;
#31302 = CARTESIAN_POINT ( 'NONE',  ( -15.01150461594595775, 52.24739583333332860, 26.00068869287368756 ) ) ;
#31303 = CARTESIAN_POINT ( 'NONE',  ( 24.50000000000000000, 16.00000000000001421, 0.000000000000000000 ) ) ;
#31304 = CARTESIAN_POINT ( 'NONE',  ( -23.41746825000000243, 2.224999997268808816, 7.608796670333725309 ) ) ;
#31305 = VECTOR ( 'NONE', #14760, 1000.000000000000000 ) ;
#31306 = CARTESIAN_POINT ( 'NONE',  ( 33.58253175000000113, 2.225000002731166937, -10.91162601494193751 ) ) ;
#31307 = CARTESIAN_POINT ( 'NONE',  ( -20.47846945139866648, 61.26524333240935505, 20.53372385742108008 ) ) ;
#31308 = CARTESIAN_POINT ( 'NONE',  ( -2.375766604868044141, 79.80125428700920054, -14.99999999999999822 ) ) ;
#31309 = CARTESIAN_POINT ( 'NONE',  ( 15.00000000000000000, 81.09999999999999432, -4.873795443493596835 ) ) ;
#31310 = CARTESIAN_POINT ( 'NONE',  ( -1.778240108872766143E-15, 59.50000000000000711, -32.49999999999999289 ) ) ;
#31311 = CARTESIAN_POINT ( 'NONE',  ( 20.08610463437157279, 15.29999999999998472, -27.64615127144129758 ) ) ;
#31312 = CARTESIAN_POINT ( 'NONE',  ( 24.20753774853731244, 64.56510416666667140, -13.97622843553633132 ) ) ;
#31313 = ADVANCED_FACE ( 'NONE', ( #4776 ), #12671, .F. ) ;
#31314 = EDGE_CURVE ( 'NONE', #21689, #30261, #28456, .T. ) ;
#31315 = CARTESIAN_POINT ( 'NONE',  ( -24.50000000000000355, 14.64999999453761603, -7.960532557706207157 ) ) ;
#31316 = CARTESIAN_POINT ( 'NONE',  ( 9.270509831248425314, 70.95000000546234276, 12.75976212528059683 ) ) ;
#31317 = CARTESIAN_POINT ( 'NONE',  ( -6.988114217768288228, 32.91145833333332860, -26.07999730980477437 ) ) ;
#31318 = CARTESIAN_POINT ( 'NONE',  ( 10.37757302488624767, 33.72500000273117848, 31.93888565452638417 ) ) ;
#31319 = CARTESIAN_POINT ( 'NONE',  ( 27.16883889988624290, 75.92500000273120975, 19.73931689729373673 ) ) ;
#31320 = VECTOR ( 'NONE', #19199, 1000.000000000000000 ) ;
#31321 = CARTESIAN_POINT ( 'NONE',  ( -2.162160676586881955E-15, 36.87500000273116996, -35.31076352940723240 ) ) ;
#31322 = CARTESIAN_POINT ( 'NONE',  ( 20.75514604977249178, 16.07500000273119767, 28.56700777964553950 ) ) ;
#31323 = CARTESIAN_POINT ( 'NONE',  ( -15.00000000000000000, 79.90000000000000568, -4.873795443493594171 ) ) ;
#31324 = CARTESIAN_POINT ( 'NONE',  ( 0.04044903254993986036, 48.24256916759064495, -27.95245687107223986 ) ) ;
#31325 = CARTESIAN_POINT ( 'NONE',  ( -27.16883889988624290, 78.92500000273116711, -19.73931689729374028 ) ) ;
#31326 = CARTESIAN_POINT ( 'NONE',  ( -20.08610463437157989, 65.69999999999998863, -27.64615127144129758 ) ) ;
#31327 =( BOUNDED_CURVE ( )  B_SPLINE_CURVE ( 2, ( #31238, #7731, #5330, #10481, #18555, #18220, #23528, #8069, #28664, #5159, #15644, #28999, #5499 ),
 .UNSPECIFIED., .F., .T. ) 
 B_SPLINE_CURVE_WITH_KNOTS ( ( 3, 2, 2, 2, 2, 2, 3 ),
 ( 0.4166666666666666852, 0.4179487179487179627, 0.4205128205128205177, 0.4230769230769230727, 0.4256410256410256276, 0.4282051282051281826, 0.4294871794871795156 ),
 .UNSPECIFIED. ) 
 CURVE ( )  GEOMETRIC_REPRESENTATION_ITEM ( )  RATIONAL_B_SPLINE_CURVE ( ( 0.9755282581475768211, 0.9755282581475768211, 1.000000000000000000, 0.9510565162951535312, 1.000000000000000000, 0.9510565162951535312, 1.000000000000000000, 0.9510565162951535312, 1.000000000000000000, 0.9510565162951535312, 1.000000000000000000, 0.9755282581475762660, 0.9755282581475768211 ) ) 
 REPRESENTATION_ITEM ( '' )  );
#31328 = CARTESIAN_POINT ( 'NONE',  ( -32.50000000000000000, 57.99999999999997868, 0.000000000000000000 ) ) ;
#31329 = DIRECTION ( 'NONE',  ( -0.000000000000000000, -1.000000000000000000, -0.000000000000000000 ) ) ;
#31330 = CARTESIAN_POINT ( 'NONE',  ( 6.486482029760648627E-15, 61.62500000273118417, 35.31076352940722529 ) ) ;
#31331 = CARTESIAN_POINT ( 'NONE',  ( 1.507698388325705758E-15, 7.624999997268814056, -24.62258325217400312 ) ) ;
#31332 = CARTESIAN_POINT ( 'NONE',  ( -27.16883889988623935, 73.57500000273118701, 19.73931689729374739 ) ) ;
#31333 = CARTESIAN_POINT ( 'NONE',  ( 10.37757302488624767, 7.725000002731185589, 31.93888565452638417 ) ) ;
#31334 = CARTESIAN_POINT ( 'NONE',  ( 23.41746825000000243, 0.7249999972688272454, -7.608796670333727974 ) ) ;
#31335 = CARTESIAN_POINT ( 'NONE',  ( -19.06425588902591173, 13.43788166759064140, -19.11951029504763611 ) ) ;
#31336 = VERTEX_POINT ( 'NONE', #18178 ) ;
#31337 = CARTESIAN_POINT ( 'NONE',  ( 33.58253175000000113, 44.22500000273117138, -10.91162601494193751 ) ) ;
#31338 = VERTEX_POINT ( 'NONE', #23832 ) ;
#31339 = CARTESIAN_POINT ( 'NONE',  ( -7.505752307972844761, 45.22916666666665719, 28.01184896238304134 ) ) ;
#31340 = CARTESIAN_POINT ( 'NONE',  ( -32.50000000000000000, 79.90000000000000568, -10.55989012756945300 ) ) ;
#31341 = CARTESIAN_POINT ( 'NONE',  ( 10.04305231718578817, 3.900000005462381125, -30.90933677959249337 ) ) ;
#31342 = CARTESIAN_POINT ( 'NONE',  ( -26.29305231718579350, 71.79999999999999716, -19.10302069950537884 ) ) ;
#31343 = CARTESIAN_POINT ( 'NONE',  ( 7.505752307972854531, 22.88541666666666430, -28.01184896238303423 ) ) ;
#31344 = CARTESIAN_POINT ( 'NONE',  ( 23.41746825000000243, 16.72499999726881725, -7.608796670333727974 ) ) ;
#31345 = CARTESIAN_POINT ( 'NONE',  ( -27.16883889988623935, 15.57500000273118168, 19.73931689729374739 ) ) ;
#31346 = CARTESIAN_POINT ( 'NONE',  ( 10.04305231718578817, 59.40000000000000568, -30.90933677959249337 ) ) ;
#31347 = CARTESIAN_POINT ( 'NONE',  ( -3.880418787951146697, 4.551254281546843750, -24.49999999999999645 ) ) ;
#31348 = CARTESIAN_POINT ( 'NONE',  ( 20.08610463437157279, 73.80000000546236549, -27.64615127144129758 ) ) ;
#31349 = CARTESIAN_POINT ( 'NONE',  ( 30.02300923189239867, 35.91368083240935505, -0.04044903255044467877 ) ) ;
#31350 = CARTESIAN_POINT ( 'NONE',  ( 2.688165632520823219E-15, 77.87500000273118417, 14.63369212191046387 ) ) ;
#31351 = CARTESIAN_POINT ( 'NONE',  ( -26.00068869287340334, 35.34635416666666430, 15.01150461594643559 ) ) ;
#31352 = ITEM_DEFINED_TRANSFORMATION ( 'NONE', 'NONE', #11745,  #1376 ) ;
#31353 = APPLICATION_CONTEXT ( 'automotive_design' ) ;
#31354 = CARTESIAN_POINT ( 'NONE',  ( -31.38736896855613523, -89.55944200217849982, 3.843844094099923719E-15 ) ) ;
#31355 = CARTESIAN_POINT ( 'NONE',  ( 24.50000000000000000, 16.09999999999998721, -7.960532557706203605 ) ) ;
#31356 = CARTESIAN_POINT ( 'NONE',  ( -26.29305231718578995, 6.199999999999983302, 19.10302069950538595 ) ) ;
#31357 = DIRECTION ( 'NONE',  ( -0.000000000000000000, -1.000000000000000000, -0.000000000000000000 ) ) ;
#31358 = CARTESIAN_POINT ( 'NONE',  ( -13.94119854578892514, 50.80951416574269075, 24.22776226481266448 ) ) ;
#31359 = CARTESIAN_POINT ( 'NONE',  ( -33.58253175000000113, 53.12500000273118417, 0.000000000000000000 ) ) ;
#31360 = CARTESIAN_POINT ( 'NONE',  ( -10.37757302488624411, 56.97500000273118559, -31.93888565452638417 ) ) ;
#31361 = CARTESIAN_POINT ( 'NONE',  ( -2.162160676586882350E-15, 42.87500000273119127, -35.31076352940722529 ) ) ;
#31362 = CARTESIAN_POINT ( 'NONE',  ( -14.45873412499999944, 81.68750000136559208, 0.000000000000000000 ) ) ;
#31363 = CARTESIAN_POINT ( 'NONE',  ( 0.000000000000000000, 0.000000000000000000, 24.50000000000000000 ) ) ;
#31364 = CARTESIAN_POINT ( 'NONE',  ( -3.880418787951118276, 8.551254281546841085, -24.50000000000000355 ) ) ;
#31365 = CARTESIAN_POINT ( 'NONE',  ( -40.00000000000000711, 66.99999999999998579, 23.09401076758504345 ) ) ;
#31366 = CARTESIAN_POINT ( 'NONE',  ( -20.08610463437156923, 78.29999999999999716, 27.64615127144130113 ) ) ;
#31367 = CARTESIAN_POINT ( 'NONE',  ( -20.75514604977248823, 16.82500000273120122, -28.56700777964554305 ) ) ;
#31368 = CARTESIAN_POINT ( 'NONE',  ( 10.04305231718579705, 6.599999999999994316, 30.90933677959248982 ) ) ;
#31369 = DIRECTION ( 'NONE',  ( 0.000000000000000000, 0.000000000000000000, -1.000000000000000000 ) ) ;
#31370 = CARTESIAN_POINT ( 'NONE',  ( 0.000000000000000000, 80.00000000000001421, 0.000000000000000000 ) ) ;
#31371 = CARTESIAN_POINT ( 'NONE',  ( -19.11951029504797006, 17.43711833240935505, -19.06425588902558133 ) ) ;
#31372 = CARTESIAN_POINT ( 'NONE',  ( -32.50000000000000000, 34.60000000546236976, 10.55989012756946366 ) ) ;
#31373 = CARTESIAN_POINT ( 'NONE',  ( 24.50000000000000000, 17.64999999453763735, 7.960532557706212486 ) ) ;
#31374 = CARTESIAN_POINT ( 'NONE',  ( -20.75514604977248823, 26.82500000273117280, -28.56700777964554305 ) ) ;
#31375 = CARTESIAN_POINT ( 'NONE',  ( -26.07999730980490583, 42.65104166666666430, -6.988114217767815717 ) ) ;
#31376 = EDGE_CURVE ( 'NONE', #9001, #24073, #14190, .T. ) ;
#31377 = ORIENTED_EDGE ( 'NONE', *, *, #33041, .F. ) ;
#31378 = CARTESIAN_POINT ( 'NONE',  ( -33.58253175000000113, 63.22500000273119269, 10.91162601494193929 ) ) ;
#31379 = CARTESIAN_POINT ( 'NONE',  ( -15.01150461594595775, 48.80989583333332860, 26.00068869287368756 ) ) ;
#31380 = VERTEX_POINT ( 'NONE', #23277 ) ;
#31381 = CARTESIAN_POINT ( 'NONE',  ( -20.50609665441004736, 15.43749999999999645, -20.50609665440969565 ) ) ;
#31382 = CARTESIAN_POINT ( 'NONE',  ( 14.97647472619947351, 11.86236083425730925, 26.02091320914850314 ) ) ;
#31383 = ORIENTED_EDGE ( 'NONE', *, *, #18882, .F. ) ;
#31384 = CARTESIAN_POINT ( 'NONE',  ( 33.58253175000000113, 4.125000002731193938, -4.112674001490185761E-15 ) ) ;
#31385 = CIRCLE ( 'NONE', #12752, 10.69578794377714104 ) ;
#31386 = CARTESIAN_POINT ( 'NONE',  ( 14.47279130897151767, 0.9249999972688209837, -19.92008829642072598 ) ) ;
#31387 = CARTESIAN_POINT ( 'NONE',  ( -27.16883889988623935, 35.57500000273120122, 19.73931689729374739 ) ) ;
#31388 = CARTESIAN_POINT ( 'NONE',  ( -10.04305231718579172, 38.10000000546237686, -30.90933677959248982 ) ) ;
#31389 = CARTESIAN_POINT ( 'NONE',  ( -15.00000000000000000, 74.00000000000001421, 0.000000000000000000 ) ) ;
#31390 = CARTESIAN_POINT ( 'NONE',  ( 26.00068869287340334, 64.56510416666667140, -15.01150461594642316 ) ) ;
#31391 = CARTESIAN_POINT ( 'NONE',  ( -20.75514604977248112, 23.42500000273119909, 28.56700777964554661 ) ) ;
#31392 = CARTESIAN_POINT ( 'NONE',  ( 11.54700538379251817, 96.00000000000002842, 19.99999999999999645 ) ) ;
#31393 = CARTESIAN_POINT ( 'NONE',  ( -27.16883889988623935, 51.57500000273118701, 19.73931689729374739 ) ) ;
#31394 =( LENGTH_UNIT ( ) NAMED_UNIT ( * ) SI_UNIT ( .MILLI., .METRE. ) );
#31395 = CARTESIAN_POINT ( 'NONE',  ( 26.29305231718578995, 27.19999999999998863, -19.10302069950538240 ) ) ;
#31396 = CARTESIAN_POINT ( 'NONE',  ( -10.04305231718578462, 26.40000000000000568, 30.90933677959249337 ) ) ;
#31397 = CARTESIAN_POINT ( 'NONE',  ( 24.50000000000000000, 4.000000000000003553, 0.000000000000000000 ) ) ;
#31398 = CARTESIAN_POINT ( 'NONE',  ( 27.16883889988624290, 69.92500000273119554, 19.73931689729373673 ) ) ;
#31399 = CARTESIAN_POINT ( 'NONE',  ( -24.50000000000000000, 2.749999994537621895, -3.000384657911015469E-15 ) ) ;
#31400 = CARTESIAN_POINT ( 'NONE',  ( 5.779280353836490358E-15, 1.000000005462375885, 32.49999999999999289 ) ) ;
#31401 = CARTESIAN_POINT ( 'NONE',  ( -33.58253175000000113, 57.37500000273118417, 0.000000000000000000 ) ) ;
#31402 = CARTESIAN_POINT ( 'NONE',  ( 5.147494310547434893, 7.051254287009218302, 32.49999999999999289 ) ) ;
#31403 = CARTESIAN_POINT ( 'NONE',  ( -2.162160676586881955E-15, 12.62500000273118772, -35.31076352940723240 ) ) ;
#31404 = CARTESIAN_POINT ( 'NONE',  ( 14.01125832528286352, 27.90402750092397355, -24.18731323226246843 ) ) ;
#31405 = CARTESIAN_POINT ( 'NONE',  ( -0.3462681986482577523, 67.00000000000001421, -33.37691080753737083 ) ) ;
#31406 = CARTESIAN_POINT ( 'NONE',  ( -33.58253175000000113, 3.475000002731185589, 10.91162601494193929 ) ) ;
#31407 = CARTESIAN_POINT ( 'NONE',  ( 20.75514604977248467, 36.42500000273118843, -28.56700777964554305 ) ) ;
#31408 = CARTESIAN_POINT ( 'NONE',  ( -26.29305231718578995, 64.70000000546237118, 19.10302069950538595 ) ) ;
#31409 = CARTESIAN_POINT ( 'NONE',  ( 33.58253175000000113, 52.47500000273117848, -10.91162601494193574 ) ) ;
#31410 = CIRCLE ( 'NONE', #1802, 24.50000000000000000 ) ;
#31411 = CARTESIAN_POINT ( 'NONE',  ( -8.960552108402744065E-16, 76.37500000273114154, -14.63369212191046209 ) ) ;
#31412 = CARTESIAN_POINT ( 'NONE',  ( 28.00173670424535644, 49.52045166574269075, -7.543491769121920321 ) ) ;
#31413 = CARTESIAN_POINT ( 'NONE',  ( -20.08610463437156923, 56.80000000546240102, 27.64615127144130113 ) ) ;
#31414 = CARTESIAN_POINT ( 'NONE',  ( 4.300734207923761154, 73.97500000273122112, 13.23629886949340495 ) ) ;
#31415 = FILL_AREA_STYLE_COLOUR ( '', #17819 ) ;
#31416 = CARTESIAN_POINT ( 'NONE',  ( -6.988114217767819270, 21.16666666666666430, 26.07999730980490583 ) ) ;
#31417 = CARTESIAN_POINT ( 'NONE',  ( 14.47279130897151767, 1.424999997268804997, -19.92008829642072598 ) ) ;
#31418 = CARTESIAN_POINT ( 'NONE',  ( 32.50000000000000000, 69.50000000546238255, -3.980102097228898626E-15 ) ) ;
#31419 = CARTESIAN_POINT ( 'NONE',  ( 7.505752307973351023, 20.88020833333333215, 28.01184896238290278 ) ) ;
#31420 = CARTESIAN_POINT ( 'NONE',  ( 6.486482029760649416E-15, 31.87500000273119127, 35.31076352940723240 ) ) ;
#31421 = CARTESIAN_POINT ( 'NONE',  ( 23.41746824999999887, 13.22499999726881192, -7.608796670333727974 ) ) ;
#31422 = ORIENTED_EDGE ( 'NONE', *, *, #14830, .F. ) ;
#31423 = CARTESIAN_POINT ( 'NONE',  ( -20.47846945139902175, 44.37538166759063785, -20.53372385742072481 ) ) ;
#31424 = CARTESIAN_POINT ( 'NONE',  ( 32.50000000000000000, 19.50000000546238255, -3.980102097228898626E-15 ) ) ;
#31425 = CARTESIAN_POINT ( 'NONE',  ( -28.01184896238304134, 56.40104166666666430, -7.505752307972844761 ) ) ;
#31426 = DIRECTION ( 'NONE',  ( -0.000000000000000000, -1.000000000000000000, -0.000000000000000000 ) ) ;
#31427 = CARTESIAN_POINT ( 'NONE',  ( 33.58253175000000823, 56.27500000273116854, 10.91162601494192863 ) ) ;
#31428 = CARTESIAN_POINT ( 'NONE',  ( -20.08610463437156923, 56.80000000546240102, 27.64615127144130113 ) ) ;
#31429 = CARTESIAN_POINT ( 'NONE',  ( 0.000000000000000000, 52.00000000000000711, 0.000000000000000000 ) ) ;
#31430 = CARTESIAN_POINT ( 'NONE',  ( 10.37757302488624056, 42.52500000273118275, -31.93888565452638417 ) ) ;
#31431 = CARTESIAN_POINT ( 'NONE',  ( 15.00000000000000355, 73.15000000546240244, 4.873795443493592394 ) ) ;
#31432 = CARTESIAN_POINT ( 'NONE',  ( -27.16883889988623935, 69.57500000273120122, 19.73931689729374739 ) ) ;
#31433 = DIRECTION ( 'NONE',  ( -0.000000000000000000, -1.000000000000000000, -0.000000000000000000 ) ) ;
#31434 = AXIS2_PLACEMENT_3D ( 'NONE', #13183, #7526, #15775 ) ;
#31435 = CARTESIAN_POINT ( 'NONE',  ( -20.75514604977248112, 61.42500000273118133, 28.56700777964554661 ) ) ;
#31436 = CARTESIAN_POINT ( 'NONE',  ( -15.01150461594595775, 24.74739583333332860, 26.00068869287368756 ) ) ;
#31437 = CARTESIAN_POINT ( 'NONE',  ( -32.50000000000000000, 47.99999999999998579, 0.000000000000000000 ) ) ;
#31438 = CARTESIAN_POINT ( 'NONE',  ( -23.41746825000000243, 3.524999997268826402, -7.608796670333730638 ) ) ;
#31439 = CARTESIAN_POINT ( 'NONE',  ( -20.75514604977248112, 9.675000002731193760, 28.56700777964554661 ) ) ;
#31440 = DIRECTION ( 'NONE',  ( 0.000000000000000000, 1.000000000000000000, 0.000000000000000000 ) ) ;
#31441 = CARTESIAN_POINT ( 'NONE',  ( -24.18731323226221974, 30.47097249907602290, 14.01125832528330406 ) ) ;
#31442 = CARTESIAN_POINT ( 'NONE',  ( -13.91746824999999532, 73.27500000273118985, -4.522059556121115875 ) ) ;
#31443 = DIRECTION ( 'NONE',  ( 0.000000000000000000, 0.000000000000000000, -1.000000000000000000 ) ) ;
#31444 = DIRECTION ( 'NONE',  ( -0.000000000000000000, -1.000000000000000000, -0.000000000000000000 ) ) ;
#31445 = CARTESIAN_POINT ( 'NONE',  ( -33.58253175000000113, 75.47500000273116427, 10.91162601494193929 ) ) ;
#31446 = ORIENTED_EDGE ( 'NONE', *, *, #18618, .F. ) ;
#31447 = CARTESIAN_POINT ( 'NONE',  ( -1.778240108872766143E-15, 20.00000000546237544, -32.49999999999999289 ) ) ;
#31448 = CARTESIAN_POINT ( 'NONE',  ( 2.584737979205441561E-13, 62.27343749999999289, 27.95245687107222921 ) ) ;
#31449 = CARTESIAN_POINT ( 'NONE',  ( 10.37757302488624767, 53.72500000273118559, 31.93888565452638417 ) ) ;
#31450 = CARTESIAN_POINT ( 'NONE',  ( -33.58253175000000113, 17.27500000273118630, -10.91162601494193218 ) ) ;
#31451 = CARTESIAN_POINT ( 'NONE',  ( -33.58253175000000113, 5.475000002731181148, 10.91162601494193929 ) ) ;
#31452 = CARTESIAN_POINT ( 'NONE',  ( -27.95245687107223276, 39.07031249999998579, 2.498001805406602216E-13 ) ) ;
#31453 = CARTESIAN_POINT ( 'NONE',  ( -7.543491769121417612, 26.04204833425729859, 28.00173670424549499 ) ) ;
#31454 = CARTESIAN_POINT ( 'NONE',  ( -0.04044903255044120238, 17.86680583240935860, -30.02300923189239867 ) ) ;
#31455 = CARTESIAN_POINT ( 'NONE',  ( -32.50000000000000000, 72.60000000546236265, 10.55989012756946366 ) ) ;
#31456 = CARTESIAN_POINT ( 'NONE',  ( 17.97732221215932569, 52.00000000000000711, -27.49025280458518239 ) ) ;
#31457 = AXIS2_PLACEMENT_3D ( 'NONE', #20912, #26393, #26053 ) ;
#31458 = CARTESIAN_POINT ( 'NONE',  ( -27.16883889988623935, 41.32500000273120122, 19.73931689729374739 ) ) ;
#31459 = CARTESIAN_POINT ( 'NONE',  ( 19.06425588902558133, 45.79649333240935505, -19.11951029504797006 ) ) ;
#31460 = CARTESIAN_POINT ( 'NONE',  ( 23.41746825000000243, 10.72499999726880127, -7.608796670333727974 ) ) ;
#31461 = CARTESIAN_POINT ( 'NONE',  ( 24.50000000000000000, 14.09999999999999076, -7.960532557706203605 ) ) ;
#31462 = ORIENTED_EDGE ( 'NONE', *, *, #17122, .F. ) ;
#31463 = ADVANCED_FACE ( 'NONE', ( #5077 ), #4730, .T. ) ;
#31464 = CARTESIAN_POINT ( 'NONE',  ( 10.37757302488624767, 55.97500000273118559, 31.93888565452638417 ) ) ;
#31465 = CARTESIAN_POINT ( 'NONE',  ( -8.891200544363830713E-16, 77.49999999999998579, -15.00000000000000000 ) ) ;
#31466 = CARTESIAN_POINT ( 'NONE',  ( -6.950374756619716266, 37.78684000092396644, -26.09010956794232428 ) ) ;
#31467 = CARTESIAN_POINT ( 'NONE',  ( -33.58253175000000113, 75.37500000273116996, 0.000000000000000000 ) ) ;
#31468 = EDGE_CURVE ( 'NONE', #9001, #32300, #28920, .T. ) ;
#31469 = VERTEX_POINT ( 'NONE', #15900 ) ;
#31470 = CARTESIAN_POINT ( 'NONE',  ( 10.37757302488624767, 21.72500000273118559, 31.93888565452638417 ) ) ;
#31471 = CARTESIAN_POINT ( 'NONE',  ( 2.740863092043355209E-13, 17.58593749999999645, 30.02300923189239512 ) ) ;
#31472 = VERTEX_POINT ( 'NONE', #25674 ) ;
#31473 = CARTESIAN_POINT ( 'NONE',  ( -32.50000000000000000, 57.89999999999999858, -10.55989012756945300 ) ) ;
#31474 = CARTESIAN_POINT ( 'NONE',  ( 27.16883889988623935, 58.32500000273119412, -19.73931689729374384 ) ) ;
#31475 = CARTESIAN_POINT ( 'NONE',  ( 28.01184896238304134, 44.36979166666666430, 7.505752307972846538 ) ) ;
#31476 = CARTESIAN_POINT ( 'NONE',  ( 0.000000000000000000, 74.00000000000001421, 0.000000000000000000 ) ) ;
#31477 = CARTESIAN_POINT ( 'NONE',  ( -7.236395654485763274, 6.524999997268826846, 22.27133577429736633 ) ) ;
#31478 = STYLED_ITEM ( 'NONE', ( #11632 ), #29162 ) ;
#31479 = CARTESIAN_POINT ( 'NONE',  ( -10.37757302488624411, 4.725000002731183812, -31.93888565452638417 ) ) ;
#31480 = CARTESIAN_POINT ( 'NONE',  ( -10.04305231718579172, 63.60000000000000142, -30.90933677959248982 ) ) ;
#31481 = CARTESIAN_POINT ( 'NONE',  ( -28.00173670424535644, 64.98920166574268364, 7.543491769121936308 ) ) ;
#31482 = CARTESIAN_POINT ( 'NONE',  ( -4.635254915624211769, 79.85000000546239107, -14.26584774442730286 ) ) ;
#31483 = CARTESIAN_POINT ( 'NONE',  ( 10.04305231718578817, 65.90000000546237402, -30.90933677959249337 ) ) ;
#31484 = CARTESIAN_POINT ( 'NONE',  ( 32.50000000000000711, 8.900000000000011013, 10.55989012756945122 ) ) ;
#31485 = CARTESIAN_POINT ( 'NONE',  ( -32.50000000000000000, 13.99999999999999822, 0.000000000000000000 ) ) ;
#31486 = CARTESIAN_POINT ( 'NONE',  ( 19.09188309203694800, 65.28125000000000000, 19.09188309203660694 ) ) ;
#31487 = CARTESIAN_POINT ( 'NONE',  ( -7.570916362186210335, 18.34999999453762598, -23.30088464923126779 ) ) ;
#31488 = CARTESIAN_POINT ( 'NONE',  ( -13.91746824999999532, 80.77500000273118985, -4.522059556121115875 ) ) ;
#31489 = CARTESIAN_POINT ( 'NONE',  ( -6.988114217767819270, 28.04166666666666075, 26.07999730980490583 ) ) ;
#31490 = CARTESIAN_POINT ( 'NONE',  ( 27.16883889988623935, 26.32500000273119056, -19.73931689729374384 ) ) ;
#31491 = CARTESIAN_POINT ( 'NONE',  ( 33.58253175000000823, 70.02500000273121827, 10.91162601494192863 ) ) ;
#31492 = CARTESIAN_POINT ( 'NONE',  ( -33.58253175000000113, 39.27500000273118275, -10.91162601494193218 ) ) ;
#31493 = CARTESIAN_POINT ( 'NONE',  ( -2.162160676586882350E-15, 14.87500000273120371, -35.31076352940722529 ) ) ;
#31494 = CARTESIAN_POINT ( 'NONE',  ( -24.50000000000000000, 7.000000000000006217, -3.000384657911015469E-15 ) ) ;
#31495 = CARTESIAN_POINT ( 'NONE',  ( -26.06988505166735237, 57.83892333425730214, -7.025853678916388567 ) ) ;
#31496 = CARTESIAN_POINT ( 'NONE',  ( 27.16883889988623935, 78.32500000273118701, -19.73931689729374384 ) ) ;
#31497 = CARTESIAN_POINT ( 'NONE',  ( -32.50000000000000000, 66.00000000000000000, 0.000000000000000000 ) ) ;
#31498 = CARTESIAN_POINT ( 'NONE',  ( 10.04305231718579705, 54.59999999999999432, 30.90933677959248982 ) ) ;
#31499 = CARTESIAN_POINT ( 'NONE',  ( 1.507698388325705758E-15, 15.12499999726880873, -24.62258325217400312 ) ) ;
#31500 = CARTESIAN_POINT ( 'NONE',  ( 33.58253175000000113, 56.12500000273118417, -4.112674001490185761E-15 ) ) ;
#31501 = CARTESIAN_POINT ( 'NONE',  ( -7.236395654485763274, 8.524999997268828622, 22.27133577429736633 ) ) ;
#31502 = EDGE_CURVE ( 'NONE', #22348, #15702, #23450, .T. ) ;
#31503 = VERTEX_POINT ( 'NONE', #23098 ) ;
#31504 = CARTESIAN_POINT ( 'NONE',  ( 6.486482029760649416E-15, 71.87500000273116996, 35.31076352940723240 ) ) ;
#31505 = CARTESIAN_POINT ( 'NONE',  ( -2.162160676586882350E-15, 4.625000002731207260, -35.31076352940722529 ) ) ;
#31506 = CARTESIAN_POINT ( 'NONE',  ( -4.523095164977116484E-15, 18.62499999726881583, 24.62258325217400312 ) ) ;
#31507 = CARTESIAN_POINT ( 'NONE',  ( -19.11951029504763611, 12.57850666759064140, 19.06425588902592239 ) ) ;
#31508 = ORIENTED_EDGE ( 'NONE', *, *, #3277, .F. ) ;
#31509 = CARTESIAN_POINT ( 'NONE',  ( 6.486482029760649416E-15, 41.62500000273116996, 35.31076352940723240 ) ) ;
#31510 = ORIENTED_EDGE ( 'NONE', *, *, #9342, .T. ) ;
#31511 = CARTESIAN_POINT ( 'NONE',  ( -26.00068869287340334, 42.22135416666666430, 15.01150461594643382 ) ) ;
#31512 = CARTESIAN_POINT ( 'NONE',  ( 32.50000000000000000, 5.000000000000004441, -3.980102097228898626E-15 ) ) ;
#31513 = CARTESIAN_POINT ( 'NONE',  ( -32.50000000000000000, 6.500000005462372776, 0.000000000000000000 ) ) ;
#31514 = CARTESIAN_POINT ( 'NONE',  ( 3.980102097228898626E-15, 52.00000000000000711, -32.50000000000000000 ) ) ;
#31515 = CARTESIAN_POINT ( 'NONE',  ( 28.01184896238304134, 20.30729166666666430, 7.505752307972846538 ) ) ;
#31516 = CARTESIAN_POINT ( 'NONE',  ( -23.41746825000000598, 15.72499999726882081, 7.608796670333726198 ) ) ;
#31517 = CARTESIAN_POINT ( 'NONE',  ( -27.16883889988624290, 15.17500000273119909, -19.73931689729374028 ) ) ;
#31518 = CARTESIAN_POINT ( 'NONE',  ( 32.50000000000000000, 61.00000000000000000, -3.980102097228898626E-15 ) ) ;
#31519 = CARTESIAN_POINT ( 'NONE',  ( -13.91746824999999532, 78.97500000273117848, 4.522059556121122093 ) ) ;
#31520 = CARTESIAN_POINT ( 'NONE',  ( 2.489536152421872915E-14, 74.00000000546238255, -32.49999999999999289 ) ) ;
#31521 = CARTESIAN_POINT ( 'NONE',  ( -7.468012846824272799, 30.04128499907601224, 28.02196122052058413 ) ) ;
#31522 = CARTESIAN_POINT ( 'NONE',  ( -13.91746824999999887, 77.37500000273116996, 0.000000000000000000 ) ) ;
#31523 = CARTESIAN_POINT ( 'NONE',  ( -15.01150461594642316, 43.08072916666666430, -26.00068869287341045 ) ) ;
#31524 = DIRECTION ( 'NONE',  ( -1.224646799147353454E-16, 1.000000000000000000, -0.000000000000000000 ) ) ;
#31525 = CARTESIAN_POINT ( 'NONE',  ( -19.82091636218621389, 13.19999999999998863, 14.40073868116558842 ) ) ;
#31526 = CARTESIAN_POINT ( 'NONE',  ( -10.04305231718579172, 3.599999999999992095, -30.90933677959248982 ) ) ;
#31527 = CARTESIAN_POINT ( 'NONE',  ( 26.29305231718579350, 17.30000000546239036, 19.10302069950537529 ) ) ;
#31528 = CARTESIAN_POINT ( 'NONE',  ( -19.11951029504797006, 65.56211833240934084, -19.06425588902558133 ) ) ;
#31529 = SHAPE_REPRESENTATION ( 'lock nut', ( #1376 ), #10174 ) ;
#31530 = CARTESIAN_POINT ( 'NONE',  ( -20.75514604977248823, 50.82500000273116569, -28.56700777964554305 ) ) ;
#31531 = CARTESIAN_POINT ( 'NONE',  ( 8.601468415847520532, 79.57500000273117280, 11.83890561707634781 ) ) ;
#31532 = CARTESIAN_POINT ( 'NONE',  ( -20.75514604977248823, 57.07500000273117280, -28.56700777964554305 ) ) ;
#31533 = CARTESIAN_POINT ( 'NONE',  ( 33.58253175000000823, 32.27500000273117564, 10.91162601494192685 ) ) ;
#31534 = CARTESIAN_POINT ( 'NONE',  ( 32.50000000000000711, 24.89999999999999858, 10.55989012756945122 ) ) ;
#31535 = CARTESIAN_POINT ( 'NONE',  ( 24.20753774853756113, 17.01302083333332504, 13.97622843553589789 ) ) ;
#31536 = CARTESIAN_POINT ( 'NONE',  ( -1.778240108872766143E-15, 16.00000000546237899, -32.49999999999999289 ) ) ;
#31537 = CARTESIAN_POINT ( 'NONE',  ( 32.50000000000000711, 74.90000000000000568, 10.55989012756945122 ) ) ;
#31538 = CARTESIAN_POINT ( 'NONE',  ( -27.16883889988623935, 15.32500000273116747, 19.73931689729374739 ) ) ;
#31539 = CARTESIAN_POINT ( 'NONE',  ( -19.82091636218621389, 12.94999999453763628, 14.40073868116558842 ) ) ;
#31540 = CARTESIAN_POINT ( 'NONE',  ( -6.950374756619247307, 16.29128499907601579, 26.09010956794245217 ) ) ;
#31541 = CARTESIAN_POINT ( 'NONE',  ( 32.50000000000000711, 35.40000000546237402, 10.55989012756945122 ) ) ;
#31542 = CARTESIAN_POINT ( 'NONE',  ( -20.75514604977248112, 23.42500000273119554, 28.56700777964554661 ) ) ;
#31543 = CARTESIAN_POINT ( 'NONE',  ( -13.97622843553588901, 41.93489583333333570, 24.20753774853756823 ) ) ;
#31544 = ORIENTED_EDGE ( 'NONE', *, *, #14595, .T. ) ;
#31545 = CARTESIAN_POINT ( 'NONE',  ( -33.58253175000000113, 61.22500000273118559, 10.91162601494193929 ) ) ;
#31546 = ORIENTED_EDGE ( 'NONE', *, *, #32629, .F. ) ;
#31547 = CARTESIAN_POINT ( 'NONE',  ( -30.02300923189239867, 64.57069416759065916, -0.04044903254991731589 ) ) ;
#31548 = CARTESIAN_POINT ( 'NONE',  ( 28.02196122052045268, 14.58371500092397710, -7.468012846824774620 ) ) ;
#31549 = CARTESIAN_POINT ( 'NONE',  ( -33.58253175000000113, 3.025000002731184967, -10.91162601494193218 ) ) ;
#31550 = CARTESIAN_POINT ( 'NONE',  ( 14.47279130897151589, 2.324999997268805796, 19.92008829642072953 ) ) ;
#31551 = CARTESIAN_POINT ( 'NONE',  ( -20.75514604977248823, 33.07500000273117990, -28.56700777964554305 ) ) ;
#31552 = CARTESIAN_POINT ( 'NONE',  ( -10.04305231718578462, 36.90000000546236691, 30.90933677959249337 ) ) ;
#31553 = AXIS2_PLACEMENT_3D ( 'NONE', #20265, #10135, #30538 ) ;
#31554 = CARTESIAN_POINT ( 'NONE',  ( -32.50000000000000000, 78.00000000000001421, 0.000000000000000000 ) ) ;
#31555 = CARTESIAN_POINT ( 'NONE',  ( -20.08610463437157989, 47.70000000000000284, -27.64615127144129758 ) ) ;
#31556 = CARTESIAN_POINT ( 'NONE',  ( 20.08610463437157279, 77.30000000000001137, -27.64615127144129758 ) ) ;
#31557 = CARTESIAN_POINT ( 'NONE',  ( 33.58253175000000823, 48.27500000273119696, 10.91162601494192863 ) ) ;
#31558 = CARTESIAN_POINT ( 'NONE',  ( 10.04305231718578817, 23.39999999999999147, -30.90933677959249337 ) ) ;
#31559 = CARTESIAN_POINT ( 'NONE',  ( 20.08610463437157279, 21.29999999999999716, -27.64615127144129758 ) ) ;
#31560 = CARTESIAN_POINT ( 'NONE',  ( -15.14183272437242600, 3.300000000000012257, 20.84094480462497856 ) ) ;
#31561 = CARTESIAN_POINT ( 'NONE',  ( -33.58253175000000113, 67.02500000273117564, -10.91162601494193218 ) ) ;
#31562 = CARTESIAN_POINT ( 'NONE',  ( -24.50000000000000355, 2.649999994537616477, -7.960532557706207157 ) ) ;
#31563 = CARTESIAN_POINT ( 'NONE',  ( -10.14794146028621924, 74.00000000000002842, -11.03244795973553849 ) ) ;
#31564 = CARTESIAN_POINT ( 'NONE',  ( -10.37757302488623701, 51.77500000273118985, 31.93888565452638417 ) ) ;
#31565 = CARTESIAN_POINT ( 'NONE',  ( -32.50000000000000000, 40.60000000546238397, 10.55989012756946366 ) ) ;
#31566 = CARTESIAN_POINT ( 'NONE',  ( 6.486482029760649416E-15, 11.62500000273118950, 35.31076352940723240 ) ) ;
#31567 = CARTESIAN_POINT ( 'NONE',  ( 13.94119854578937812, 32.48736083425731636, 24.22776226481240514 ) ) ;
#31568 = CARTESIAN_POINT ( 'NONE',  ( 3.778760231354629433E-15, 2.249999994537632553, -24.50000000000000355 ) ) ;
#31569 = DIRECTION ( 'NONE',  ( -1.000000000000000000, 0.000000000000000000, 0.000000000000000000 ) ) ;
#31570 = CARTESIAN_POINT ( 'NONE',  ( 20.75514604977248467, 32.42500000273116711, -28.56700777964554305 ) ) ;
#31571 = FACE_OUTER_BOUND ( 'NONE', #25775, .T. ) ;
#31572 = DIRECTION ( 'NONE',  ( -0.000000000000000000, 0.000000000000000000, -1.000000000000000000 ) ) ;
#31573 = CARTESIAN_POINT ( 'NONE',  ( -13.91746824999999887, 76.87500000273116996, 0.000000000000000000 ) ) ;
#31574 = CARTESIAN_POINT ( 'NONE',  ( 28.00173670424535644, 46.08295166574269075, -7.543491769121920321 ) ) ;
#31575 = CARTESIAN_POINT ( 'NONE',  ( 26.29305231718579350, 57.30000000546238681, 19.10302069950537529 ) ) ;
#31576 = CARTESIAN_POINT ( 'NONE',  ( 4.300734207923757602, 78.77500000273118985, -13.23629886949340673 ) ) ;
#31577 = CARTESIAN_POINT ( 'NONE',  ( 5.147494310547434893, 60.55125428154682510, 32.49999999999999289 ) ) ;
#31578 = CARTESIAN_POINT ( 'NONE',  ( 13.97622843553589966, 19.59114583333332149, -24.20753774853756113 ) ) ;
#31579 = CARTESIAN_POINT ( 'NONE',  ( -7.236395654485757944, 5.724999997268803931, -22.27133577429736988 ) ) ;
#31580 = CARTESIAN_POINT ( 'NONE',  ( -10.04305231718578462, 68.90000000546237402, 30.90933677959249337 ) ) ;
#31581 = CARTESIAN_POINT ( 'NONE',  ( -28.01184896238290278, 25.17708333333332860, 7.505752307973363457 ) ) ;
#31582 = CARTESIAN_POINT ( 'NONE',  ( -33.58253175000000113, 31.27500000273118275, -10.91162601494193218 ) ) ;
#31583 = CARTESIAN_POINT ( 'NONE',  ( 1.507698388325705758E-15, 15.62499999726882116, -24.62258325217400312 ) ) ;
#31584 = ORIENTED_EDGE ( 'NONE', *, *, #12725, .T. ) ;
#31585 = CARTESIAN_POINT ( 'NONE',  ( -25.98046417659859486, 44.23215250092398065, -15.04653450569291628 ) ) ;
#31586 = CARTESIAN_POINT ( 'NONE',  ( 10.04305231718579705, 17.10000000546236976, 30.90933677959248982 ) ) ;
#31587 = ADVANCED_FACE ( 'NONE', ( #7820, #18309 ), #5251, .F. ) ;
#31588 = CARTESIAN_POINT ( 'NONE',  ( -26.00068869287340334, 49.09635416666665719, 15.01150461594643382 ) ) ;
#31589 = CARTESIAN_POINT ( 'NONE',  ( 26.29305231718578995, 75.19999999999998863, -19.10302069950538240 ) ) ;
#31590 = CARTESIAN_POINT ( 'NONE',  ( -10.37757302488624411, 54.97500000273119980, -31.93888565452638417 ) ) ;
#31591 = CARTESIAN_POINT ( 'NONE',  ( -26.29305231718579350, 56.30000000546237260, -19.10302069950537884 ) ) ;
#31592 = CARTESIAN_POINT ( 'NONE',  ( -27.16883889988623935, 39.32500000273120122, 19.73931689729374739 ) ) ;
#31593 = CYLINDRICAL_SURFACE ( 'NONE', #4451, 32.50000000000000000 ) ;
#31594 = CARTESIAN_POINT ( 'NONE',  ( 20.75514604977248467, 68.67500000273119554, -28.56700777964554305 ) ) ;
#31595 = CARTESIAN_POINT ( 'NONE',  ( -10.04305231718578462, 0.9000000054623646939, 30.90933677959249337 ) ) ;
#31596 = EDGE_CURVE ( 'NONE', #871, #30951, #24123, .T. ) ;
#31597 = CARTESIAN_POINT ( 'NONE',  ( 33.58253175000000113, 60.22500000273119980, -10.91162601494193574 ) ) ;
#31598 = EDGE_CURVE ( 'NONE', #4188, #7938, #21218, .T. ) ;
#31599 = CARTESIAN_POINT ( 'NONE',  ( 2.740863092043355209E-13, 17.58593749999999645, 30.02300923189239867 ) ) ;
#31600 = CARTESIAN_POINT ( 'NONE',  ( -10.04305231718579172, 43.60000000000000142, -30.90933677959248982 ) ) ;
#31601 = CARTESIAN_POINT ( 'NONE',  ( 23.41746824999999887, 6.624999997268815832, 0.000000000000000000 ) ) ;
#31602 = CARTESIAN_POINT ( 'NONE',  ( 27.16883889988623935, 12.57500000273120655, -19.73931689729374384 ) ) ;
#31603 = DIRECTION ( 'NONE',  ( -0.000000000000000000, -1.000000000000000000, -0.000000000000000000 ) ) ;
#31604 = CARTESIAN_POINT ( 'NONE',  ( 6.950374756619257965, 35.19753499907601935, -26.09010956794244507 ) ) ;
#31605 = CARTESIAN_POINT ( 'NONE',  ( 0.000000000000000000, 82.00000000000001421, 0.000000000000000000 ) ) ;
#31606 = CARTESIAN_POINT ( 'NONE',  ( -33.58253175000000113, 77.37500000273116996, 0.000000000000000000 ) ) ;
#31607 = CARTESIAN_POINT ( 'NONE',  ( 3.980102097228898626E-15, 82.00000000000001421, 32.50000000000000000 ) ) ;
#31608 = CARTESIAN_POINT ( 'NONE',  ( -33.58253175000000113, 77.47500000273120691, 10.91162601494193929 ) ) ;
#31609 = ORIENTED_EDGE ( 'NONE', *, *, #5047, .T. ) ;
#31610 = VECTOR ( 'NONE', #6200, 1000.000000000000000 ) ;
#31611 = CYLINDRICAL_SURFACE ( 'NONE', #24454, 32.50000000000000000 ) ;
#31612 = CARTESIAN_POINT ( 'NONE',  ( -26.07999730980477437, 59.55208333333332149, 6.988114217768305103 ) ) ;
#31613 = CARTESIAN_POINT ( 'NONE',  ( -10.37757302488624411, 56.72500000273118559, -31.93888565452638417 ) ) ;
#31614 = CARTESIAN_POINT ( 'NONE',  ( 33.58253175000000113, 18.37500000273119127, -4.112674001490185761E-15 ) ) ;
#31615 = CARTESIAN_POINT ( 'NONE',  ( -20.75514604977248112, 1.675000002731184434, 28.56700777964554661 ) ) ;
#31616 = CARTESIAN_POINT ( 'NONE',  ( 27.95245687107223276, 44.22656249999999289, -2.463307335887066074E-13 ) ) ;
#31617 = CARTESIAN_POINT ( 'NONE',  ( -7.543491769121417612, 32.91704833425729504, 28.00173670424549499 ) ) ;
#31618 = CARTESIAN_POINT ( 'NONE',  ( -0.04044903255044120238, 21.30430583240935860, -30.02300923189239867 ) ) ;
#31619 = CARTESIAN_POINT ( 'NONE',  ( -26.29305231718578995, 70.70000000546238539, 19.10302069950538595 ) ) ;
#31620 = CARTESIAN_POINT ( 'NONE',  ( 5.779280353836490358E-15, 57.00000000546238965, 32.49999999999999289 ) ) ;
#31621 = CARTESIAN_POINT ( 'NONE',  ( 20.75514604977249178, 37.82500000273117280, 28.56700777964553950 ) ) ;
#31622 = CARTESIAN_POINT ( 'NONE',  ( -26.09010956794245217, 48.08815999907601935, -6.950374756619243755 ) ) ;
#31623 = CARTESIAN_POINT ( 'NONE',  ( 7.236395654485755280, 18.22499999726881370, 22.27133577429736988 ) ) ;
#31624 = CARTESIAN_POINT ( 'NONE',  ( 0.000000000000000000, 80.00000000000001421, 0.000000000000000000 ) ) ;
#31625 = ORIENTED_EDGE ( 'NONE', *, *, #5711, .F. ) ;
#31626 = CARTESIAN_POINT ( 'NONE',  ( 33.58253175000000823, 46.27500000273120406, 10.91162601494192863 ) ) ;
#31627 = DIRECTION ( 'NONE',  ( 0.8660254037844371533, -0.5000000000000026645, 0.000000000000000000 ) ) ;
#31628 = CARTESIAN_POINT ( 'NONE',  ( 27.95245687107223986, 55.97694416759064495, 0.04044903254993640479 ) ) ;
#31629 = CARTESIAN_POINT ( 'NONE',  ( 33.58253175000000113, 70.37500000273119838, -4.112674001490185761E-15 ) ) ;
#31630 = ORIENTED_EDGE ( 'NONE', *, *, #27039, .T. ) ;
#31631 = CARTESIAN_POINT ( 'NONE',  ( -10.37757302488623701, 25.52500000273118275, 31.93888565452638417 ) ) ;
#31632 = CARTESIAN_POINT ( 'NONE',  ( -20.50609665441004736, 22.31250000000000000, -20.50609665440969565 ) ) ;
#31633 = VERTEX_POINT ( 'NONE', #6082 ) ;
#31634 = CARTESIAN_POINT ( 'NONE',  ( 5.779280353836490358E-15, 49.00000000546238255, 32.49999999999999289 ) ) ;
#31635 = CARTESIAN_POINT ( 'NONE',  ( 10.37757302488624056, 60.52500000273119696, -31.93888565452638417 ) ) ;
#31636 = CARTESIAN_POINT ( 'NONE',  ( 28.01184896238304134, 47.80729166666666430, 7.505752307972846538 ) ) ;
#31637 = TOROIDAL_SURFACE ( 'NONE', #3165, 12.11000150615021553, 1.999999999999992228 ) ;
#31638 = CARTESIAN_POINT ( 'NONE',  ( -20.08610463437156923, 66.80000000546236549, 27.64615127144130113 ) ) ;
#31639 = CARTESIAN_POINT ( 'NONE',  ( -14.47279130897152299, 6.424999997268821872, 19.92008829642072243 ) ) ;
#31640 = CARTESIAN_POINT ( 'NONE',  ( -33.58253175000000113, 5.125000002731194826, 0.000000000000000000 ) ) ;
#31641 = CARTESIAN_POINT ( 'NONE',  ( 33.58253175000000113, 28.37500000273118772, -4.112674001490185761E-15 ) ) ;
#31642 = CARTESIAN_POINT ( 'NONE',  ( -4.223320258572821363E-15, 78.75000000546238255, 15.00000000000000355 ) ) ;
#31643 = CARTESIAN_POINT ( 'NONE',  ( 14.97647472619900455, 62.84076416574269786, -26.02091320914876960 ) ) ;
#31644 = CARTESIAN_POINT ( 'NONE',  ( -27.16883889988624290, 79.17500000273119554, -19.73931689729374028 ) ) ;
#31645 = CARTESIAN_POINT ( 'NONE',  ( 32.50000000000000000, 65.60000000546239107, -10.55989012756945833 ) ) ;
#31646 = CARTESIAN_POINT ( 'NONE',  ( -32.50000000000000000, 4.000000000000003553, 0.000000000000000000 ) ) ;
#31647 = CARTESIAN_POINT ( 'NONE',  ( -26.29305231718579350, 17.79999999999999716, -19.10302069950537884 ) ) ;
#31648 = CARTESIAN_POINT ( 'NONE',  ( -24.20753774853730889, 59.40885416666666430, 13.97622843553634020 ) ) ;
#31649 = CARTESIAN_POINT ( 'NONE',  ( 23.41746825000000243, 3.024999997268812635, 7.608796670333735079 ) ) ;
#31650 = CARTESIAN_POINT ( 'NONE',  ( -15.00000000000000000, 70.35000000546237686, 4.873795443493597723 ) ) ;
#31651 = CARTESIAN_POINT ( 'NONE',  ( 13.97622843553589966, 33.34114583333332860, -24.20753774853756113 ) ) ;
#31652 = EDGE_CURVE ( 'NONE', #10540, #22185, #27112, .T. ) ;
#31653 = CARTESIAN_POINT ( 'NONE',  ( -2.162160676586881955E-15, 22.62500000273119127, -35.31076352940723240 ) ) ;
#31654 = CARTESIAN_POINT ( 'NONE',  ( 33.58253175000000113, 72.22500000273119269, -10.91162601494193751 ) ) ;
#31655 = CARTESIAN_POINT ( 'NONE',  ( -33.58253175000000113, 35.37500000273117706, 0.000000000000000000 ) ) ;
#31656 = CARTESIAN_POINT ( 'NONE',  ( 20.75514604977249178, 18.07500000273119056, 28.56700777964553950 ) ) ;
#31657 = CARTESIAN_POINT ( 'NONE',  ( -19.82091636218621389, 7.200000000000011724, 14.40073868116558842 ) ) ;
#31658 = CARTESIAN_POINT ( 'NONE',  ( -26.06988505166735237, 61.27642333425730925, -7.025853678916388567 ) ) ;
#31659 = CARTESIAN_POINT ( 'NONE',  ( -2.162160676586882350E-15, 68.62500000273119838, -35.31076352940722529 ) ) ;
#31660 = CARTESIAN_POINT ( 'NONE',  ( 13.38432950954957690, -58.51673569255127205, 1.639107629260334588E-15 ) ) ;
#31661 = CARTESIAN_POINT ( 'NONE',  ( -20.08610463437156923, 54.30000000000000426, 27.64615127144130113 ) ) ;
#31662 = CARTESIAN_POINT ( 'NONE',  ( -15.00000000000000000, 72.35000000546236265, 4.873795443493597723 ) ) ;
#31663 = CARTESIAN_POINT ( 'NONE',  ( -20.75514604977248823, 60.82500000273120122, -28.56700777964554305 ) ) ;
#31664 = CARTESIAN_POINT ( 'NONE',  ( -4.523095164977116484E-15, 6.624999997268815832, 24.62258325217400312 ) ) ;
#31665 = VECTOR ( 'NONE', #26054, 1000.000000000000000 ) ;
#31666 = VERTEX_POINT ( 'NONE', #16402 ) ;
#31667 = CARTESIAN_POINT ( 'NONE',  ( -20.75514604977248823, 73.07500000273115859, -28.56700777964554305 ) ) ;
#31668 = CARTESIAN_POINT ( 'NONE',  ( 1.093617666956751375E-13, 61.50000000000000711, -32.50000000000000711 ) ) ;
#31669 = CARTESIAN_POINT ( 'NONE',  ( 1.507698388325705758E-15, 1.124999997268814722, -24.62258325217400312 ) ) ;
#31670 = CARTESIAN_POINT ( 'NONE',  ( 24.22776226481241224, 11.00298583425731103, -13.94119854578936923 ) ) ;
#31671 = ORIENTED_EDGE ( 'NONE', *, *, #6933, .T. ) ;
#31672 = CARTESIAN_POINT ( 'NONE',  ( 27.16883889988623935, 42.32500000273119412, -19.73931689729374384 ) ) ;
#31673 = LINE ( 'NONE', #24621, #15434 ) ;
#31674 = ORIENTED_EDGE ( 'NONE', *, *, #12497, .F. ) ;
#31675 = CARTESIAN_POINT ( 'NONE',  ( -28.01184896238304134, 39.21354166666666430, -7.505752307972844761 ) ) ;
#31676 = CARTESIAN_POINT ( 'NONE',  ( -2.162160676586882350E-15, 66.87500000273119838, -35.31076352940722529 ) ) ;
#31677 = CARTESIAN_POINT ( 'NONE',  ( 20.08610463437157279, 5.800000005462378816, -27.64615127144129758 ) ) ;
#31678 = CARTESIAN_POINT ( 'NONE',  ( 5.779280353836490358E-15, 27.00000000546237544, 32.49999999999999289 ) ) ;
#31679 = CARTESIAN_POINT ( 'NONE',  ( 2.740863092043355209E-13, 21.02343749999999645, 30.02300923189239512 ) ) ;
#31680 = CARTESIAN_POINT ( 'NONE',  ( 24.50000000000000355, 2.099999999999991651, -7.960532557706203605 ) ) ;
#31681 = CARTESIAN_POINT ( 'NONE',  ( 33.58253175000000823, 10.27500000273117564, 10.91162601494192863 ) ) ;
#31682 = CARTESIAN_POINT ( 'NONE',  ( -10.04305231718578462, 60.40000000000000568, 30.90933677959249337 ) ) ;
#31683 = CARTESIAN_POINT ( 'NONE',  ( -8.601468415847518756, 76.57500000273117280, -11.83890561707634603 ) ) ;
#31684 = CARTESIAN_POINT ( 'NONE',  ( 0.000000000000000000, 52.00000000000000711, 0.000000000000000000 ) ) ;
#31685 = CARTESIAN_POINT ( 'NONE',  ( 0.04044903255045854962, 33.33555583240935505, 30.02300923189239867 ) ) ;
#31686 = CARTESIAN_POINT ( 'NONE',  ( -13.91746824999999532, 75.27500000273121827, -4.522059556121115875 ) ) ;
#31687 = CARTESIAN_POINT ( 'NONE',  ( 2.740863092043355209E-13, 51.96093750000000000, 30.02300923189239867 ) ) ;
#31688 = ITEM_DEFINED_TRANSFORMATION ( 'NONE', 'NONE', #15623,  #1376 ) ;
#31689 = DIRECTION ( 'NONE',  ( 0.000000000000000000, 0.000000000000000000, -1.000000000000000000 ) ) ;
#31690 = CARTESIAN_POINT ( 'NONE',  ( 7.313012447739250820E-14, 15.50000000000000178, 24.50000000000000000 ) ) ;
#31691 = CARTESIAN_POINT ( 'NONE',  ( -10.04305231718578462, 4.400000000000014566, 30.90933677959249337 ) ) ;
#31692 = FACE_OUTER_BOUND ( 'NONE', #29669, .T. ) ;
#31693 = EDGE_CURVE ( 'NONE', #14415, #13367, #11159, .T. ) ;
#31694 = CARTESIAN_POINT ( 'NONE',  ( -24.18731323226221974, 64.84597249907602645, 14.01125832528330406 ) ) ;
#31695 = CARTESIAN_POINT ( 'NONE',  ( -33.58253175000000113, 41.02500000273118985, -10.91162601494193218 ) ) ;
#31696 = CARTESIAN_POINT ( 'NONE',  ( 12.13525491562420910, 71.45000000546237118, -8.816778784387098611 ) ) ;
#31697 = CARTESIAN_POINT ( 'NONE',  ( 20.75514604977248467, 54.67500000273119554, -28.56700777964554305 ) ) ;
#31698 = CARTESIAN_POINT ( 'NONE',  ( -10.37757302488623701, 33.77500000273120406, 31.93888565452638417 ) ) ;
#31699 = LINE ( 'NONE', #8192, #23485 ) ;
#31700 = EDGE_CURVE ( 'NONE', #6717, #13108, #13490, .T. ) ;
#31701 = CARTESIAN_POINT ( 'NONE',  ( -6.988114217768288228, 19.16145833333332860, -26.07999730980477437 ) ) ;
#31702 = CARTESIAN_POINT ( 'NONE',  ( 1.093617666956751375E-13, 61.50000000000000000, -32.50000000000000711 ) ) ;
#31703 = CARTESIAN_POINT ( 'NONE',  ( -5.147494310547423346, 22.94874572391553968, 32.50000000000000000 ) ) ;
#31704 = CARTESIAN_POINT ( 'NONE',  ( 32.50000000000000000, 73.00000000000000000, -3.980102097228898626E-15 ) ) ;
#31705 = CARTESIAN_POINT ( 'NONE',  ( 6.486482029760649416E-15, 13.62500000273118417, 35.31076352940723240 ) ) ;
#31706 = CARTESIAN_POINT ( 'NONE',  ( -23.41746824999999887, 7.624999997268816720, -2.867812753649727150E-15 ) ) ;
#31707 = CARTESIAN_POINT ( 'NONE',  ( -20.08610463437157989, 39.69999999999999574, -27.64615127144129758 ) ) ;
#31708 = CARTESIAN_POINT ( 'NONE',  ( -6.950374756619247307, 23.16628499907601579, 26.09010956794245217 ) ) ;
#31709 = CARTESIAN_POINT ( 'NONE',  ( -26.29305231718578995, 34.70000000546237828, 19.10302069950538595 ) ) ;
#31710 = CARTESIAN_POINT ( 'NONE',  ( 1.093617666956751375E-13, 61.50000000000000711, -32.50000000000000711 ) ) ;
#31711 = CARTESIAN_POINT ( 'NONE',  ( 6.486482029760648627E-15, 19.62500000273116996, 35.31076352940722529 ) ) ;
#31712 = CARTESIAN_POINT ( 'NONE',  ( 27.95245687107222921, 44.22656249999997868, -2.463307335887066074E-13 ) ) ;
#31713 = EDGE_LOOP ( 'NONE', ( #29757, #2298, #3482, #13234 ) ) ;
#31714 = CARTESIAN_POINT ( 'NONE',  ( 6.486482029760649416E-15, 65.62500000273116996, 35.31076352940723240 ) ) ;
#31715 = ORIENTED_EDGE ( 'NONE', *, *, #13138, .F. ) ;
#31716 = CARTESIAN_POINT ( 'NONE',  ( 26.00068869287340334, 13.00260416666666430, -15.01150461594642316 ) ) ;
#31717 = CARTESIAN_POINT ( 'NONE',  ( 28.02196122052045268, 18.02121500092397710, -7.468012846824774620 ) ) ;
#31718 = CARTESIAN_POINT ( 'NONE',  ( -20.75514604977248112, 5.425000002731182214, 28.56700777964554661 ) ) ;
#31719 = ORIENTED_EDGE ( 'NONE', *, *, #25524, .F. ) ;
#31720 = FACE_OUTER_BOUND ( 'NONE', #15571, .T. ) ;
#31721 = CARTESIAN_POINT ( 'NONE',  ( -20.75514604977248112, 27.67500000273118133, 28.56700777964554661 ) ) ;
#31722 = CARTESIAN_POINT ( 'NONE',  ( 32.50000000000000000, 39.60000000546234844, -10.55989012756945833 ) ) ;
#31723 =( BOUNDED_CURVE ( )  B_SPLINE_CURVE ( 2, ( #9977, #30904, #27189, #15133, #24611, #30082, #24775, #8993, #7398, #30251, #6754, #3681, #17234 ),
 .UNSPECIFIED., .F., .T. ) 
 B_SPLINE_CURVE_WITH_KNOTS ( ( 3, 2, 2, 2, 2, 2, 3 ),
 ( 0.2628205128205128305, 0.2641025641025641080, 0.2666666666666666630, 0.2692307692307692180, 0.2717948717948717730, 0.2743589743589743835, 0.2756410256410256610 ),
 .UNSPECIFIED. ) 
 CURVE ( )  GEOMETRIC_REPRESENTATION_ITEM ( )  RATIONAL_B_SPLINE_CURVE ( ( 0.9755282581475768211, 0.9755282581475768211, 1.000000000000000000, 0.9510565162951535312, 1.000000000000000000, 0.9510565162951535312, 1.000000000000000000, 0.9510565162951535312, 1.000000000000000000, 0.9510565162951535312, 1.000000000000000000, 0.9755282581475768211, 0.9755282581475768211 ) ) 
 REPRESENTATION_ITEM ( '' )  );
#31724 = CARTESIAN_POINT ( 'NONE',  ( -20.08610463437157989, 79.70000000000000284, -27.64615127144129758 ) ) ;
#31725 = CARTESIAN_POINT ( 'NONE',  ( -4.223320258572821363E-15, 78.75000000546236834, 15.00000000000000355 ) ) ;
#31726 = CARTESIAN_POINT ( 'NONE',  ( 6.486482029760649416E-15, 39.87500000273119127, 35.31076352940723240 ) ) ;
#31727 = CARTESIAN_POINT ( 'NONE',  ( 10.04305231718579705, 24.59999999999999787, 30.90933677959248982 ) ) ;
#31728 = CARTESIAN_POINT ( 'NONE',  ( 6.277390505771533514E-15, 22.49999999999998934, 34.17252228774368916 ) ) ;
#31729 = CARTESIAN_POINT ( 'NONE',  ( -15.14183272437242600, 7.300000000000001599, 20.84094480462497856 ) ) ;
#31730 = CARTESIAN_POINT ( 'NONE',  ( -33.58253175000000113, 65.12500000273119838, 0.000000000000000000 ) ) ;
#31731 = CARTESIAN_POINT ( 'NONE',  ( -26.85105675556549087, 66.99999999999997158, 19.27006841923039104 ) ) ;
#31732 = CARTESIAN_POINT ( 'NONE',  ( 9.930763101775172075, 74.00000000000000000, -10.06536667093442006 ) ) ;
#31733 = CARTESIAN_POINT ( 'NONE',  ( -33.58253175000000113, 53.27500000273118275, -10.91162601494193041 ) ) ;
#31734 = CARTESIAN_POINT ( 'NONE',  ( 23.41746824999999887, 4.624999997268814056, 0.000000000000000000 ) ) ;
#31735 = CARTESIAN_POINT ( 'NONE',  ( 3.880418787951132042, 4.198745712990783474, -24.50000000000000355 ) ) ;
#31736 = CARTESIAN_POINT ( 'NONE',  ( 33.58253175000000113, 12.12500000273120193, -4.112674001490185761E-15 ) ) ;
#31737 = CARTESIAN_POINT ( 'NONE',  ( -26.09010956794232428, 33.48996500092397355, 6.950374756619732253 ) ) ;
#31738 = CARTESIAN_POINT ( 'NONE',  ( 9.638965394428042899, 66.99999999999995737, -31.78062433674936571 ) ) ;
#31739 = CARTESIAN_POINT ( 'NONE',  ( -13.42768774669675125, 52.00000000000000000, 30.32522641246977457 ) ) ;
#31740 = CARTESIAN_POINT ( 'NONE',  ( 27.16883889988624290, 35.92500000273117422, 19.73931689729373673 ) ) ;
#31741 = CARTESIAN_POINT ( 'NONE',  ( -26.29305231718579350, 18.30000000546239036, -19.10302069950537884 ) ) ;
#31742 = DIRECTION ( 'NONE',  ( 0.000000000000000000, 0.000000000000000000, 1.000000000000000000 ) ) ;
#31743 = CARTESIAN_POINT ( 'NONE',  ( 13.91746824999999887, 75.87500000273116996, -1.704398294459741270E-15 ) ) ;
#31744 = CARTESIAN_POINT ( 'NONE',  ( 0.04044903255045854962, 43.64805583240936215, 30.02300923189239867 ) ) ;
#31745 = CARTESIAN_POINT ( 'NONE',  ( 32.50000000000000711, 51.40000000546238823, 10.55989012756945122 ) ) ;
#31746 = CARTESIAN_POINT ( 'NONE',  ( 2.688165632520823219E-15, 73.87500000273116996, 14.63369212191046387 ) ) ;
#31747 = CARTESIAN_POINT ( 'NONE',  ( -27.95245687107222921, 18.44531249999999645, 2.498001805406602216E-13 ) ) ;
#31748 = CARTESIAN_POINT ( 'NONE',  ( 26.29305231718578995, 69.70000000546238539, -19.10302069950538240 ) ) ;
#31749 = CARTESIAN_POINT ( 'NONE',  ( 20.50609665441005092, 17.15624999999999645, 20.50609665440969209 ) ) ;
#31750 = ADVANCED_FACE ( 'NONE', ( #24291 ), #425, .T. ) ;
#31751 = CARTESIAN_POINT ( 'NONE',  ( 20.75514604977249178, 30.07500000273118701, 28.56700777964553950 ) ) ;
#31752 = CARTESIAN_POINT ( 'NONE',  ( 23.41746824999999887, 13.12499999726882116, 0.000000000000000000 ) ) ;
#31753 = ORIENTED_EDGE ( 'NONE', *, *, #14029, .T. ) ;
#31754 = CARTESIAN_POINT ( 'NONE',  ( -15.04653450569291984, 39.93527750092397355, 25.98046417659859486 ) ) ;
#31755 = CARTESIAN_POINT ( 'NONE',  ( -10.04305231718579172, 14.10000000546239640, -30.90933677959248982 ) ) ;
#31756 = CARTESIAN_POINT ( 'NONE',  ( 28.01184896238304134, 54.68229166666665719, 7.505752307972846538 ) ) ;
#31757 = CARTESIAN_POINT ( 'NONE',  ( 5.147494310547440222, 75.44874571845313938, -32.50000000000000000 ) ) ;
#31758 = CARTESIAN_POINT ( 'NONE',  ( 10.37757302488624056, 48.77500000273118985, -31.93888565452638417 ) ) ;
#31759 = CARTESIAN_POINT ( 'NONE',  ( -10.04305231718578462, 54.90000000546238823, 30.90933677959249337 ) ) ;
#31760 = CARTESIAN_POINT ( 'NONE',  ( 11.25946833292375793, 76.17500000273119554, 8.180482586598731842 ) ) ;
#31761 = CARTESIAN_POINT ( 'NONE',  ( -33.58253175000000113, 37.22500000273119980, 10.91162601494193929 ) ) ;
#31762 = CARTESIAN_POINT ( 'NONE',  ( -33.58253175000000113, 63.47500000273117138, 10.91162601494193929 ) ) ;
#31763 = CARTESIAN_POINT ( 'NONE',  ( -2.092463501923844636E-15, 2.000000005462382102, -34.17252228774368916 ) ) ;
#31764 = CARTESIAN_POINT ( 'NONE',  ( 27.16883889988623935, 52.32500000273120122, -19.73931689729374384 ) ) ;
#31765 = CARTESIAN_POINT ( 'NONE',  ( 15.01150461594643382, 20.73697916666666075, 26.00068869287340334 ) ) ;
#31766 = CARTESIAN_POINT ( 'NONE',  ( 26.29305231718579350, 42.80000000000000426, 19.10302069950537529 ) ) ;
#31767 = CARTESIAN_POINT ( 'NONE',  ( -23.41746825000000598, 7.724999997268809260, 7.608796670333726198 ) ) ;
#31768 = CARTESIAN_POINT ( 'NONE',  ( -20.75514604977248823, 11.07500000273117813, -28.56700777964554305 ) ) ;
#31769 = DIRECTION ( 'NONE',  ( -0.000000000000000000, -1.000000000000000000, -0.000000000000000000 ) ) ;
#31770 = CARTESIAN_POINT ( 'NONE',  ( -0.04044903255042732459, 38.49180583240935505, -27.95245687107223986 ) ) ;
#31771 = DIRECTION ( 'NONE',  ( 1.000000000000000000, 0.000000000000000000, 0.000000000000000000 ) ) ;
#31772 = CARTESIAN_POINT ( 'NONE',  ( 10.37757302488624767, 69.97500000273119269, 31.93888565452638417 ) ) ;
#31773 = FACE_OUTER_BOUND ( 'NONE', #9200, .T. ) ;
#31774 = CARTESIAN_POINT ( 'NONE',  ( 33.58253175000000113, 66.37500000273121259, -4.112674001490185761E-15 ) ) ;
#31775 = ORIENTED_EDGE ( 'NONE', *, *, #22250, .T. ) ;
#31776 = LINE ( 'NONE', #18760, #11300 ) ;
#31777 = CARTESIAN_POINT ( 'NONE',  ( -24.20753774853756823, 59.98177083333332149, -13.97622843553588723 ) ) ;
#31778 = CARTESIAN_POINT ( 'NONE',  ( -27.16883889988624290, 56.92500000273119554, -19.73931689729374028 ) ) ;
#31779 = CARTESIAN_POINT ( 'NONE',  ( -10.37757302488623701, 7.775000002731194293, 31.93888565452638417 ) ) ;
#31780 = CARTESIAN_POINT ( 'NONE',  ( -33.58253175000000113, 1.475000002731190474, 10.91162601494193929 ) ) ;
#31781 = CARTESIAN_POINT ( 'NONE',  ( 13.97622843553589966, 43.65364583333332860, -24.20753774853756113 ) ) ;
#31782 = CARTESIAN_POINT ( 'NONE',  ( 30.02300923189239867, 31.91444416759064495, 0.04044903254992252006 ) ) ;
#31783 = ADVANCED_FACE ( 'NONE', ( #32330, #8822 ), #32165, .F. ) ;
#31784 = CARTESIAN_POINT ( 'NONE',  ( 20.47846945139867003, 21.73399333240935505, -20.53372385742107653 ) ) ;
#31785 = CARTESIAN_POINT ( 'NONE',  ( -32.50000000000000000, 76.40000000546235981, -10.55989012756945478 ) ) ;
#31786 = CARTESIAN_POINT ( 'NONE',  ( -32.50000000000000000, 56.50000000546237544, 0.000000000000000000 ) ) ;
#31787 = CARTESIAN_POINT ( 'NONE',  ( 27.16883889988623935, 36.32500000273120122, -19.73931689729374384 ) ) ;
#31788 = CARTESIAN_POINT ( 'NONE',  ( 13.94119854578893580, 42.21576416574269075, -24.22776226481265383 ) ) ;
#31789 = CARTESIAN_POINT ( 'NONE',  ( 23.41746825000000243, 14.72499999726881903, -7.608796670333727974 ) ) ;
#31790 = ADVANCED_FACE ( 'NONE', ( #19306 ), #21619, .T. ) ;
#31791 = CARTESIAN_POINT ( 'NONE',  ( -32.50000000000000000, 2.600000005462363095, 10.55989012756946366 ) ) ;
#31792 = VERTEX_POINT ( 'NONE', #29085 ) ;
#31793 = CARTESIAN_POINT ( 'NONE',  ( 20.75514604977248467, 46.67500000273118133, -28.56700777964554305 ) ) ;
#31794 = CARTESIAN_POINT ( 'NONE',  ( -1.778240108872766143E-15, 50.00000000546237544, -32.49999999999999289 ) ) ;
#31795 = CARTESIAN_POINT ( 'NONE',  ( -0.04044903254992426173, 49.96131916759065206, 27.95245687107223276 ) ) ;
#31796 = CARTESIAN_POINT ( 'NONE',  ( 33.58253175000000823, 66.27500000273118985, 10.91162601494192863 ) ) ;
#31797 = ORIENTED_EDGE ( 'NONE', *, *, #17545, .T. ) ;
#31798 = CARTESIAN_POINT ( 'NONE',  ( 27.16883889988623935, 20.32500000273117280, -19.73931689729374384 ) ) ;
#31799 = EDGE_CURVE ( 'NONE', #21272, #33751, #23422, .T. ) ;
#31800 = CARTESIAN_POINT ( 'NONE',  ( 7.505752307973351023, 20.88020833333333215, 28.01184896238290278 ) ) ;
#31801 = ORIENTED_EDGE ( 'NONE', *, *, #8939, .T. ) ;
#31802 = CYLINDRICAL_SURFACE ( 'NONE', #5644, 32.50000000000000000 ) ;
#31803 = CARTESIAN_POINT ( 'NONE',  ( 33.58253175000000823, 52.02500000273118985, 10.91162601494192863 ) ) ;
#31804 = CARTESIAN_POINT ( 'NONE',  ( 15.01150461594596308, 47.09114583333332860, -26.00068869287367335 ) ) ;
#31805 = CARTESIAN_POINT ( 'NONE',  ( 32.50000000000000711, 19.40000000546238468, 10.55989012756945122 ) ) ;
#31806 = CARTESIAN_POINT ( 'NONE',  ( -7.570916362186215665, 7.149999994537637349, 23.30088464923126423 ) ) ;
#31807 = CARTESIAN_POINT ( 'NONE',  ( -7.236395654485763274, 10.52499999726880198, 22.27133577429736633 ) ) ;
#31808 = CARTESIAN_POINT ( 'NONE',  ( -33.58253175000000113, 29.27500000273118630, -10.91162601494193218 ) ) ;
#31809 = CARTESIAN_POINT ( 'NONE',  ( -2.375766604868045029, 77.80125428700922896, -14.99999999999999822 ) ) ;
#31810 = CARTESIAN_POINT ( 'NONE',  ( -7.468012846824272799, 57.54128499907602645, 28.02196122052058413 ) ) ;
#31811 = CARTESIAN_POINT ( 'NONE',  ( 20.75514604977248467, 78.67500000273116711, -28.56700777964554305 ) ) ;
#31812 = CARTESIAN_POINT ( 'NONE',  ( 32.50000000000000711, 65.40000000546237402, 10.55989012756945122 ) ) ;
#31813 = CARTESIAN_POINT ( 'NONE',  ( -26.29305231718579350, 3.799999999999998046, -19.10302069950537884 ) ) ;
#31814 = CARTESIAN_POINT ( 'NONE',  ( -32.50000000000000000, 12.09999999999999787, 10.55989012756946366 ) ) ;
#31815 = CARTESIAN_POINT ( 'NONE',  ( -13.97622843553588901, 59.12239583333333570, 24.20753774853756823 ) ) ;
#31816 = CARTESIAN_POINT ( 'NONE',  ( 15.14183272437242245, 18.04999999453762172, -20.84094480462497856 ) ) ;
#31817 = CARTESIAN_POINT ( 'NONE',  ( -13.91746824999999532, 72.77500000273117564, -4.522059556121115875 ) ) ;
#31818 = CARTESIAN_POINT ( 'NONE',  ( -27.95245687107222921, 35.63281249999998579, 2.498001805406602216E-13 ) ) ;
#31819 =( BOUNDED_SURFACE ( )  B_SPLINE_SURFACE ( 1, 2, ( 
 ( #32971, #4501, #2271, #31098, #25446, #15498, #19957, #12399, #2098, #6903, #28186, #17384, #25618, #13426, #26797, #28862, #5192, #10346, #2785, #29362, #31935, #18247, #18417, #20822, #13251, #3127, #5359, #8428, #20988, #31438, #21159, #28694, #21326, #15676, #26124, #29026, #23389, #22, #8260, #16177, #13084, #18752, #3291, #23724, #26464, #26633, #15839, #13599, #31266, #23894, #33851, #26296, #2621, #7761, #191, #5863, #18917, #23558, #10678, #10510, #31601, #24065, #8099, #16341, #7930, #18586, #5529, #16009, #2956, #365, #10851, #31767, #29194, #5700, #531, #11018, #21488, #24716, #6693, #9099, #14095, #14428, #11183, #3621, #6533, #11843, #22322, #32268, #3453, #3788, #30028, #29683, #27635, #21654, #32767, #1193, #27296, #9261, #27463, #3953, #19080, #1366, #8761, #32099, #6023, #6188, #21985, #24389, #32599, #17006, #19580, #27127, #24883, #19745, #8596, #30191, #697, #24551, #863, #17177, #19244, #29520, #1023, #13756, #11505, #16501, #16670, #24227, #32433, #11674, #8931, #26954, #19412, #13925, #11344, #21820, #29861, #6361, #22157, #16840, #14258, #33458, #22653, #1536, #33286, #25742, #17863, #14765, #9783, #12012, #20263, #33105, #14937, #9610, #30708, #17515, #12532, #12357, #7032, #2224, #30363, #2056, #9429, #10133, #9957, #20091, #22481, #7203, #12701, #28314, #25230, #17687, #32930, #28147, #30536, #25402, #27976, #4633, #4461, #23001, #22826 ),
 ( #4123, #1704, #20433, #30883, #27806, #7379, #7552, #1880, #15112, #4802, #25576, #15282, #19914, #23172, #18036, #33634, #6864, #25055, #20615, #31059, #14598, #17343, #4290, #12183, #18376, #8220, #23516, #3088, #26085, #2581, #26255, #15633, #31227, #31560, #13560, #18543, #21117, #24022, #10305, #10469, #31397, #5488, #21449, #23856, #28821, #29150, #25911, #5319, #21289, #26592, #492, #13045, #18207, #28989, #10809, #20948, #8388, #2405, #10975, #15967, #8058, #31892, #18714, #5656, #33812, #16138, #33976, #12873, #20783, #7887, #2743, #5146, #13384, #31729, #322, #15799, #28482, #4978, #23350, #15456, #7720, #13207, #23683, #28650, #149, #10638, #26423, #2917, #6147, #5824, #826, #22118, #3582, #16801, #8723, #16302, #3415, #26759, #1324, #24845, #27425, #8890, #11471, #3916, #658, #11307, #21785, #29821, #11806, #14223, #19207, #19542, #3251, #29645, #11635, #16967, #14388, #13889, #8561, #19375, #1153, #32233, #32729, #13721, #22284, #6325, #32396, #18873, #32562, #9061, #24186, #6494, #24356, #11146, #21616, #16632, #27088, #29483, #3749, #29990, #24679, #14054, #29322, #32061, #19045, #5987, #16464, #24516, #26919, #986, #21945, #27258, #30493, #20392, #6994, #30152, #25187, #12491, #27937, #7162, #33065, #6656, #27765, #17139, #25703, #15241, #30844, #1497, #17645, #14556, #2184, #4593, #4251, #27592, #4421, #7335, #22960, #19872, #14896, #4083, #25360 ) ),
 .UNSPECIFIED., .F., .F., .T. ) 
 B_SPLINE_SURFACE_WITH_KNOTS ( ( 2, 2 ),
 ( 3, 2, 2, 2, 2, 2, 2, 2, 2, 2, 2, 2, 2, 2, 2, 2, 2, 2, 2, 2, 2, 2, 2, 2, 2, 2, 2, 2, 2, 2, 2, 2, 2, 2, 2, 2, 2, 2, 2, 2, 2, 2, 2, 2, 2, 2, 2, 2, 2, 2, 2, 2, 2, 2, 2, 2, 2, 2, 2, 2, 2, 2, 2, 2, 2, 2, 2, 2, 2, 2, 2, 2, 2, 2, 2, 2, 2, 2, 2, 2, 2, 2, 2, 2, 2, 2, 2, 2, 2, 2, 3 ),
 ( 0.000000000000000000, 1.000000000000000000 ),
 ( 0.000000000000000000, 0.01111111111111111154, 0.02222222222222222307, 0.03333333333333333287, 0.04444444444444444614, 0.05555555555555555247, 0.06666666666666666574, 0.07777777777777777901, 0.08888888888888889228, 0.1000000000000000056, 0.1111111111111111049, 0.1222222222222222182, 0.1333333333333333315, 0.1444444444444444309, 0.1555555555555555580, 0.1666666666666666574, 0.1777777777777777846, 0.1888888888888888840, 0.2000000000000000111, 0.2111111111111111105, 0.2222222222222222099, 0.2333333333333333370, 0.2444444444444444364, 0.2555555555555555358, 0.2666666666666666630, 0.2777777777777777901, 0.2888888888888888618, 0.2999999999999999889, 0.3111111111111111160, 0.3222222222222222432, 0.3333333333333333148, 0.3444444444444444420, 0.3555555555555555691, 0.3666666666666666408, 0.3777777777777777679, 0.3888888888888888951, 0.4000000000000000222, 0.4111111111111110938, 0.4222222222222222210, 0.4333333333333333481, 0.4444444444444444198, 0.4555555555555555469, 0.4666666666666666741, 0.4777777777777778012, 0.4888888888888888729, 0.5000000000000000000, 0.5111111111111110716, 0.5222222222222222543, 0.5333333333333333259, 0.5444444444444443976, 0.5555555555555555802, 0.5666666666666666519, 0.5777777777777777235, 0.5888888888888889062, 0.5999999999999999778, 0.6111111111111111605, 0.6222222222222222321, 0.6333333333333333037, 0.6444444444444444864, 0.6555555555555555580, 0.6666666666666666297, 0.6777777777777778123, 0.6888888888888888840, 0.6999999999999999556, 0.7111111111111111382, 0.7222222222222222099, 0.7333333333333332815, 0.7444444444444444642, 0.7555555555555555358, 0.7666666666666667185, 0.7777777777777777901, 0.7888888888888888618, 0.8000000000000000444, 0.8111111111111111160, 0.8222222222222221877, 0.8333333333333333703, 0.8444444444444444420, 0.8555555555555555136, 0.8666666666666666963, 0.8777777777777777679, 0.8888888888888888395, 0.9000000000000000222, 0.9111111111111110938, 0.9222222222222222765, 0.9333333333333333481, 0.9444444444444444198, 0.9555555555555556024, 0.9666666666666666741, 0.9777777777777777457, 0.9888888888888889284, 1.000000000000000000 ),
 .UNSPECIFIED. ) 
 GEOMETRIC_REPRESENTATION_ITEM ( )  RATIONAL_B_SPLINE_SURFACE ( (
 ( 1.000000000000000000, 0.9510565162951535312, 1.000000000000000000, 0.9510565162951535312, 1.000000000000000000, 0.9510565162951535312, 1.000000000000000000, 0.9510565162951535312, 1.000000000000000000, 0.9510565162951535312, 1.000000000000000000, 0.9510565162951535312, 1.000000000000000000, 0.9510565162951535312, 1.000000000000000000, 0.9510565162951535312, 1.000000000000000000, 0.9510565162951535312, 1.000000000000000000, 0.9510565162951535312, 1.000000000000000000, 0.9510565162951535312, 1.000000000000000000, 0.9510565162951535312, 1.000000000000000000, 0.9510565162951535312, 1.000000000000000000, 0.9510565162951535312, 1.000000000000000000, 0.9510565162951535312, 1.000000000000000000, 0.9510565162951535312, 1.000000000000000000, 0.9510565162951535312, 1.000000000000000000, 0.9510565162951535312, 1.000000000000000000, 0.9510565162951535312, 1.000000000000000000, 0.9510565162951535312, 1.000000000000000000, 0.9510565162951535312, 1.000000000000000000, 0.9510565162951535312, 1.000000000000000000, 0.9510565162951535312, 1.000000000000000000, 0.9510565162951535312, 1.000000000000000000, 0.9510565162951535312, 1.000000000000000000, 0.9510565162951535312, 1.000000000000000000, 0.9510565162951535312, 1.000000000000000000, 0.9510565162951535312, 1.000000000000000000, 0.9510565162951535312, 1.000000000000000000, 0.9510565162951535312, 1.000000000000000000, 0.9510565162951535312, 1.000000000000000000, 0.9510565162951535312, 1.000000000000000000, 0.9510565162951535312, 1.000000000000000000, 0.9510565162951535312, 1.000000000000000000, 0.9510565162951535312, 1.000000000000000000, 0.9510565162951535312, 1.000000000000000000, 0.9510565162951535312, 1.000000000000000000, 0.9510565162951535312, 1.000000000000000000, 0.9510565162951535312, 1.000000000000000000, 0.9510565162951535312, 1.000000000000000000, 0.9510565162951535312, 1.000000000000000000, 0.9510565162951535312, 1.000000000000000000, 0.9510565162951535312, 1.000000000000000000, 0.9510565162951535312, 1.000000000000000000, 0.9510565162951535312, 1.000000000000000000, 0.9510565162951535312, 1.000000000000000000, 0.9510565162951535312, 1.000000000000000000, 0.9510565162951535312, 1.000000000000000000, 0.9510565162951535312, 1.000000000000000000, 0.9510565162951535312, 1.000000000000000000, 0.9510565162951535312, 1.000000000000000000, 0.9510565162951535312, 1.000000000000000000, 0.9510565162951535312, 1.000000000000000000, 0.9510565162951535312, 1.000000000000000000, 0.9510565162951535312, 1.000000000000000000, 0.9510565162951535312, 1.000000000000000000, 0.9510565162951535312, 1.000000000000000000, 0.9510565162951535312, 1.000000000000000000, 0.9510565162951535312, 1.000000000000000000, 0.9510565162951535312, 1.000000000000000000, 0.9510565162951535312, 1.000000000000000000, 0.9510565162951535312, 1.000000000000000000, 0.9510565162951535312, 1.000000000000000000, 0.9510565162951535312, 1.000000000000000000, 0.9510565162951535312, 1.000000000000000000, 0.9510565162951535312, 1.000000000000000000, 0.9510565162951535312, 1.000000000000000000, 0.9510565162951535312, 1.000000000000000000, 0.9510565162951535312, 1.000000000000000000, 0.9510565162951535312, 1.000000000000000000, 0.9510565162951535312, 1.000000000000000000, 0.9510565162951535312, 1.000000000000000000, 0.9510565162951535312, 1.000000000000000000, 0.9510565162951535312, 1.000000000000000000, 0.9510565162951535312, 1.000000000000000000, 0.9510565162951535312, 1.000000000000000000, 0.9510565162951535312, 1.000000000000000000, 0.9510565162951535312, 1.000000000000000000, 0.9510565162951535312, 1.000000000000000000, 0.9510565162951535312, 1.000000000000000000, 0.9510565162951535312, 1.000000000000000000, 0.9510565162951535312, 1.000000000000000000, 0.9510565162951535312, 1.000000000000000000, 0.9510565162951535312, 1.000000000000000000, 0.9510565162951535312, 1.000000000000000000, 0.9510565162951535312, 1.000000000000000000, 0.9510565162951535312, 1.000000000000000000, 0.9510565162951535312, 1.000000000000000000, 0.9510565162951535312, 1.000000000000000000, 0.9510565162951535312, 1.000000000000000000),
 ( 1.000000000000000000, 0.9510565162951535312, 1.000000000000000000, 0.9510565162951535312, 1.000000000000000000, 0.9510565162951535312, 1.000000000000000000, 0.9510565162951535312, 1.000000000000000000, 0.9510565162951535312, 1.000000000000000000, 0.9510565162951535312, 1.000000000000000000, 0.9510565162951535312, 1.000000000000000000, 0.9510565162951535312, 1.000000000000000000, 0.9510565162951535312, 1.000000000000000000, 0.9510565162951535312, 1.000000000000000000, 0.9510565162951535312, 1.000000000000000000, 0.9510565162951535312, 1.000000000000000000, 0.9510565162951535312, 1.000000000000000000, 0.9510565162951535312, 1.000000000000000000, 0.9510565162951535312, 1.000000000000000000, 0.9510565162951535312, 1.000000000000000000, 0.9510565162951535312, 1.000000000000000000, 0.9510565162951535312, 1.000000000000000000, 0.9510565162951535312, 1.000000000000000000, 0.9510565162951535312, 1.000000000000000000, 0.9510565162951535312, 1.000000000000000000, 0.9510565162951535312, 1.000000000000000000, 0.9510565162951535312, 1.000000000000000000, 0.9510565162951535312, 1.000000000000000000, 0.9510565162951535312, 1.000000000000000000, 0.9510565162951535312, 1.000000000000000000, 0.9510565162951535312, 1.000000000000000000, 0.9510565162951535312, 1.000000000000000000, 0.9510565162951535312, 1.000000000000000000, 0.9510565162951535312, 1.000000000000000000, 0.9510565162951535312, 1.000000000000000000, 0.9510565162951535312, 1.000000000000000000, 0.9510565162951535312, 1.000000000000000000, 0.9510565162951535312, 1.000000000000000000, 0.9510565162951535312, 1.000000000000000000, 0.9510565162951535312, 1.000000000000000000, 0.9510565162951535312, 1.000000000000000000, 0.9510565162951535312, 1.000000000000000000, 0.9510565162951535312, 1.000000000000000000, 0.9510565162951535312, 1.000000000000000000, 0.9510565162951535312, 1.000000000000000000, 0.9510565162951535312, 1.000000000000000000, 0.9510565162951535312, 1.000000000000000000, 0.9510565162951535312, 1.000000000000000000, 0.9510565162951535312, 1.000000000000000000, 0.9510565162951535312, 1.000000000000000000, 0.9510565162951535312, 1.000000000000000000, 0.9510565162951535312, 1.000000000000000000, 0.9510565162951535312, 1.000000000000000000, 0.9510565162951535312, 1.000000000000000000, 0.9510565162951535312, 1.000000000000000000, 0.9510565162951535312, 1.000000000000000000, 0.9510565162951535312, 1.000000000000000000, 0.9510565162951535312, 1.000000000000000000, 0.9510565162951535312, 1.000000000000000000, 0.9510565162951535312, 1.000000000000000000, 0.9510565162951535312, 1.000000000000000000, 0.9510565162951535312, 1.000000000000000000, 0.9510565162951535312, 1.000000000000000000, 0.9510565162951535312, 1.000000000000000000, 0.9510565162951535312, 1.000000000000000000, 0.9510565162951535312, 1.000000000000000000, 0.9510565162951535312, 1.000000000000000000, 0.9510565162951535312, 1.000000000000000000, 0.9510565162951535312, 1.000000000000000000, 0.9510565162951535312, 1.000000000000000000, 0.9510565162951535312, 1.000000000000000000, 0.9510565162951535312, 1.000000000000000000, 0.9510565162951535312, 1.000000000000000000, 0.9510565162951535312, 1.000000000000000000, 0.9510565162951535312, 1.000000000000000000, 0.9510565162951535312, 1.000000000000000000, 0.9510565162951535312, 1.000000000000000000, 0.9510565162951535312, 1.000000000000000000, 0.9510565162951535312, 1.000000000000000000, 0.9510565162951535312, 1.000000000000000000, 0.9510565162951535312, 1.000000000000000000, 0.9510565162951535312, 1.000000000000000000, 0.9510565162951535312, 1.000000000000000000, 0.9510565162951535312, 1.000000000000000000, 0.9510565162951535312, 1.000000000000000000, 0.9510565162951535312, 1.000000000000000000, 0.9510565162951535312, 1.000000000000000000, 0.9510565162951535312, 1.000000000000000000, 0.9510565162951535312, 1.000000000000000000, 0.9510565162951535312, 1.000000000000000000, 0.9510565162951535312, 1.000000000000000000, 0.9510565162951535312, 1.000000000000000000, 0.9510565162951535312, 1.000000000000000000, 0.9510565162951535312, 1.000000000000000000) ) ) 
 REPRESENTATION_ITEM ( '' )  SURFACE ( )  );
#31820 = CARTESIAN_POINT ( 'NONE',  ( 33.58253175000000113, 26.22500000273119625, -10.91162601494193751 ) ) ;
#31821 = CARTESIAN_POINT ( 'NONE',  ( -27.16883889988624290, 72.92500000273120975, -19.73931689729374028 ) ) ;
#31822 = CARTESIAN_POINT ( 'NONE',  ( -27.16883889988623935, 35.57500000273118701, 19.73931689729374739 ) ) ;
#31823 = CARTESIAN_POINT ( 'NONE',  ( 33.58253175000000823, 16.27500000273118985, 10.91162601494192685 ) ) ;
#31824 = CARTESIAN_POINT ( 'NONE',  ( -6.950374756619716266, 54.97434000092398065, -26.09010956794232428 ) ) ;
#31825 = CARTESIAN_POINT ( 'NONE',  ( -20.75514604977248823, 70.82500000273117280, -28.56700777964554305 ) ) ;
#31826 = CARTESIAN_POINT ( 'NONE',  ( 32.50000000000000711, 3.400000005462366914, 10.55989012756945122 ) ) ;
#31827 = CARTESIAN_POINT ( 'NONE',  ( 32.50000000000000000, 51.09999999999998721, -10.55989012756945833 ) ) ;
#31828 = CARTESIAN_POINT ( 'NONE',  ( -4.223320258572821363E-15, 78.75000000546238255, 15.00000000000000355 ) ) ;
#31829 = CARTESIAN_POINT ( 'NONE',  ( -27.16883889988624290, 60.92500000273118133, -19.73931689729374028 ) ) ;
#31830 = CARTESIAN_POINT ( 'NONE',  ( -7.236395654485757944, 17.72499999726881370, -22.27133577429736988 ) ) ;
#31831 = EDGE_LOOP ( 'NONE', ( #17028, #24907, #22544, #32993 ) ) ;
#31832 = CARTESIAN_POINT ( 'NONE',  ( -20.75514604977248112, 69.67500000273119554, 28.56700777964554661 ) ) ;
#31833 = CARTESIAN_POINT ( 'NONE',  ( 10.37757302488624767, 1.725000002731180704, 31.93888565452638417 ) ) ;
#31834 = CARTESIAN_POINT ( 'NONE',  ( 23.41746825000000243, 8.524999997268812635, 7.608796670333735079 ) ) ;
#31835 = CARTESIAN_POINT ( 'NONE',  ( 24.22776226481241224, 24.75298583425730925, -13.94119854578936923 ) ) ;
#31836 = ORIENTED_EDGE ( 'NONE', *, *, #21746, .T. ) ;
#31837 = CARTESIAN_POINT ( 'NONE',  ( -20.75514604977248823, 36.82500000273117990, -28.56700777964554305 ) ) ;
#31838 = LINE ( 'NONE', #32005, #3375 ) ;
#31839 = AXIS2_PLACEMENT_3D ( 'NONE', #10444, #23661, #26060 ) ;
#31840 = ORIENTED_EDGE ( 'NONE', *, *, #26437, .F. ) ;
#31841 = CARTESIAN_POINT ( 'NONE',  ( 28.01184896238290278, 40.64583333333332860, -7.505752307973347470 ) ) ;
#31842 = CARTESIAN_POINT ( 'NONE',  ( -32.50000000000000000, 60.40000000546236691, -10.55989012756945300 ) ) ;
#31843 = CARTESIAN_POINT ( 'NONE',  ( -32.50000000000000000, 0.5000000054623809920, 0.000000000000000000 ) ) ;
#31844 = CARTESIAN_POINT ( 'NONE',  ( -5.147494310547450880, 72.44874571845318201, 32.49999999999999289 ) ) ;
#31845 = CARTESIAN_POINT ( 'NONE',  ( -28.01184896238290278, 21.73958333333332860, 7.505752307973363457 ) ) ;
#31846 = CARTESIAN_POINT ( 'NONE',  ( 19.82091636218621034, 1.799999999999996048, 14.40073868116559730 ) ) ;
#31847 = CARTESIAN_POINT ( 'NONE',  ( -10.37757302488623701, 7.775000002731180970, 31.93888565452638417 ) ) ;
#31848 = CARTESIAN_POINT ( 'NONE',  ( -10.04305231718579172, 61.59999999999998721, -30.90933677959248982 ) ) ;
#31849 = CARTESIAN_POINT ( 'NONE',  ( 4.300734207923757602, 76.27500000273118985, -13.23629886949340673 ) ) ;
#31850 = LINE ( 'NONE', #8343, #12677 ) ;
#31851 = CARTESIAN_POINT ( 'NONE',  ( 7.468012846824281681, 31.76003499907602290, -28.02196122052058058 ) ) ;
#31852 = VECTOR ( 'NONE', #2911, 1000.000000000000000 ) ;
#31853 = CARTESIAN_POINT ( 'NONE',  ( 8.601468415847516980, 74.67500000273118133, -11.83890561707634781 ) ) ;
#31854 = CARTESIAN_POINT ( 'NONE',  ( 26.00068869287341045, 47.37760416666666430, -15.01150461594642493 ) ) ;
#31855 = DIRECTION ( 'NONE',  ( 0.000000000000000000, 0.000000000000000000, -1.000000000000000000 ) ) ;
#31856 = CARTESIAN_POINT ( 'NONE',  ( 10.04305231718579705, 49.10000000546238397, 30.90933677959248982 ) ) ;
#31857 = CARTESIAN_POINT ( 'NONE',  ( 27.95245687107223276, 59.97618083240934794, -0.04044903255042905932 ) ) ;
#31858 = CARTESIAN_POINT ( 'NONE',  ( -33.58253175000000113, 41.22500000273118559, 10.91162601494193929 ) ) ;
#31859 = CARTESIAN_POINT ( 'NONE',  ( 9.270509831248425314, 70.95000000546237118, 12.75976212528059683 ) ) ;
#31860 = CARTESIAN_POINT ( 'NONE',  ( 10.37757302488624056, 54.77500000273121117, -31.93888565452638417 ) ) ;
#31861 = CARTESIAN_POINT ( 'NONE',  ( -33.58253175000000113, 35.27500000273119696, -10.91162601494193041 ) ) ;
#31862 = DIRECTION ( 'NONE',  ( 0.000000000000000000, 1.000000000000000000, 0.000000000000000000 ) ) ;
#31863 = CARTESIAN_POINT ( 'NONE',  ( 24.20753774853756113, 23.88802083333332504, 13.97622843553589789 ) ) ;
#31864 = CARTESIAN_POINT ( 'NONE',  ( -12.13525491562421088, 80.05000000546236549, -8.816778784387096835 ) ) ;
#31865 = CARTESIAN_POINT ( 'NONE',  ( -2.375766604868044585, 80.44874571845313938, 14.99999999999999822 ) ) ;
#31866 = CARTESIAN_POINT ( 'NONE',  ( -20.08610463437156923, 72.30000000000002558, 27.64615127144130113 ) ) ;
#31867 = CARTESIAN_POINT ( 'NONE',  ( 33.58253175000000823, 8.025000002731188076, 10.91162601494192863 ) ) ;
#31868 = CARTESIAN_POINT ( 'NONE',  ( 1.507698388325705758E-15, 7.124999997268799845, -24.62258325217400312 ) ) ;
#31869 = CARTESIAN_POINT ( 'NONE',  ( 24.22776226481265383, 29.32513916574269075, 13.94119854578893580 ) ) ;
#31870 = CARTESIAN_POINT ( 'NONE',  ( -15.14183272437242067, 12.70000000000000639, -20.84094480462497856 ) ) ;
#31871 = CARTESIAN_POINT ( 'NONE',  ( 27.16883889988623935, 20.32500000273118701, -19.73931689729374384 ) ) ;
#31872 = COLOUR_RGB ( '', 0.09019608, 0.27058824, 0.51372549) ;
#31873 = CARTESIAN_POINT ( 'NONE',  ( -26.07999730980477437, 49.23958333333332860, 6.988114217768305103 ) ) ;
#31874 = EDGE_LOOP ( 'NONE', ( #4488, #4021, #3028, #31276 ) ) ;
#31875 = CARTESIAN_POINT ( 'NONE',  ( 33.58253175000000823, 64.02500000273118985, 10.91162601494192863 ) ) ;
#31876 = EDGE_CURVE ( 'NONE', #24787, #28001, #15094, .T. ) ;
#31877 = ORIENTED_EDGE ( 'NONE', *, *, #5392, .T. ) ;
#31878 = CARTESIAN_POINT ( 'NONE',  ( 7.505752307973351023, 17.44270833333333215, 28.01184896238290278 ) ) ;
#31879 = CARTESIAN_POINT ( 'NONE',  ( 14.97647472619947351, 15.29986083425731280, 26.02091320914850314 ) ) ;
#31880 = CARTESIAN_POINT ( 'NONE',  ( -20.75514604977248112, 7.425000002731191984, 28.56700777964554661 ) ) ;
#31881 = EDGE_CURVE ( 'NONE', #28042, #8956, #30405, .T. ) ;
#31882 = VERTEX_POINT ( 'NONE', #15302 ) ;
#31883 = DIRECTION ( 'NONE',  ( -0.000000000000000000, 1.000000000000000000, -0.000000000000000000 ) ) ;
#31884 = CARTESIAN_POINT ( 'NONE',  ( -33.58253175000000113, 25.37500000273118417, 0.000000000000000000 ) ) ;
#31885 = CARTESIAN_POINT ( 'NONE',  ( -32.50000000000000000, 32.40000000546238113, -10.55989012756945478 ) ) ;
#31886 = CARTESIAN_POINT ( 'NONE',  ( 26.29305231718578995, 79.19999999999998863, -19.10302069950538240 ) ) ;
#31887 = CARTESIAN_POINT ( 'NONE',  ( 32.50000000000000711, 33.40000000546238113, 10.55989012756945122 ) ) ;
#31888 = CARTESIAN_POINT ( 'NONE',  ( 10.04305231718579705, 37.10000000546237686, 30.90933677959248982 ) ) ;
#31889 = CARTESIAN_POINT ( 'NONE',  ( -33.58253175000000113, 43.47500000273117138, 10.91162601494193929 ) ) ;
#31890 = CARTESIAN_POINT ( 'NONE',  ( -10.04305231718579172, 23.59999999999999432, -30.90933677959248982 ) ) ;
#31891 = CARTESIAN_POINT ( 'NONE',  ( -32.50000000000000000, 21.90000000000000924, -10.55989012756945478 ) ) ;
#31892 = CARTESIAN_POINT ( 'NONE',  ( 24.50000000000000355, 6.100000000000010303, -7.960532557706203605 ) ) ;
#31893 = CARTESIAN_POINT ( 'NONE',  ( -20.75514604977248823, 60.82500000273121543, -28.56700777964554305 ) ) ;
#31894 = CARTESIAN_POINT ( 'NONE',  ( -5.147494310547418017, 77.55125428154686062, -32.50000000000000000 ) ) ;
#31895 = CARTESIAN_POINT ( 'NONE',  ( -8.219587594935800823, 74.00000000000002842, -12.42830407035704177 ) ) ;
#31896 = CARTESIAN_POINT ( 'NONE',  ( 10.37757302488624056, 54.77500000273119696, -31.93888565452638417 ) ) ;
#31897 = CARTESIAN_POINT ( 'NONE',  ( -14.47279130897151767, 1.324999997268808238, -19.92008829642072598 ) ) ;
#31898 = CARTESIAN_POINT ( 'NONE',  ( 7.570916362186213000, 4.149999994537633796, -23.30088464923126423 ) ) ;
#31899 = CARTESIAN_POINT ( 'NONE',  ( 27.16883889988624290, 3.925000002731188431, 19.73931689729373673 ) ) ;
#31900 = CARTESIAN_POINT ( 'NONE',  ( -26.06988505166735237, 40.65142333425730214, -7.025853678916388567 ) ) ;
#31901 = CARTESIAN_POINT ( 'NONE',  ( 13.67209884950243470, 16.99999999999998934, -19.02727893622179423 ) ) ;
#31902 = CARTESIAN_POINT ( 'NONE',  ( -28.18730216971796310, 52.00000000000000711, 16.82255561449002457 ) ) ;
#31903 = PRODUCT_DEFINITION_CONTEXT ( 'detailed design', #14461, 'design' ) ;
#31904 = CARTESIAN_POINT ( 'NONE',  ( -27.16883889988623935, 31.32500000273118346, 19.73931689729374739 ) ) ;
#31905 = CARTESIAN_POINT ( 'NONE',  ( 32.50000000000000000, 64.99999999999998579, -3.980102097228898626E-15 ) ) ;
#31906 = DIRECTION ( 'NONE',  ( 0.000000000000000000, -1.000000000000000000, 0.000000000000000000 ) ) ;
#31907 = CARTESIAN_POINT ( 'NONE',  ( -8.960552108402744065E-16, 78.37500000273119838, -14.63369212191046209 ) ) ;
#31908 = CARTESIAN_POINT ( 'NONE',  ( 15.04653450569339945, 57.11159749907603356, 25.98046417659831775 ) ) ;
#31909 = CARTESIAN_POINT ( 'NONE',  ( 26.29305231718579350, 53.30000000546237970, 19.10302069950537529 ) ) ;
#31910 = CARTESIAN_POINT ( 'NONE',  ( 2.688165632520823219E-15, 71.87500000273116996, 14.63369212191046387 ) ) ;
#31911 = DIRECTION ( 'NONE',  ( 0.000000000000000000, 0.000000000000000000, -1.000000000000000000 ) ) ;
#31912 = VECTOR ( 'NONE', #32658, 1000.000000000000000 ) ;
#31913 = CARTESIAN_POINT ( 'NONE',  ( -13.97622843553588901, 14.43489583333332682, 24.20753774853756823 ) ) ;
#31914 =( BOUNDED_CURVE ( )  B_SPLINE_CURVE ( 2, ( #31642, #26675, #5230, #18289, #21030, #26169, #2662, #23937, #13640, #32144, #29065, #31809, #23597 ),
 .UNSPECIFIED., .F., .T. ) 
 B_SPLINE_CURVE_WITH_KNOTS ( ( 3, 2, 2, 2, 2, 2, 3 ),
 ( 0.1500000000000000222, 0.1600000000000000033, 0.1799999999999999933, 0.2000000000000000111, 0.2200000000000000011, 0.2399999999999999911, 0.2500000000000000000 ),
 .UNSPECIFIED. ) 
 CURVE ( )  GEOMETRIC_REPRESENTATION_ITEM ( )  RATIONAL_B_SPLINE_CURVE ( ( 0.9755282581475768211, 0.9755282581475768211, 1.000000000000000000, 0.9510565162951535312, 1.000000000000000000, 0.9510565162951535312, 1.000000000000000000, 0.9510565162951535312, 1.000000000000000000, 0.9510565162951535312, 1.000000000000000000, 0.9755282581475768211, 0.9755282581475768211 ) ) 
 REPRESENTATION_ITEM ( '' )  );
#31915 = AXIS2_PLACEMENT_3D ( 'NONE', #12564, #4837, #25610 ) ;
#31916 = CARTESIAN_POINT ( 'NONE',  ( 20.08610463437158344, 71.20000000546237118, 27.64615127144129403 ) ) ;
#31917 = CARTESIAN_POINT ( 'NONE',  ( 7.505752307972854531, 33.19791666666665719, -28.01184896238303423 ) ) ;
#31918 =( BOUNDED_SURFACE ( )  B_SPLINE_SURFACE ( 1, 2, ( 
 ( #18909, #16334, #11010, #858, #29355, #11177, #5691, #16664, #8755, #5856, #26790, #11338, #13591, #3282, #16494, #13750, #5521, #24220, #691, #32095, #24055, #26948, #8590, #18578, #21814, #13918, #32263, #19239, #18744, #19075, #6182, #21480, #523, #29514, #26625, #24385, #8091, #29677, #29186, #2777, #29019, #2947, #357, #13241, #23716, #10671, #21150, #16000, #26456, #23886, #10841, #21319, #31760, #8251, #16169, #3120, #31927, #6858, #17337, #32427, #14758, #19739, #6526, #22475, #22315, #1358, #3781, #12004, #30356, #32923, #16999, #27800, #9422, #24545, #4284, #14088, #27456, #14252, #25221, #32593, #8923, #19406, #22149, #6355, #30184, #6687, #1699, #12176, #16834, #1530, #9092, #1186, #33100, #17171, #19907, #27628, #24876, #11837, #19574, #22647, #11499 ),
 ( #27289, #9603, #1016, #32760, #20085, #29854, #30529, #7026, #21978, #27121, #3614, #24709, #4116, #3947, #14590, #11668, #25049, #30022, #14422, #9254, #10125, #30701, #7372, #4971, #20257, #12694, #13039, #7197, #26077, #25396, #23164, #23343, #33279, #15626, #33805, #9775, #12865, #31052, #2215, #31219, #28140, #20607, #20426, #10462, #12351, #20940, #17678, #9951, #4626, #15105, #28475, #18029, #7544, #2397, #15448, #33626, #25570, #33452, #4453, #2050, #4796, #25903, #12525, #30875, #22993, #10298, #17856, #25736, #18199, #20775, #28308, #2573, #7712, #28642, #15275, #1873, #22820, #5138, #23510, #33968, #31389, #17509, #27970, #14930, #18537, #26752, #15793, #15960, #24014, #11140, #8382, #8051, #10802, #28814, #13551, #28983, #23850, #3245, #651, #142, #486 ) ),
 .UNSPECIFIED., .F., .F., .T. ) 
 B_SPLINE_SURFACE_WITH_KNOTS ( ( 2, 2 ),
 ( 3, 2, 2, 2, 2, 2, 2, 2, 2, 2, 2, 2, 2, 2, 2, 2, 2, 2, 2, 2, 2, 2, 2, 2, 2, 2, 2, 2, 2, 2, 2, 2, 2, 2, 2, 2, 2, 2, 2, 2, 2, 2, 2, 2, 2, 2, 2, 2, 2, 2, 3 ),
 ( 0.000000000000000000, 1.000000000000000000 ),
 ( 0.000000000000000000, 0.02000000000000000042, 0.04000000000000000083, 0.05999999999999999778, 0.08000000000000000167, 0.1000000000000000056, 0.1199999999999999956, 0.1400000000000000133, 0.1600000000000000033, 0.1799999999999999933, 0.2000000000000000111, 0.2200000000000000011, 0.2399999999999999911, 0.2600000000000000089, 0.2800000000000000266, 0.2999999999999999889, 0.3200000000000000067, 0.3400000000000000244, 0.3599999999999999867, 0.3800000000000000044, 0.4000000000000000222, 0.4199999999999999845, 0.4400000000000000022, 0.4600000000000000200, 0.4799999999999999822, 0.5000000000000000000, 0.5200000000000000178, 0.5400000000000000355, 0.5600000000000000533, 0.5799999999999999600, 0.5999999999999999778, 0.6199999999999999956, 0.6400000000000000133, 0.6600000000000000311, 0.6800000000000000488, 0.6999999999999999556, 0.7199999999999999734, 0.7399999999999999911, 0.7600000000000000089, 0.7800000000000000266, 0.8000000000000000444, 0.8199999999999999512, 0.8399999999999999689, 0.8599999999999999867, 0.8800000000000000044, 0.9000000000000000222, 0.9200000000000000400, 0.9399999999999999467, 0.9599999999999999645, 0.9799999999999999822, 1.000000000000000000 ),
 .UNSPECIFIED. ) 
 GEOMETRIC_REPRESENTATION_ITEM ( )  RATIONAL_B_SPLINE_SURFACE ( (
 ( 1.000000000000000000, 0.9510565162951535312, 1.000000000000000000, 0.9510565162951535312, 1.000000000000000000, 0.9510565162951535312, 1.000000000000000000, 0.9510565162951535312, 1.000000000000000000, 0.9510565162951535312, 1.000000000000000000, 0.9510565162951535312, 1.000000000000000000, 0.9510565162951535312, 1.000000000000000000, 0.9510565162951535312, 1.000000000000000000, 0.9510565162951535312, 1.000000000000000000, 0.9510565162951535312, 1.000000000000000000, 0.9510565162951535312, 1.000000000000000000, 0.9510565162951535312, 1.000000000000000000, 0.9510565162951535312, 1.000000000000000000, 0.9510565162951535312, 1.000000000000000000, 0.9510565162951535312, 1.000000000000000000, 0.9510565162951535312, 1.000000000000000000, 0.9510565162951535312, 1.000000000000000000, 0.9510565162951535312, 1.000000000000000000, 0.9510565162951535312, 1.000000000000000000, 0.9510565162951535312, 1.000000000000000000, 0.9510565162951535312, 1.000000000000000000, 0.9510565162951535312, 1.000000000000000000, 0.9510565162951535312, 1.000000000000000000, 0.9510565162951535312, 1.000000000000000000, 0.9510565162951535312, 1.000000000000000000, 0.9510565162951535312, 1.000000000000000000, 0.9510565162951535312, 1.000000000000000000, 0.9510565162951535312, 1.000000000000000000, 0.9510565162951535312, 1.000000000000000000, 0.9510565162951535312, 1.000000000000000000, 0.9510565162951535312, 1.000000000000000000, 0.9510565162951535312, 1.000000000000000000, 0.9510565162951535312, 1.000000000000000000, 0.9510565162951535312, 1.000000000000000000, 0.9510565162951535312, 1.000000000000000000, 0.9510565162951535312, 1.000000000000000000, 0.9510565162951535312, 1.000000000000000000, 0.9510565162951535312, 1.000000000000000000, 0.9510565162951535312, 1.000000000000000000, 0.9510565162951535312, 1.000000000000000000, 0.9510565162951535312, 1.000000000000000000, 0.9510565162951535312, 1.000000000000000000, 0.9510565162951535312, 1.000000000000000000, 0.9510565162951535312, 1.000000000000000000, 0.9510565162951535312, 1.000000000000000000, 0.9510565162951535312, 1.000000000000000000, 0.9510565162951535312, 1.000000000000000000, 0.9510565162951535312, 1.000000000000000000, 0.9510565162951535312, 1.000000000000000000, 0.9510565162951535312, 1.000000000000000000),
 ( 1.000000000000000000, 0.9510565162951535312, 1.000000000000000000, 0.9510565162951535312, 1.000000000000000000, 0.9510565162951535312, 1.000000000000000000, 0.9510565162951535312, 1.000000000000000000, 0.9510565162951535312, 1.000000000000000000, 0.9510565162951535312, 1.000000000000000000, 0.9510565162951535312, 1.000000000000000000, 0.9510565162951535312, 1.000000000000000000, 0.9510565162951535312, 1.000000000000000000, 0.9510565162951535312, 1.000000000000000000, 0.9510565162951535312, 1.000000000000000000, 0.9510565162951535312, 1.000000000000000000, 0.9510565162951535312, 1.000000000000000000, 0.9510565162951535312, 1.000000000000000000, 0.9510565162951535312, 1.000000000000000000, 0.9510565162951535312, 1.000000000000000000, 0.9510565162951535312, 1.000000000000000000, 0.9510565162951535312, 1.000000000000000000, 0.9510565162951535312, 1.000000000000000000, 0.9510565162951535312, 1.000000000000000000, 0.9510565162951535312, 1.000000000000000000, 0.9510565162951535312, 1.000000000000000000, 0.9510565162951535312, 1.000000000000000000, 0.9510565162951535312, 1.000000000000000000, 0.9510565162951535312, 1.000000000000000000, 0.9510565162951535312, 1.000000000000000000, 0.9510565162951535312, 1.000000000000000000, 0.9510565162951535312, 1.000000000000000000, 0.9510565162951535312, 1.000000000000000000, 0.9510565162951535312, 1.000000000000000000, 0.9510565162951535312, 1.000000000000000000, 0.9510565162951535312, 1.000000000000000000, 0.9510565162951535312, 1.000000000000000000, 0.9510565162951535312, 1.000000000000000000, 0.9510565162951535312, 1.000000000000000000, 0.9510565162951535312, 1.000000000000000000, 0.9510565162951535312, 1.000000000000000000, 0.9510565162951535312, 1.000000000000000000, 0.9510565162951535312, 1.000000000000000000, 0.9510565162951535312, 1.000000000000000000, 0.9510565162951535312, 1.000000000000000000, 0.9510565162951535312, 1.000000000000000000, 0.9510565162951535312, 1.000000000000000000, 0.9510565162951535312, 1.000000000000000000, 0.9510565162951535312, 1.000000000000000000, 0.9510565162951535312, 1.000000000000000000, 0.9510565162951535312, 1.000000000000000000, 0.9510565162951535312, 1.000000000000000000, 0.9510565162951535312, 1.000000000000000000, 0.9510565162951535312, 1.000000000000000000) ) ) 
 REPRESENTATION_ITEM ( '' )  SURFACE ( )  );
#31919 = CARTESIAN_POINT ( 'NONE',  ( 1.507698388325705758E-15, 13.62499999726882649, -24.62258325217400312 ) ) ;
#31920 = ORIENTED_EDGE ( 'NONE', *, *, #5240, .T. ) ;
#31921 = CARTESIAN_POINT ( 'NONE',  ( 30.02300923189239867, 38.78944416759064495, 0.04044903254992252006 ) ) ;
#31922 = CARTESIAN_POINT ( 'NONE',  ( 32.50000000000000000, 17.60000000546238397, -10.55989012756945833 ) ) ;
#31923 = CARTESIAN_POINT ( 'NONE',  ( -20.50609665440969209, 48.95312500000000000, 20.50609665441005092 ) ) ;
#31924 = DIRECTION ( 'NONE',  ( -0.4999999999999997224, 0.000000000000000000, 0.8660254037844388186 ) ) ;
#31925 = CARTESIAN_POINT ( 'NONE',  ( 27.16883889988624290, 46.17500000273119554, 19.73931689729373673 ) ) ;
#31926 = CARTESIAN_POINT ( 'NONE',  ( -32.50000000000000000, 58.50000000546237544, 0.000000000000000000 ) ) ;
#31927 = CARTESIAN_POINT ( 'NONE',  ( -4.300734207923755825, 75.77500000273118985, 13.23629886949340673 ) ) ;
#31928 = CARTESIAN_POINT ( 'NONE',  ( -20.75514604977248112, 35.42500000273119554, 28.56700777964554661 ) ) ;
#31929 = CARTESIAN_POINT ( 'NONE',  ( -8.891200544363830713E-16, 75.50000000000000000, -15.00000000000000000 ) ) ;
#31930 = CARTESIAN_POINT ( 'NONE',  ( 10.37757302488624056, 64.77500000273117564, -31.93888565452638417 ) ) ;
#31931 = DIRECTION ( 'NONE',  ( 0.000000000000000000, 0.000000000000000000, 1.000000000000000000 ) ) ;
#31932 = CARTESIAN_POINT ( 'NONE',  ( 33.58253175000000113, 56.22500000273117138, -10.91162601494193574 ) ) ;
#31933 = CARTESIAN_POINT ( 'NONE',  ( -7.505752307972844761, 17.72916666666666430, 28.01184896238304134 ) ) ;
#31934 = CARTESIAN_POINT ( 'NONE',  ( 20.08610463437157279, 41.30000000000001137, -27.64615127144129758 ) ) ;
#31935 = CARTESIAN_POINT ( 'NONE',  ( 23.41746824999999887, 2.624999997268812280, 0.000000000000000000 ) ) ;
#31936 = CARTESIAN_POINT ( 'NONE',  ( -33.58253175000000113, 5.375000002731167292, 0.000000000000000000 ) ) ;
#31937 = CYLINDRICAL_SURFACE ( 'NONE', #21698, 32.50000000000000000 ) ;
#31938 = FACE_OUTER_BOUND ( 'NONE', #304, .T. ) ;
#31939 = CARTESIAN_POINT ( 'NONE',  ( 10.37757302488624767, 73.97500000273119269, 31.93888565452638417 ) ) ;
#31940 = FACE_OUTER_BOUND ( 'NONE', #14473, .T. ) ;
#31941 = CONICAL_SURFACE ( 'NONE', #7845, 13.32050807568876927, 0.2617993877991500740 ) ;
#31942 = CARTESIAN_POINT ( 'NONE',  ( -33.58253175000000113, 65.47500000273117848, 10.91162601494193929 ) ) ;
#31943 = ORIENTED_EDGE ( 'NONE', *, *, #18402, .T. ) ;
#31944 = DIRECTION ( 'NONE',  ( 0.000000000000000000, 0.000000000000000000, -1.000000000000000000 ) ) ;
#31945 = CARTESIAN_POINT ( 'NONE',  ( 24.20753774853731244, 61.12760416666665719, -13.97622843553632599 ) ) ;
#31946 = CARTESIAN_POINT ( 'NONE',  ( 27.16883889988623935, 56.32500000273120122, -19.73931689729374384 ) ) ;
#31947 = CARTESIAN_POINT ( 'NONE',  ( 27.16883889988624290, 12.17500000273118133, 19.73931689729373673 ) ) ;
#31948 = CARTESIAN_POINT ( 'NONE',  ( 20.75514604977249178, 62.07500000273119412, 28.56700777964553950 ) ) ;
#31949 = CARTESIAN_POINT ( 'NONE',  ( 6.988114217767829928, 40.07291666666666430, -26.07999730980489872 ) ) ;
#31950 = CARTESIAN_POINT ( 'NONE',  ( -28.02196122052045268, 33.48996500092397355, 7.468012846824790607 ) ) ;
#31951 = VECTOR ( 'NONE', #5285, 999.9999999999998863 ) ;
#31952 = CARTESIAN_POINT ( 'NONE',  ( 0.04044903255045854962, 23.02305583240935860, 30.02300923189239867 ) ) ;
#31953 = CARTESIAN_POINT ( 'NONE',  ( 32.50000000000000000, 75.60000000546236265, -10.55989012756945833 ) ) ;
#31954 = CARTESIAN_POINT ( 'NONE',  ( 8.601468415847516980, 76.17500000273115290, -11.83890561707634781 ) ) ;
#31955 = CARTESIAN_POINT ( 'NONE',  ( -20.75514604977248112, 37.42500000273118843, 28.56700777964554661 ) ) ;
#31956 = CARTESIAN_POINT ( 'NONE',  ( 24.22776226481265383, 49.95013916574269786, 13.94119854578893580 ) ) ;
#31957 = CARTESIAN_POINT ( 'NONE',  ( 7.236395654485755280, 16.22499999726881370, 22.27133577429736988 ) ) ;
#31958 = FACE_OUTER_BOUND ( 'NONE', #5428, .T. ) ;
#31959 = ORIENTED_EDGE ( 'NONE', *, *, #9685, .F. ) ;
#31960 = CARTESIAN_POINT ( 'NONE',  ( -2.162160676586881955E-15, 50.87500000273119838, -35.31076352940723240 ) ) ;
#31961 = CARTESIAN_POINT ( 'NONE',  ( 20.08610463437158344, 50.69999999999999574, 27.64615127144129403 ) ) ;
#31962 = CARTESIAN_POINT ( 'NONE',  ( -19.11951029504763611, 50.39100666759063785, 19.06425588902592239 ) ) ;
#31963 = PRODUCT_RELATED_PRODUCT_CATEGORY ( 'part', '', ( #27642 ) ) ;
#31964 = CARTESIAN_POINT ( 'NONE',  ( -33.58253175000000113, 69.47500000273116427, 10.91162601494193929 ) ) ;
#31965 = ORIENTED_EDGE ( 'NONE', *, *, #19915, .F. ) ;
#31966 = CARTESIAN_POINT ( 'NONE',  ( -10.37757302488623701, 15.52500000273120051, 31.93888565452638417 ) ) ;
#31967 = AXIS2_PLACEMENT_3D ( 'NONE', #26096, #20627, #29164 ) ;
#31968 = CARTESIAN_POINT ( 'NONE',  ( -7.505752307973343918, 29.47395833333332860, -28.01184896238290989 ) ) ;
#31969 = ORIENTED_EDGE ( 'NONE', *, *, #27745, .T. ) ;
#31970 = CARTESIAN_POINT ( 'NONE',  ( 27.16883889988624290, 55.92500000273120975, 19.73931689729373673 ) ) ;
#31971 = CARTESIAN_POINT ( 'NONE',  ( 15.01150461594596308, 50.52864583333333570, -26.00068869287367335 ) ) ;
#31972 = CARTESIAN_POINT ( 'NONE',  ( -26.29305231718579350, 16.30000000546239036, -19.10302069950537884 ) ) ;
#31973 = CARTESIAN_POINT ( 'NONE',  ( -30.16025403784430736, -22.00000000000000000, 0.000000000000000000 ) ) ;
#31974 = CARTESIAN_POINT ( 'NONE',  ( 1.507698388325705758E-15, 9.624999997268808727, -24.62258325217400312 ) ) ;
#31975 = CARTESIAN_POINT ( 'NONE',  ( -33.58253175000000113, 21.47500000273119980, 10.91162601494193929 ) ) ;
#31976 = DIRECTION ( 'NONE',  ( 0.000000000000000000, -1.000000000000000000, 0.000000000000000000 ) ) ;
#31977 = CARTESIAN_POINT ( 'NONE',  ( 20.47846945139867003, 66.42149333240935505, -20.53372385742107653 ) ) ;
#31978 = CARTESIAN_POINT ( 'NONE',  ( 11.25946833292375793, 79.67500000273119554, 8.180482586598731842 ) ) ;
#31979 = CARTESIAN_POINT ( 'NONE',  ( -10.04305231718578462, 4.400000000000014566, 30.90933677959249337 ) ) ;
#31980 = CARTESIAN_POINT ( 'NONE',  ( 10.04305231718578817, 13.40000000000000924, -30.90933677959249337 ) ) ;
#31981 = EDGE_LOOP ( 'NONE', ( #30237, #4660, #33620, #20592 ) ) ;
#31982 = CARTESIAN_POINT ( 'NONE',  ( -19.82091636218621034, 18.54999999453762882, -14.40073868116559552 ) ) ;
#31983 = CARTESIAN_POINT ( 'NONE',  ( 4.300734207923761154, 77.47500000273119269, 13.23629886949340495 ) ) ;
#31984 = CARTESIAN_POINT ( 'NONE',  ( -19.09188309203694445, 36.06250000000000000, -19.09188309203661049 ) ) ;
#31985 = CARTESIAN_POINT ( 'NONE',  ( 33.58253175000000823, 24.02500000273117564, 10.91162601494192863 ) ) ;
#31986 = CARTESIAN_POINT ( 'NONE',  ( 6.486482029760649416E-15, 75.62500000273121259, 35.31076352940723240 ) ) ;
#31987 = CARTESIAN_POINT ( 'NONE',  ( 27.16883889988624290, 30.17500000273119909, 19.73931689729373673 ) ) ;
#31988 = VECTOR ( 'NONE', #12324, 1000.000000000000000 ) ;
#31989 = CARTESIAN_POINT ( 'NONE',  ( 33.58253175000000113, 18.47500000273117848, -10.91162601494193574 ) ) ;
#31990 = CARTESIAN_POINT ( 'NONE',  ( -19.11951029504763611, 53.82850666759064495, 19.06425588902592239 ) ) ;
#31991 = CARTESIAN_POINT ( 'NONE',  ( 33.58253175000000823, 70.02500000273120406, 10.91162601494192685 ) ) ;
#31992 = DIRECTION ( 'NONE',  ( -0.000000000000000000, -1.000000000000000000, -0.000000000000000000 ) ) ;
#31993 = CARTESIAN_POINT ( 'NONE',  ( -4.300734207923759378, 80.97500000273119269, -13.23629886949340495 ) ) ;
#31994 = CARTESIAN_POINT ( 'NONE',  ( -32.50000000000000000, 55.90000000000000568, -10.55989012756945478 ) ) ;
#31995 = CARTESIAN_POINT ( 'NONE',  ( -2.375766604868045029, 71.80125428700922896, -14.99999999999999822 ) ) ;
#31996 = CARTESIAN_POINT ( 'NONE',  ( -2.162160676586882350E-15, 58.62500000273118417, -35.31076352940722529 ) ) ;
#31997 = CARTESIAN_POINT ( 'NONE',  ( -23.41746824999999887, 18.12499999726882649, -2.867812753649727150E-15 ) ) ;
#31998 = ORIENTED_EDGE ( 'NONE', *, *, #31274, .T. ) ;
#31999 = CARTESIAN_POINT ( 'NONE',  ( 10.37757302488624056, 64.77500000273118985, -31.93888565452638417 ) ) ;
#32000 = CARTESIAN_POINT ( 'NONE',  ( -32.50000000000000000, 61.89999999999999147, -10.55989012756945300 ) ) ;
#32001 = CARTESIAN_POINT ( 'NONE',  ( 1.507698388325705758E-15, 5.124999997268805174, -24.62258325217400312 ) ) ;
#32002 = CARTESIAN_POINT ( 'NONE',  ( 6.950374756619721595, 25.75559000092397710, 26.09010956794232428 ) ) ;
#32003 = ORIENTED_EDGE ( 'NONE', *, *, #27471, .T. ) ;
#32004 = CARTESIAN_POINT ( 'NONE',  ( -10.37757302488624411, 38.72500000273119980, -31.93888565452638417 ) ) ;
#32005 = CARTESIAN_POINT ( 'NONE',  ( -10.72870458603807542, -72.44024934668307480, 1.313887373028906602E-15 ) ) ;
#32006 = EDGE_CURVE ( 'NONE', #31666, #14496, #24506, .T. ) ;
#32007 = VERTEX_POINT ( 'NONE', #20632 ) ;
#32008 = CARTESIAN_POINT ( 'NONE',  ( 28.01184896238290278, 47.52083333333332860, -7.505752307973347470 ) ) ;
#32009 = CARTESIAN_POINT ( 'NONE',  ( -5.147494310547377161, 60.05125428700922896, -32.50000000000002132 ) ) ;
#32010 = CARTESIAN_POINT ( 'NONE',  ( -24.50000000000000711, 3.099999999999989431, 7.960532557706201828 ) ) ;
#32011 = CARTESIAN_POINT ( 'NONE',  ( 10.37757302488624056, 72.52500000273120406, -31.93888565452638417 ) ) ;
#32012 = CARTESIAN_POINT ( 'NONE',  ( 15.01150461594643204, 17.29947916666666430, 26.00068869287340334 ) ) ;
#32013 = CARTESIAN_POINT ( 'NONE',  ( 19.82091636218621034, 7.800000000000001599, 14.40073868116559730 ) ) ;
#32014 = CARTESIAN_POINT ( 'NONE',  ( 10.37757302488624767, 9.975000002731187365, 31.93888565452638417 ) ) ;
#32015 = CARTESIAN_POINT ( 'NONE',  ( 6.486482029760649416E-15, 17.62500000273117351, 35.31076352940723240 ) ) ;
#32016 =( BOUNDED_CURVE ( )  B_SPLINE_CURVE ( 2, ( #29462, #8536, #21764, #16941, #803, #16279, #26737, #19350, #27061, #24329, #8700, #24490, #13699 ),
 .UNSPECIFIED., .F., .T. ) 
 B_SPLINE_CURVE_WITH_KNOTS ( ( 3, 2, 2, 2, 2, 2, 3 ),
 ( 0.3269230769230769273, 0.3282051282051282048, 0.3307692307692307598, 0.3333333333333333148, 0.3358974358974358698, 0.3384615384615384803, 0.3397435897435897578 ),
 .UNSPECIFIED. ) 
 CURVE ( )  GEOMETRIC_REPRESENTATION_ITEM ( )  RATIONAL_B_SPLINE_CURVE ( ( 0.9755282581475768211, 0.9755282581475768211, 1.000000000000000000, 0.9510565162951535312, 1.000000000000000000, 0.9510565162951535312, 1.000000000000000000, 0.9510565162951535312, 1.000000000000000000, 0.9510565162951535312, 1.000000000000000000, 0.9755282581475768211, 0.9755282581475768211 ) ) 
 REPRESENTATION_ITEM ( '' )  );
#32017 = CARTESIAN_POINT ( 'NONE',  ( -4.300734207923759378, 80.47500000273119269, -13.23629886949340495 ) ) ;
#32018 = CARTESIAN_POINT ( 'NONE',  ( 1.806199397676865774E-16, -24.47487373415291145, 0.000000000000000000 ) ) ;
#32019 = CARTESIAN_POINT ( 'NONE',  ( -26.02091320914878025, 37.91888916574269075, -14.97647472619899389 ) ) ;
#32020 = CARTESIAN_POINT ( 'NONE',  ( -4.300734207923755825, 77.77500000273118985, 13.23629886949340673 ) ) ;
#32021 = CARTESIAN_POINT ( 'NONE',  ( -28.01184896238290278, 45.80208333333333570, 7.505752307973363457 ) ) ;
#32022 = EDGE_CURVE ( 'NONE', #9005, #20850, #31723, .T. ) ;
#32023 = CARTESIAN_POINT ( 'NONE',  ( -3.880418787951104953, 11.44874571845314293, 24.50000000000000711 ) ) ;
#32024 = DIRECTION ( 'NONE',  ( -0.000000000000000000, 1.000000000000000000, -0.000000000000000000 ) ) ;
#32025 = CARTESIAN_POINT ( 'NONE',  ( -13.94119854578892514, 57.68451416574269075, 24.22776226481266448 ) ) ;
#32026 = CARTESIAN_POINT ( 'NONE',  ( -20.75514604977248112, 43.42500000273117422, 28.56700777964554661 ) ) ;
#32027 = CARTESIAN_POINT ( 'NONE',  ( 4.635254915624209993, 73.65000000546240244, -14.26584774442730463 ) ) ;
#32028 = CARTESIAN_POINT ( 'NONE',  ( -33.58253175000000113, 47.47500000273119269, 10.91162601494193929 ) ) ;
#32029 = CARTESIAN_POINT ( 'NONE',  ( -10.37757302488623701, 37.77500000273118275, 31.93888565452638417 ) ) ;
#32030 = CARTESIAN_POINT ( 'NONE',  ( -0.4126531432213792483, 16.99999999999998579, 24.09281253189301353 ) ) ;
#32031 = CARTESIAN_POINT ( 'NONE',  ( 26.07999730980477437, 23.45833333333333215, -6.988114217768290004 ) ) ;
#32032 = PRESENTATION_LAYER_ASSIGNMENT (  '', '', ( #28197 ) ) ;
#32033 = CARTESIAN_POINT ( 'NONE',  ( -4.635254915624211769, 79.60000000000000853, -14.26584774442730286 ) ) ;
#32034 = CARTESIAN_POINT ( 'NONE',  ( 20.08610463437158344, 70.70000000000000284, 27.64615127144129403 ) ) ;
#32035 = CARTESIAN_POINT ( 'NONE',  ( 10.37757302488624767, 9.725000002731173154, 31.93888565452638417 ) ) ;
#32036 = CARTESIAN_POINT ( 'NONE',  ( -4.523095164977117273E-15, 2.124999997268811835, 24.62258325217400312 ) ) ;
#32037 = DIRECTION ( 'NONE',  ( -0.000000000000000000, -1.000000000000000000, -0.000000000000000000 ) ) ;
#32038 = CARTESIAN_POINT ( 'NONE',  ( -7.025853678916861966, 31.47357666574268364, -26.06988505166722803 ) ) ;
#32039 = CARTESIAN_POINT ( 'NONE',  ( -20.08610463437156923, 60.29999999999997584, 27.64615127144130113 ) ) ;
#32040 = CARTESIAN_POINT ( 'NONE',  ( -10.37757302488623701, 21.52500000273119340, 31.93888565452638417 ) ) ;
#32041 = CARTESIAN_POINT ( 'NONE',  ( -13.97622843553588901, 55.68489583333332860, 24.20753774853756823 ) ) ;
#32042 = ORIENTED_EDGE ( 'NONE', *, *, #18121, .F. ) ;
#32043 = CARTESIAN_POINT ( 'NONE',  ( -33.58253175000000113, 55.22500000273117848, 10.91162601494193929 ) ) ;
#32044 = ORIENTED_EDGE ( 'NONE', *, *, #22250, .F. ) ;
#32045 = CARTESIAN_POINT ( 'NONE',  ( 2.740863092043355209E-13, 21.02343749999999645, 30.02300923189239512 ) ) ;
#32046 = CARTESIAN_POINT ( 'NONE',  ( 30.02300923189239867, 25.03944416759064495, 0.04044903254992252006 ) ) ;
#32047 = CARTESIAN_POINT ( 'NONE',  ( 15.14183272437242067, 15.44999999453762207, 20.84094480462498211 ) ) ;
#32048 = EDGE_LOOP ( 'NONE', ( #18145, #28892, #4153, #4962 ) ) ;
#32049 = CARTESIAN_POINT ( 'NONE',  ( -14.47279130897152122, 1.924999997268818541, 19.92008829642072243 ) ) ;
#32050 = CARTESIAN_POINT ( 'NONE',  ( -2.162160676586881955E-15, 26.87500000273116996, -35.31076352940723240 ) ) ;
#32051 =( BOUNDED_CURVE ( )  B_SPLINE_CURVE ( 2, ( #18441, #31289, #15862, #21349, #2644, #31791, #7783, #18269, #28717, #13107, #23581, #46, #2807 ),
 .UNSPECIFIED., .F., .F. ) 
 B_SPLINE_CURVE_WITH_KNOTS ( ( 3, 2, 2, 2, 2, 2, 3 ),
 ( 0.9679487179487179516, 0.9692307692307692291, 0.9717948717948717841, 0.9743589743589743390, 0.9769230769230768940, 0.9794871794871794490, 0.9807692307692307265 ),
 .UNSPECIFIED. ) 
 CURVE ( )  GEOMETRIC_REPRESENTATION_ITEM ( )  RATIONAL_B_SPLINE_CURVE ( ( 0.9755282581475768211, 0.9755282581475768211, 1.000000000000000000, 0.9510565162951535312, 1.000000000000000000, 0.9510565162951535312, 1.000000000000000000, 0.9510565162951535312, 1.000000000000000000, 0.9510565162951535312, 1.000000000000000000, 0.9755282581475768211, 0.9755282581475768211 ) ) 
 REPRESENTATION_ITEM ( '' )  );
#32052 = MECHANICAL_DESIGN_GEOMETRIC_PRESENTATION_REPRESENTATION (  '', ( #12317 ), #16710 ) ;
#32053 = CARTESIAN_POINT ( 'NONE',  ( 6.277390505771533514E-15, 29.00000000546237189, 34.17252228774368916 ) ) ;
#32054 = CARTESIAN_POINT ( 'NONE',  ( 32.50000000000000000, 77.00000000000001421, -3.980102097228898626E-15 ) ) ;
#32055 = CARTESIAN_POINT ( 'NONE',  ( -20.08610463437156923, 54.80000000546236549, 27.64615127144130113 ) ) ;
#32056 = LINE ( 'NONE', #11303, #589 ) ;
#32057 = CARTESIAN_POINT ( 'NONE',  ( -10.37757302488623701, 41.77500000273118275, 31.93888565452638417 ) ) ;
#32058 =( NAMED_UNIT ( * ) SI_UNIT ( $, .STERADIAN. ) SOLID_ANGLE_UNIT ( ) );
#32059 = CARTESIAN_POINT ( 'NONE',  ( -26.29305231718578995, 22.19999999999998508, 19.10302069950538595 ) ) ;
#32060 = CARTESIAN_POINT ( 'NONE',  ( 20.08610463437158344, 22.70000000000000995, 27.64615127144129403 ) ) ;
#32061 = CARTESIAN_POINT ( 'NONE',  ( 15.14183272437242245, 14.30000000000001315, -20.84094480462497856 ) ) ;
#32062 = CARTESIAN_POINT ( 'NONE',  ( 33.58253175000000113, 66.12500000273119838, -4.112674001490185761E-15 ) ) ;
#32063 = CARTESIAN_POINT ( 'NONE',  ( 10.37757302488624056, 52.77500000273118985, -31.93888565452638417 ) ) ;
#32064 = CARTESIAN_POINT ( 'NONE',  ( 1.507698388325705758E-15, 9.124999997268822938, -24.62258325217400312 ) ) ;
#32065 = CARTESIAN_POINT ( 'NONE',  ( -4.223320258572819786E-15, 9.499999999999992895, 24.50000000000000000 ) ) ;
#32066 = CARTESIAN_POINT ( 'NONE',  ( -10.37757302488624411, 2.725000002731181592, -31.93888565452638417 ) ) ;
#32067 = CARTESIAN_POINT ( 'NONE',  ( -13.94119854578936923, 41.08111083425730214, -24.22776226481241224 ) ) ;
#32068 = EDGE_CURVE ( 'NONE', #28845, #2126, #15069, .T. ) ;
#32069 = CARTESIAN_POINT ( 'NONE',  ( 30.22248186753583710, 66.99999999999998579, -12.55019540181426052 ) ) ;
#32070 = MANIFOLD_SOLID_BREP ( 'Cavity1', #1300 ) ;
#32071 = FACE_OUTER_BOUND ( 'NONE', #4872, .T. ) ;
#32072 = CARTESIAN_POINT ( 'NONE',  ( -33.58253175000000113, 31.12500000273120548, 0.000000000000000000 ) ) ;
#32073 = CARTESIAN_POINT ( 'NONE',  ( -1.053607264507113999E-13, 64.50000000000000000, 32.50000000000000711 ) ) ;
#32074 = CARTESIAN_POINT ( 'NONE',  ( 32.50000000000000000, 61.60000000546236265, -10.55989012756945833 ) ) ;
#32075 = EDGE_CURVE ( 'NONE', #21334, #9459, #18621, .T. ) ;
#32076 = CARTESIAN_POINT ( 'NONE',  ( 5.147494310547434893, 1.051254287009222965, 32.49999999999999289 ) ) ;
#32077 = CARTESIAN_POINT ( 'NONE',  ( -20.53372385742107653, 58.68711833240935505, -20.47846945139867003 ) ) ;
#32078 = CARTESIAN_POINT ( 'NONE',  ( -32.50000000000000000, 48.40000000546237402, -10.55989012756945478 ) ) ;
#32079 = AXIS2_PLACEMENT_3D ( 'NONE', #16005, #23554, #11014 ) ;
#32080 = DIRECTION ( 'NONE',  ( -0.000000000000000000, 1.000000000000000000, -0.000000000000000000 ) ) ;
#32081 =( NAMED_UNIT ( * ) PLANE_ANGLE_UNIT ( ) SI_UNIT ( $, .RADIAN. ) );
#32082 = CARTESIAN_POINT ( 'NONE',  ( 13.97622843553633665, 27.61197916666666430, 24.20753774853730889 ) ) ;
#32083 = EDGE_LOOP ( 'NONE', ( #18270, #9124, #4682, #2387 ) ) ;
#32084 = CARTESIAN_POINT ( 'NONE',  ( -33.58253175000000113, 73.12500000273118417, 0.000000000000000000 ) ) ;
#32085 = CARTESIAN_POINT ( 'NONE',  ( 28.01184896238290278, 30.33333333333332860, -7.505752307973347470 ) ) ;
#32086 = CARTESIAN_POINT ( 'NONE',  ( -7.236395654485757944, 11.72499999726880837, -22.27133577429736988 ) ) ;
#32087 = ORIENTED_EDGE ( 'NONE', *, *, #23790, .T. ) ;
#32088 = CARTESIAN_POINT ( 'NONE',  ( 28.00173670424549499, 52.68267333425730214, 7.543491769121417612 ) ) ;
#32089 = CARTESIAN_POINT ( 'NONE',  ( -10.04305231718579172, 20.10000000546237331, -30.90933677959248982 ) ) ;
#32090 = CARTESIAN_POINT ( 'NONE',  ( -7.505752307972844761, 52.10416666666666430, 28.01184896238304134 ) ) ;
#32091 = CARTESIAN_POINT ( 'NONE',  ( -32.50000000000000000, 36.09999999999999432, 10.55989012756946366 ) ) ;
#32092 = CARTESIAN_POINT ( 'NONE',  ( 33.58253175000000113, 48.47500000273118559, -10.91162601494193751 ) ) ;
#32093 = CARTESIAN_POINT ( 'NONE',  ( 20.08610463437158344, 53.20000000546237118, 27.64615127144129403 ) ) ;
#32094 = PRODUCT ( 'connector', 'connector', '', ( #280 ) ) ;
#32095 = CARTESIAN_POINT ( 'NONE',  ( -13.91746824999999532, 79.47500000273115006, 4.522059556121122093 ) ) ;
#32096 = CARTESIAN_POINT ( 'NONE',  ( -10.37757302488624411, 38.72500000273118559, -31.93888565452638417 ) ) ;
#32097 = CARTESIAN_POINT ( 'NONE',  ( 27.16883889988623935, 62.57500000273119412, -19.73931689729374384 ) ) ;
#32098 = CARTESIAN_POINT ( 'NONE',  ( -10.04305231718578462, 42.39999999999999147, 30.90933677959249337 ) ) ;
#32099 = CARTESIAN_POINT ( 'NONE',  ( 14.47279130897151767, 10.92499999726882365, -19.92008829642072598 ) ) ;
#32100 = CARTESIAN_POINT ( 'NONE',  ( 10.37757302488624767, 1.975000002731180926, 31.93888565452638417 ) ) ;
#32101 = DIRECTION ( 'NONE',  ( 0.000000000000000000, 0.000000000000000000, -1.000000000000000000 ) ) ;
#32102 = CARTESIAN_POINT ( 'NONE',  ( -13.91746824999999887, 75.37500000273116996, 0.000000000000000000 ) ) ;
#32103 = CARTESIAN_POINT ( 'NONE',  ( -10.37757302488624411, 70.97500000273119269, -31.93888565452638417 ) ) ;
#32104 = DIRECTION ( 'NONE',  ( 0.000000000000000000, 0.000000000000000000, 1.000000000000000000 ) ) ;
#32105 = CARTESIAN_POINT ( 'NONE',  ( -2.162160676586881955E-15, 70.87500000273118417, -35.31076352940723240 ) ) ;
#32106 = ORIENTED_EDGE ( 'NONE', *, *, #25184, .T. ) ;
#32107 = CARTESIAN_POINT ( 'NONE',  ( -4.523095164977116484E-15, 18.62499999726881583, 24.62258325217400312 ) ) ;
#32108 = CARTESIAN_POINT ( 'NONE',  ( 24.18731323226247554, 11.57590250092397355, 14.01125832528285997 ) ) ;
#32109 = ADVANCED_FACE ( 'NONE', ( #5165 ), #26272, .F. ) ;
#32110 = DIRECTION ( 'NONE',  ( -1.000000000000000000, 0.000000000000000000, 0.000000000000000000 ) ) ;
#32111 = CIRCLE ( 'NONE', #27734, 16.50000000000002842 ) ;
#32112 = CARTESIAN_POINT ( 'NONE',  ( -10.37757302488623701, 45.52500000273117564, 31.93888565452638417 ) ) ;
#32113 = CARTESIAN_POINT ( 'NONE',  ( -10.37757302488624411, 10.97500000273120335, -31.93888565452638417 ) ) ;
#32114 = CARTESIAN_POINT ( 'NONE',  ( -33.58253175000000113, 63.27500000273118985, -10.91162601494193041 ) ) ;
#32115 = CARTESIAN_POINT ( 'NONE',  ( 6.988114217767829928, 53.82291666666666430, -26.07999730980489872 ) ) ;
#32116 =( BOUNDED_CURVE ( )  B_SPLINE_CURVE ( 2, ( #19808, #16903, #16738, #14662, #6431, #32995, #30431 ),
 .UNSPECIFIED., .F., .T. ) 
 B_SPLINE_CURVE_WITH_KNOTS ( ( 3, 2, 2, 3 ),
 ( 0.9935897435897436125, 0.9948717948717948900, 0.9974358974358974450, 1.000000000000000000 ),
 .UNSPECIFIED. ) 
 CURVE ( )  GEOMETRIC_REPRESENTATION_ITEM ( )  RATIONAL_B_SPLINE_CURVE ( ( 0.9755282581475768211, 0.9755282581475768211, 1.000000000000000000, 0.9510565162951535312, 1.000000000000000000, 0.9510565162951535312, 1.000000000000000000 ) ) 
 REPRESENTATION_ITEM ( '' )  );
#32117 = CARTESIAN_POINT ( 'NONE',  ( -0.04044903254990864921, 43.08631916759065916, 30.02300923189239867 ) ) ;
#32118 = EDGE_CURVE ( 'NONE', #13788, #4296, #167, .T. ) ;
#32119 = CARTESIAN_POINT ( 'NONE',  ( -28.02196122052058413, 27.46315999907601935, -7.468012846824272799 ) ) ;
#32120 = CARTESIAN_POINT ( 'NONE',  ( -32.50000000000000000, 68.60000000546237686, 10.55989012756946366 ) ) ;
#32121 = CARTESIAN_POINT ( 'NONE',  ( 13.91746824999999887, 79.87500000273118417, -1.704398294459741270E-15 ) ) ;
#32122 =( BOUNDED_CURVE ( )  B_SPLINE_CURVE ( 2, ( #32301, #10884, #26989, #8293, #11536, #6053, #21359, #5897, #3488, #16537, #26666, #8463, #18622 ),
 .UNSPECIFIED., .F., .T. ) 
 B_SPLINE_CURVE_WITH_KNOTS ( ( 3, 2, 2, 2, 2, 2, 3 ),
 ( 0.02777777777777777971, 0.03333333333333333287, 0.04444444444444444614, 0.05555555555555555247, 0.06666666666666667962, 0.07777777777777777901, 0.08333333333333334259 ),
 .UNSPECIFIED. ) 
 CURVE ( )  GEOMETRIC_REPRESENTATION_ITEM ( )  RATIONAL_B_SPLINE_CURVE ( ( 0.9755282581475768211, 0.9755282581475768211, 1.000000000000000000, 0.9510565162951535312, 1.000000000000000000, 0.9510565162951535312, 1.000000000000000000, 0.9510565162951535312, 1.000000000000000000, 0.9510565162951535312, 1.000000000000000000, 0.9755282581475767101, 0.9755282581475768211 ) ) 
 REPRESENTATION_ITEM ( '' )  );
#32123 = CARTESIAN_POINT ( 'NONE',  ( -0.04044903255042732459, 59.11680583240937636, -27.95245687107223986 ) ) ;
#32124 = CARTESIAN_POINT ( 'NONE',  ( -18.94512977948575738, 13.42499999726881654, -13.76444248337723231 ) ) ;
#32125 = CARTESIAN_POINT ( 'NONE',  ( 10.04305231718578817, 59.40000000000000568, -30.90933677959249337 ) ) ;
#32126 = ORIENTED_EDGE ( 'NONE', *, *, #6421, .T. ) ;
#32127 = CARTESIAN_POINT ( 'NONE',  ( -2.162160676586881955E-15, 48.87500000273117706, -35.31076352940723240 ) ) ;
#32128 = CARTESIAN_POINT ( 'NONE',  ( -10.04305231718578462, 50.90000000546238113, 30.90933677959249337 ) ) ;
#32129 = MANIFOLD_SOLID_BREP ( 'Cavity1', #10105 ) ;
#32130 = CARTESIAN_POINT ( 'NONE',  ( 13.94119854578937812, 53.11236083425731636, 24.22776226481240514 ) ) ;
#32131 = CARTESIAN_POINT ( 'NONE',  ( -33.58253175000000113, 67.37500000273119838, 0.000000000000000000 ) ) ;
#32132 = ORIENTED_EDGE ( 'NONE', *, *, #13841, .T. ) ;
#32133 = CARTESIAN_POINT ( 'NONE',  ( 20.75514604977248467, 20.42500000273120619, -28.56700777964554305 ) ) ;
#32134 = CARTESIAN_POINT ( 'NONE',  ( 26.00068869287367335, 23.88802083333331794, 15.01150461594596308 ) ) ;
#32135 = ORIENTED_EDGE ( 'NONE', *, *, #30437, .F. ) ;
#32136 = DIRECTION ( 'NONE',  ( 0.000000000000000000, 0.000000000000000000, -1.000000000000000000 ) ) ;
#32137 = CARTESIAN_POINT ( 'NONE',  ( -10.37757302488623701, 55.52500000273119696, 31.93888565452638417 ) ) ;
#32138 = CARTESIAN_POINT ( 'NONE',  ( 20.50609665440969565, 54.10937499999999289, -20.50609665441004736 ) ) ;
#32139 = CARTESIAN_POINT ( 'NONE',  ( -2.092463501923844636E-15, 16.00000000546237544, -34.17252228774368916 ) ) ;
#32140 = DIRECTION ( 'NONE',  ( -0.000000000000000000, 1.000000000000000000, -0.000000000000000000 ) ) ;
#32141 = AXIS2_PLACEMENT_3D ( 'NONE', #14346, #19499, #13849 ) ;
#32142 = CARTESIAN_POINT ( 'NONE',  ( 14.47279130897151944, 11.42499999726880944, -19.92008829642072598 ) ) ;
#32143 = CARTESIAN_POINT ( 'NONE',  ( -27.16883889988623935, 21.57500000273118701, 19.73931689729374739 ) ) ;
#32144 = CARTESIAN_POINT ( 'NONE',  ( -9.270509831248423538, 77.95000000546237118, -12.75976212528059861 ) ) ;
#32145 = CARTESIAN_POINT ( 'NONE',  ( -26.06988505166722803, 20.30170166574269075, 7.025853678916877953 ) ) ;
#32146 = CARTESIAN_POINT ( 'NONE',  ( 10.04305231718579705, 65.10000000546239107, 30.90933677959248982 ) ) ;
#32147 = DIRECTION ( 'NONE',  ( 1.000000000000000000, 1.416100796715761110E-16, 0.000000000000000000 ) ) ;
#32148 = VECTOR ( 'NONE', #31292, 999.9999999999998863 ) ;
#32149 = CARTESIAN_POINT ( 'NONE',  ( 26.29305231718578995, 13.20000000000000284, -19.10302069950538240 ) ) ;
#32150 = EDGE_LOOP ( 'NONE', ( #21599, #5724, #10353, #16568 ) ) ;
#32151 = CARTESIAN_POINT ( 'NONE',  ( -15.14183272437241889, 18.44999999453764161, -20.84094480462497856 ) ) ;
#32152 = CARTESIAN_POINT ( 'NONE',  ( -4.300734207923759378, 74.47500000273119269, -13.23629886949340495 ) ) ;
#32153 = CARTESIAN_POINT ( 'NONE',  ( 26.07999730980490227, 37.49479166666666430, 6.988114217767821046 ) ) ;
#32154 = CARTESIAN_POINT ( 'NONE',  ( 27.16883889988624290, 27.92500000273118133, 19.73931689729373673 ) ) ;
#32155 = CARTESIAN_POINT ( 'NONE',  ( -10.37757302488624411, 66.72500000273116427, -31.93888565452638417 ) ) ;
#32156 = CARTESIAN_POINT ( 'NONE',  ( 20.75514604977248467, 32.67500000273118843, -28.56700777964554305 ) ) ;
#32157 = CARTESIAN_POINT ( 'NONE',  ( -33.58253175000000113, 15.47500000273118381, 10.91162601494193929 ) ) ;
#32158 = CARTESIAN_POINT ( 'NONE',  ( -27.16883889988624290, 7.175000002731191096, -19.73931689729374028 ) ) ;
#32159 = CARTESIAN_POINT ( 'NONE',  ( -6.950374756619716266, 61.84934000092397355, -26.09010956794232428 ) ) ;
#32160 = CARTESIAN_POINT ( 'NONE',  ( -33.58253175000000113, 71.02500000273117564, -10.91162601494193041 ) ) ;
#32161 = CARTESIAN_POINT ( 'NONE',  ( 30.02300923189239512, 54.53906249999998579, -2.619432448724977703E-13 ) ) ;
#32162 = DIRECTION ( 'NONE',  ( 0.000000000000000000, 0.000000000000000000, 1.000000000000000000 ) ) ;
#32163 = CARTESIAN_POINT ( 'NONE',  ( 13.91746825000000065, 76.27500000273118985, 4.522059556121115875 ) ) ;
#32164 = CARTESIAN_POINT ( 'NONE',  ( 10.04305231718578817, 53.39999999999999147, -30.90933677959249337 ) ) ;
#32165 = PLANE ( 'NONE',  #12801 ) ;
#32166 = CARTESIAN_POINT ( 'NONE',  ( 10.37757302488624767, 59.72500000273117848, 31.93888565452638417 ) ) ;
#32167 = CARTESIAN_POINT ( 'NONE',  ( -18.94512977948575738, 15.92499999726881832, -13.76444248337723231 ) ) ;
#32168 = VECTOR ( 'NONE', #21545, 1000.000000000000000 ) ;
#32169 = ORIENTED_EDGE ( 'NONE', *, *, #3894, .T. ) ;
#32170 = CARTESIAN_POINT ( 'NONE',  ( -27.16883889988623935, 65.57500000273118701, 19.73931689729374739 ) ) ;
#32171 = CARTESIAN_POINT ( 'NONE',  ( 26.50000000000000000, -22.99999999999999645, 3.245314017740485765E-15 ) ) ;
#32172 = CARTESIAN_POINT ( 'NONE',  ( 23.41746824999999887, 4.624999997268814056, 0.000000000000000000 ) ) ;
#32173 = CARTESIAN_POINT ( 'NONE',  ( -6.950374756619716266, 27.47434000092397000, -26.09010956794232428 ) ) ;
#32174 = VERTEX_POINT ( 'NONE', #8238 ) ;
#32175 = CARTESIAN_POINT ( 'NONE',  ( -20.75514604977248112, 35.42500000273119554, 28.56700777964554661 ) ) ;
#32176 = CARTESIAN_POINT ( 'NONE',  ( -20.08610463437157989, 42.20000000546238539, -27.64615127144129758 ) ) ;
#32177 = ORIENTED_EDGE ( 'NONE', *, *, #1170, .T. ) ;
#32178 = CARTESIAN_POINT ( 'NONE',  ( 26.00068869287340334, 47.37760416666666430, -15.01150461594642316 ) ) ;
#32179 = CARTESIAN_POINT ( 'NONE',  ( 33.58253175000000823, 66.27500000273117564, 10.91162601494192685 ) ) ;
#32180 = CARTESIAN_POINT ( 'NONE',  ( 26.29305231718578995, 59.20000000000001705, -19.10302069950538240 ) ) ;
#32181 = CARTESIAN_POINT ( 'NONE',  ( 20.75514604977248467, 76.42500000273118133, -28.56700777964554305 ) ) ;
#32182 = CARTESIAN_POINT ( 'NONE',  ( 20.50609665440969565, 30.04687500000000000, -20.50609665441004736 ) ) ;
#32183 = CARTESIAN_POINT ( 'NONE',  ( -24.50000000000000355, 6.899999999999985256, -7.960532557706207157 ) ) ;
#32184 = CARTESIAN_POINT ( 'NONE',  ( 33.58253175000000113, 8.475000002731173154, -10.91162601494193751 ) ) ;
#32185 = CARTESIAN_POINT ( 'NONE',  ( 33.58253175000000113, 18.22500000273118559, -10.91162601494193751 ) ) ;
#32186 = MANIFOLD_SOLID_BREP ( 'Sweep1', #19408 ) ;
#32187 = CARTESIAN_POINT ( 'NONE',  ( -8.960552108402744065E-16, 78.37500000273116996, -14.63369212191046209 ) ) ;
#32188 = DIRECTION ( 'NONE',  ( -0.000000000000000000, 1.000000000000000000, -0.000000000000000000 ) ) ;
#32189 = CARTESIAN_POINT ( 'NONE',  ( -14.97647472619899389, 40.49701416574269786, 26.02091320914878025 ) ) ;
#32190 = CARTESIAN_POINT ( 'NONE',  ( 4.300734207923761154, 71.97500000273119269, 13.23629886949340495 ) ) ;
#32191 = CARTESIAN_POINT ( 'NONE',  ( -26.00068869287368756, 46.23177083333332149, -15.01150461594595775 ) ) ;
#32192 = CARTESIAN_POINT ( 'NONE',  ( -7.579748464070165821E-14, 10.49999999999999112, -24.50000000000000000 ) ) ;
#32193 = CARTESIAN_POINT ( 'NONE',  ( 32.50000000000000711, 70.90000000000000568, 10.55989012756945122 ) ) ;
#32194 = CARTESIAN_POINT ( 'NONE',  ( -14.01125832528328985, 65.70534749907602645, -24.18731323226223040 ) ) ;
#32195 = CARTESIAN_POINT ( 'NONE',  ( 27.16883889988623935, 42.32500000273120833, -19.73931689729374384 ) ) ;
#32196 = CARTESIAN_POINT ( 'NONE',  ( 15.00000000000000000, 71.25000000546238255, -1.836970198721029589E-15 ) ) ;
#32197 = CARTESIAN_POINT ( 'NONE',  ( -2.162160676586881955E-15, 46.87500000273118417, -35.31076352940723240 ) ) ;
#32198 = CARTESIAN_POINT ( 'NONE',  ( -33.58253175000000113, 33.27500000273120406, -10.91162601494193041 ) ) ;
#32199 = CARTESIAN_POINT ( 'NONE',  ( 9.555238894532166682, 16.99999999999998934, 21.84766023402006141 ) ) ;
#32200 = VECTOR ( 'NONE', #15875, 1000.000000000000000 ) ;
#32201 = CARTESIAN_POINT ( 'NONE',  ( -2.428612866367529427E-13, 22.74218749999999645, -27.95245687107223276 ) ) ;
#32202 = CARTESIAN_POINT ( 'NONE',  ( 6.001560367445586717E-15, 3.249999994537631665, 24.50000000000000000 ) ) ;
#32203 = CARTESIAN_POINT ( 'NONE',  ( 32.50000000000000711, 70.90000000000000568, 10.55989012756945122 ) ) ;
#32204 = CARTESIAN_POINT ( 'NONE',  ( -10.37757302488624411, 10.72500000273117493, -31.93888565452638417 ) ) ;
#32205 = CARTESIAN_POINT ( 'NONE',  ( -23.41746824999999887, 5.624999997268814944, -2.867812753649727150E-15 ) ) ;
#32206 = EDGE_CURVE ( 'NONE', #9681, #9005, #2153, .T. ) ;
#32207 = DIRECTION ( 'NONE',  ( -0.000000000000000000, -1.000000000000000000, -0.000000000000000000 ) ) ;
#32208 = CARTESIAN_POINT ( 'NONE',  ( 26.09010956794244507, 29.18190999907601579, 6.950374756619249084 ) ) ;
#32209 = DIRECTION ( 'NONE',  ( 0.000000000000000000, 0.000000000000000000, -1.000000000000000000 ) ) ;
#32210 = CARTESIAN_POINT ( 'NONE',  ( 10.37757302488624056, 18.52500000273118985, -31.93888565452638417 ) ) ;
#32211 = CARTESIAN_POINT ( 'NONE',  ( 18.94512977948575738, 8.924999997268812990, 13.76444248337723408 ) ) ;
#32212 = CARTESIAN_POINT ( 'NONE',  ( 24.20753774853756113, 51.38802083333332149, 13.97622843553589789 ) ) ;
#32213 = EDGE_CURVE ( 'NONE', #11742, #10580, #8743, .T. ) ;
#32214 = ORIENTED_EDGE ( 'NONE', *, *, #22423, .F. ) ;
#32215 = CARTESIAN_POINT ( 'NONE',  ( -20.75514604977248112, 55.42500000273119554, 28.56700777964554661 ) ) ;
#32216 = EDGE_CURVE ( 'NONE', #9461, #23625, #6168, .T. ) ;
#32217 =( BOUNDED_CURVE ( )  B_SPLINE_CURVE ( 2, ( #14811, #14641, #3997, #28019, #25451, #17734, #25275, #30234, #1748, #6738, #1927, #17220, #22701 ),
 .UNSPECIFIED., .F., .T. ) 
 B_SPLINE_CURVE_WITH_KNOTS ( ( 3, 2, 2, 2, 2, 2, 3 ),
 ( 0.4166666666666666852, 0.4222222222222222210, 0.4333333333333333481, 0.4444444444444444198, 0.4555555555555555469, 0.4666666666666666741, 0.4722222222222222654 ),
 .UNSPECIFIED. ) 
 CURVE ( )  GEOMETRIC_REPRESENTATION_ITEM ( )  RATIONAL_B_SPLINE_CURVE ( ( 0.9755282581475767101, 0.9755282581475768211, 1.000000000000000000, 0.9510565162951535312, 1.000000000000000000, 0.9510565162951535312, 1.000000000000000000, 0.9510565162951535312, 1.000000000000000000, 0.9510565162951535312, 1.000000000000000000, 0.9755282581475765991, 0.9755282581475767101 ) ) 
 REPRESENTATION_ITEM ( '' )  );
#32218 = ORIENTED_EDGE ( 'NONE', *, *, #2527, .F. ) ;
#32219 = CARTESIAN_POINT ( 'NONE',  ( -26.00068869287340334, 25.03385416666666785, 15.01150461594643382 ) ) ;
#32220 = CARTESIAN_POINT ( 'NONE',  ( 25.98046417659858420, 25.32590250092397710, 15.04653450569292872 ) ) ;
#32221 = CARTESIAN_POINT ( 'NONE',  ( -33.58253175000000113, 1.225000002731198467, 10.91162601494193929 ) ) ;
#32222 = EDGE_CURVE ( 'NONE', #27878, #1088, #14239, .T. ) ;
#32223 = CARTESIAN_POINT ( 'NONE',  ( -14.47279130897152122, 7.924999997268803220, 19.92008829642072243 ) ) ;
#32224 = CARTESIAN_POINT ( 'NONE',  ( 10.37757302488624767, 27.97500000273117493, 31.93888565452638417 ) ) ;
#32225 = CARTESIAN_POINT ( 'NONE',  ( 32.50000000000000000, 29.50000000546237899, -3.980102097228898626E-15 ) ) ;
#32226 = CARTESIAN_POINT ( 'NONE',  ( 26.29305231718578995, 69.19999999999998863, -19.10302069950538240 ) ) ;
#32227 = DIRECTION ( 'NONE',  ( -1.000000000000000000, 0.000000000000000000, 0.000000000000000000 ) ) ;
#32228 = CARTESIAN_POINT ( 'NONE',  ( -19.82091636218621389, 11.19999999999998863, 14.40073868116558842 ) ) ;
#32229 = CARTESIAN_POINT ( 'NONE',  ( 7.468012846824777284, 53.25559000092396644, 28.02196122052045268 ) ) ;
#32230 = CARTESIAN_POINT ( 'NONE',  ( -10.37757302488623701, 45.77500000273118985, 31.93888565452638417 ) ) ;
#32231 = CARTESIAN_POINT ( 'NONE',  ( 18.94512977948576093, 13.32499999726882756, -13.76444248337722875 ) ) ;
#32232 = CARTESIAN_POINT ( 'NONE',  ( 6.277390505771533514E-15, 18.49999999999999645, 34.17252228774368916 ) ) ;
#32233 = CARTESIAN_POINT ( 'NONE',  ( 24.50000000000000355, 12.09999999999999787, -7.960532557706203605 ) ) ;
#32234 = CARTESIAN_POINT ( 'NONE',  ( 33.58253175000000823, 62.02500000273116143, 10.91162601494192863 ) ) ;
#32235 = CARTESIAN_POINT ( 'NONE',  ( 20.75514604977249178, 52.07500000273119412, 28.56700777964553950 ) ) ;
#32236 = CARTESIAN_POINT ( 'NONE',  ( -14.47279130897151767, 13.32499999726880624, -19.92008829642072598 ) ) ;
#32237 = LINE ( 'NONE', #10981, #16141 ) ;
#32238 = CARTESIAN_POINT ( 'NONE',  ( 27.16883889988623935, 6.325000002731173687, -19.73931689729374384 ) ) ;
#32239 = CARTESIAN_POINT ( 'NONE',  ( -24.22776226481240514, 36.78423583425730214, 13.94119854578937812 ) ) ;
#32240 = CARTESIAN_POINT ( 'NONE',  ( 11.74590207350062698, 16.99999999999998579, -20.27301895490997197 ) ) ;
#32241 = MANIFOLD_SOLID_BREP ( 'Thread3', #17772 ) ;
#32242 = CARTESIAN_POINT ( 'NONE',  ( -5.147494310547430452, 19.55125428154684641, -32.49999999999999289 ) ) ;
#32243 = CARTESIAN_POINT ( 'NONE',  ( 10.37757302488624056, 30.52500000273118630, -31.93888565452638417 ) ) ;
#32244 = LINE ( 'NONE', #3592, #1223 ) ;
#32245 = CARTESIAN_POINT ( 'NONE',  ( 3.735172737399427541E-15, 70.00000000000000000, 30.50000000000000000 ) ) ;
#32246 =( REPRESENTATION_RELATIONSHIP ('NONE','NONE', #5873, #31529 ) REPRESENTATION_RELATIONSHIP_WITH_TRANSFORMATION ( #28440 )SHAPE_REPRESENTATION_RELATIONSHIP( ) );
#32247 = CARTESIAN_POINT ( 'NONE',  ( -10.04305231718578462, 30.90000000546239178, 30.90933677959249337 ) ) ;
#32248 = CARTESIAN_POINT ( 'NONE',  ( 7.543491769121922985, 53.81732666574268364, 28.00173670424535644 ) ) ;
#32249 = CARTESIAN_POINT ( 'NONE',  ( 26.29305231718578995, 49.70000000546236407, -19.10302069950538240 ) ) ;
#32250 = CARTESIAN_POINT ( 'NONE',  ( 8.998893468610761559, 16.99999999999998579, -21.61938333025141290 ) ) ;
#32251 = CARTESIAN_POINT ( 'NONE',  ( 13.97622843553589966, 29.90364583333332504, -24.20753774853756113 ) ) ;
#32252 = CARTESIAN_POINT ( 'NONE',  ( -20.75514604977248823, 72.82500000273118701, -28.56700777964554305 ) ) ;
#32253 = CARTESIAN_POINT ( 'NONE',  ( -28.01184896238290278, 32.05208333333332860, 7.505752307973363457 ) ) ;
#32254 = LINE ( 'NONE', #4107, #908 ) ;
#32255 = ORIENTED_EDGE ( 'NONE', *, *, #14071, .F. ) ;
#32256 = CARTESIAN_POINT ( 'NONE',  ( 15.04653450569292872, 51.96652750092398065, -25.98046417659857710 ) ) ;
#32257 = CARTESIAN_POINT ( 'NONE',  ( 32.50000000000000711, 9.400000005462366914, 10.55989012756945122 ) ) ;
#32258 = CARTESIAN_POINT ( 'NONE',  ( 7.505752307972854531, 60.69791666666667140, -28.01184896238303423 ) ) ;
#32259 = CARTESIAN_POINT ( 'NONE',  ( 32.50000000000000711, 56.90000000000000568, 10.55989012756945122 ) ) ;
#32260 = CARTESIAN_POINT ( 'NONE',  ( -33.58253175000000113, 47.47500000273119269, 10.91162601494193929 ) ) ;
#32261 = CARTESIAN_POINT ( 'NONE',  ( 32.50000000000000000, 49.50000000546239676, -3.980102097228898626E-15 ) ) ;
#32262 = ADVANCED_FACE ( 'NONE', ( #6005 ), #1342, .F. ) ;
#32263 = CARTESIAN_POINT ( 'NONE',  ( 4.300734207923757602, 78.77500000273118985, -13.23629886949340673 ) ) ;
#32264 = CARTESIAN_POINT ( 'NONE',  ( 10.37757302488624767, 33.72500000273117848, 31.93888565452638417 ) ) ;
#32265 = CARTESIAN_POINT ( 'NONE',  ( 24.50000000000000000, 11.90000000000000213, 7.960532557706212486 ) ) ;
#32266 = CARTESIAN_POINT ( 'NONE',  ( -10.37757302488624411, 62.97500000273120691, -31.93888565452638417 ) ) ;
#32267 = CARTESIAN_POINT ( 'NONE',  ( 32.50000000000000000, 39.00000000000000711, -3.980102097228898626E-15 ) ) ;
#32268 = CARTESIAN_POINT ( 'NONE',  ( -14.47279130897151589, 9.324999997268816898, -19.92008829642072598 ) ) ;
#32269 = CARTESIAN_POINT ( 'NONE',  ( -33.58253175000000113, 3.275000002731191628, -10.91162601494193218 ) ) ;
#32270 = DIRECTION ( 'NONE',  ( -0.000000000000000000, 1.000000000000000000, -0.000000000000000000 ) ) ;
#32271 = CARTESIAN_POINT ( 'NONE',  ( 13.91746824999999532, 78.47500000273120691, -4.522059556121118540 ) ) ;
#32272 = CARTESIAN_POINT ( 'NONE',  ( -27.16883889988623935, 73.57500000273120122, 19.73931689729374739 ) ) ;
#32273 = CARTESIAN_POINT ( 'NONE',  ( -24.50000000000000711, 18.84999999453762953, 7.960532557706201828 ) ) ;
#32274 = CARTESIAN_POINT ( 'NONE',  ( 10.37757302488624056, 70.77500000273118985, -31.93888565452638417 ) ) ;
#32275 = ORIENTED_EDGE ( 'NONE', *, *, #15946, .F. ) ;
#32276 = CARTESIAN_POINT ( 'NONE',  ( -7.570916362186210335, 6.349999994537613546, -23.30088464923126779 ) ) ;
#32277 = CARTESIAN_POINT ( 'NONE',  ( -19.11951029504763611, 16.01600666759064140, 19.06425588902592239 ) ) ;
#32278 = DIRECTION ( 'NONE',  ( 0.000000000000000000, 1.000000000000000000, 0.000000000000000000 ) ) ;
#32279 = CARTESIAN_POINT ( 'NONE',  ( -10.37757302488624411, 48.72500000273120691, -31.93888565452638417 ) ) ;
#32280 = CARTESIAN_POINT ( 'NONE',  ( 10.37757302488624056, 10.77500000273116854, -31.93888565452638417 ) ) ;
#32281 = CARTESIAN_POINT ( 'NONE',  ( 6.486482029760648627E-15, 61.87500000273117706, 35.31076352940722529 ) ) ;
#32282 = CARTESIAN_POINT ( 'NONE',  ( -26.07999730980490583, 52.96354166666666430, -6.988114217767815717 ) ) ;
#32283 = CARTESIAN_POINT ( 'NONE',  ( 20.47846945139902530, 39.21913166759063785, 20.53372385742071771 ) ) ;
#32284 = CARTESIAN_POINT ( 'NONE',  ( 20.47846945139867003, 32.04649333240934084, -20.53372385742107653 ) ) ;
#32285 = CARTESIAN_POINT ( 'NONE',  ( -26.29305231718579350, 68.30000000546236549, -19.10302069950537884 ) ) ;
#32286 = CARTESIAN_POINT ( 'NONE',  ( 8.601468415847516980, 78.17500000273120975, -11.83890561707634781 ) ) ;
#32287 = CARTESIAN_POINT ( 'NONE',  ( -13.94119854578892514, 57.68451416574269075, 24.22776226481266448 ) ) ;
#32288 = CARTESIAN_POINT ( 'NONE',  ( -14.47279130897151589, 15.32499999726880269, -19.92008829642072598 ) ) ;
#32289 = CARTESIAN_POINT ( 'NONE',  ( 32.50000000000000711, 13.40000000546237047, 10.55989012756945122 ) ) ;
#32290 = ORIENTED_EDGE ( 'NONE', *, *, #7128, .F. ) ;
#32291 = CARTESIAN_POINT ( 'NONE',  ( 10.37757302488624767, 47.97500000273117848, 31.93888565452638417 ) ) ;
#32292 = CARTESIAN_POINT ( 'NONE',  ( 0.000000000000000000, 80.00000000000001421, 0.000000000000000000 ) ) ;
#32293 = CARTESIAN_POINT ( 'NONE',  ( -14.01125832528285109, 50.24777750092398065, 24.18731323226248264 ) ) ;
#32294 = CARTESIAN_POINT ( 'NONE',  ( 27.16883889988623935, 66.57500000273120122, -19.73931689729374384 ) ) ;
#32295 = ORIENTED_EDGE ( 'NONE', *, *, #7702, .T. ) ;
#32296 = CARTESIAN_POINT ( 'NONE',  ( 27.16883889988624290, 17.92500000273118843, 19.73931689729373673 ) ) ;
#32297 = CARTESIAN_POINT ( 'NONE',  ( -28.01184896238304134, 25.46354166666666430, -7.505752307972844761 ) ) ;
#32299 = ORIENTED_EDGE ( 'NONE', *, *, #9790, .F. ) ;
#32298 = EDGE_CURVE ( 'NONE', #21770, #16286, #18894, .T. ) ;
#32300 = VERTEX_POINT ( 'NONE', #8578 ) ;
#32301 = CARTESIAN_POINT ( 'NONE',  ( -6.668400408272875007E-16, 2.249999994537632553, -24.50000000000000355 ) ) ;
#32302 = CARTESIAN_POINT ( 'NONE',  ( 27.16883889988623935, 54.32500000273118701, -19.73931689729374384 ) ) ;
#32303 = CARTESIAN_POINT ( 'NONE',  ( -15.01150461594595775, 59.12239583333333570, 26.00068869287368756 ) ) ;
#32304 = EDGE_CURVE ( 'NONE', #28296, #476, #16408, .T. ) ;
#32305 = CARTESIAN_POINT ( 'NONE',  ( 26.29305231718578995, 9.700000005462394270, -19.10302069950538240 ) ) ;
#32306 = DIRECTION ( 'NONE',  ( -0.2583678462756402450, 0.9660466117175128264, 0.000000000000000000 ) ) ;
#32307 = CARTESIAN_POINT ( 'NONE',  ( -14.47279130897152299, 12.42499999726880588, 19.92008829642072243 ) ) ;
#32308 = CARTESIAN_POINT ( 'NONE',  ( -27.16883889988624290, 25.17500000273117777, -19.73931689729374028 ) ) ;
#32309 = CARTESIAN_POINT ( 'NONE',  ( 4.635254915624209993, 77.39999999999999147, -14.26584774442730463 ) ) ;
#32310 = CARTESIAN_POINT ( 'NONE',  ( 26.09010956794244507, 18.86940999907601935, 6.950374756619249084 ) ) ;
#32311 = CYLINDRICAL_SURFACE ( 'NONE', #25384, 16.50000000000002842 ) ;
#32312 = CARTESIAN_POINT ( 'NONE',  ( -24.50000000000000000, -2.000000000000001332, 0.000000000000000000 ) ) ;
#32313 = CARTESIAN_POINT ( 'NONE',  ( -32.50000000000000000, 34.10000000000000142, 10.55989012756946366 ) ) ;
#32314 =( BOUNDED_CURVE ( )  B_SPLINE_CURVE ( 2, ( #10716, #59, #21195, #31638, #8136, #29061, #16047, #27163, #14132, #901, #6057, #13799, #21858 ),
 .UNSPECIFIED., .F., .T. ) 
 B_SPLINE_CURVE_WITH_KNOTS ( ( 3, 2, 2, 2, 2, 2, 3 ),
 ( 0.1474358974358974395, 0.1487179487179487170, 0.1512820512820512719, 0.1538461538461538547, 0.1564102564102564097, 0.1589743589743589647, 0.1602564102564102699 ),
 .UNSPECIFIED. ) 
 CURVE ( )  GEOMETRIC_REPRESENTATION_ITEM ( )  RATIONAL_B_SPLINE_CURVE ( ( 0.9755282581475768211, 0.9755282581475768211, 1.000000000000000000, 0.9510565162951535312, 1.000000000000000000, 0.9510565162951535312, 1.000000000000000000, 0.9510565162951535312, 1.000000000000000000, 0.9510565162951535312, 1.000000000000000000, 0.9755282581475764880, 0.9755282581475768211 ) ) 
 REPRESENTATION_ITEM ( '' )  );
#32315 = CARTESIAN_POINT ( 'NONE',  ( 10.04305231718579705, 10.59999999999998366, 30.90933677959248982 ) ) ;
#32316 = ORIENTED_EDGE ( 'NONE', *, *, #4738, .T. ) ;
#32317 = CARTESIAN_POINT ( 'NONE',  ( 14.47279130897151767, 5.424999997268823648, -19.92008829642072598 ) ) ;
#32318 = CARTESIAN_POINT ( 'NONE',  ( 13.91746825000000065, 77.77500000273117564, 4.522059556121114987 ) ) ;
#32319 = CARTESIAN_POINT ( 'NONE',  ( 26.07999730980477437, 44.08333333333332860, -6.988114217768290004 ) ) ;
#32320 = CARTESIAN_POINT ( 'NONE',  ( 6.486482029760649416E-15, 17.62500000273117351, 35.31076352940723240 ) ) ;
#32321 = CARTESIAN_POINT ( 'NONE',  ( 20.75514604977248467, 68.42500000273120975, -28.56700777964554305 ) ) ;
#32322 = CARTESIAN_POINT ( 'NONE',  ( 27.16883889988623935, 32.57500000273117990, -19.73931689729374384 ) ) ;
#32323 = CARTESIAN_POINT ( 'NONE',  ( 20.75514604977248467, 18.67500000273120264, -28.56700777964554305 ) ) ;
#32324 = CARTESIAN_POINT ( 'NONE',  ( -10.37757302488624411, 6.975000002731185589, -31.93888565452638417 ) ) ;
#32325 = CARTESIAN_POINT ( 'NONE',  ( -15.04653450569291984, 12.43527750092397532, 25.98046417659859486 ) ) ;
#32326 = CARTESIAN_POINT ( 'NONE',  ( 2.740863092043355209E-13, 55.39843749999999289, 30.02300923189239512 ) ) ;
#32327 = CARTESIAN_POINT ( 'NONE',  ( 5.147494310547434893, 59.05125428700924317, 32.49999999999999289 ) ) ;
#32328 = CARTESIAN_POINT ( 'NONE',  ( -13.91746824999999532, 75.27500000273123248, -4.522059556121115875 ) ) ;
#32329 = CARTESIAN_POINT ( 'NONE',  ( -20.08610463437156923, 48.30000000000001847, 27.64615127144130113 ) ) ;
#32330 = FACE_OUTER_BOUND ( 'NONE', #3984, .T. ) ;
#32331 = CARTESIAN_POINT ( 'NONE',  ( 33.58253175000000823, 50.02500000273119696, 10.91162601494192685 ) ) ;
#32332 = CARTESIAN_POINT ( 'NONE',  ( 23.41746824999999887, 17.12499999726882649, 0.000000000000000000 ) ) ;
#32333 = VERTEX_POINT ( 'NONE', #12157 ) ;
#32334 = CARTESIAN_POINT ( 'NONE',  ( -33.58253175000000113, 67.47500000273117848, 10.91162601494193929 ) ) ;
#32335 = CARTESIAN_POINT ( 'NONE',  ( 5.779280353836490358E-15, 62.50000000000000000, 32.49999999999999289 ) ) ;
#32336 = CARTESIAN_POINT ( 'NONE',  ( 23.41746824999999887, 6.624999997268815832, 0.000000000000000000 ) ) ;
#32337 = CARTESIAN_POINT ( 'NONE',  ( 0.04044903254993986036, 24.18006916759064140, -27.95245687107223986 ) ) ;
#32338 = ORIENTED_EDGE ( 'NONE', *, *, #9999, .T. ) ;
#32339 = CARTESIAN_POINT ( 'NONE',  ( -10.37757302488623701, 35.52500000273118985, 31.93888565452638417 ) ) ;
#32340 = CARTESIAN_POINT ( 'NONE',  ( -15.14183272437242778, 1.299999999999988054, 20.84094480462497856 ) ) ;
#32341 = VERTEX_POINT ( 'NONE', #25554 ) ;
#32342 = CARTESIAN_POINT ( 'NONE',  ( 30.02300923189239512, 54.53906249999998579, -2.619432448724977703E-13 ) ) ;
#32343 = CARTESIAN_POINT ( 'NONE',  ( -27.16883889988624290, 61.17500000273118133, -19.73931689729374028 ) ) ;
#32344 = CARTESIAN_POINT ( 'NONE',  ( -8.891200544363830713E-16, 75.75000000546238255, -15.00000000000000000 ) ) ;
#32345 = CARTESIAN_POINT ( 'NONE',  ( 33.58253175000000113, 74.12500000273119838, -4.112674001490185761E-15 ) ) ;
#32346 = CARTESIAN_POINT ( 'NONE',  ( -26.00068869287340334, 28.47135416666666075, 15.01150461594643382 ) ) ;
#32347 = CARTESIAN_POINT ( 'NONE',  ( 19.82091636218621034, 5.799999999999999822, 14.40073868116559730 ) ) ;
#32348 = EDGE_CURVE ( 'NONE', #31380, #15184, #30402, .T. ) ;
#32349 = CYLINDRICAL_SURFACE ( 'NONE', #6195, 24.50000000000000000 ) ;
#32350 = EDGE_CURVE ( 'NONE', #19359, #3811, #30511, .T. ) ;
#32351 = CARTESIAN_POINT ( 'NONE',  ( -10.37757302488624411, 14.72500000273119269, -31.93888565452638417 ) ) ;
#32352 = CARTESIAN_POINT ( 'NONE',  ( 13.91746824999999532, 73.97500000273120691, -4.522059556121118540 ) ) ;
#32353 = CARTESIAN_POINT ( 'NONE',  ( 7.543491769121922985, 46.94232666574269075, 28.00173670424535644 ) ) ;
#32354 = CARTESIAN_POINT ( 'NONE',  ( 15.00000000000000355, 78.89999999999999147, 4.873795443493592394 ) ) ;
#32355 = CARTESIAN_POINT ( 'NONE',  ( -30.02300923189239867, 45.94531249999998579, 2.654126918244514854E-13 ) ) ;
#32356 = CARTESIAN_POINT ( 'NONE',  ( -15.14183272437242067, 10.70000000000001172, -20.84094480462497856 ) ) ;
#32357 = CARTESIAN_POINT ( 'NONE',  ( 32.50000000000000000, 71.00000000000001421, -3.980102097228898626E-15 ) ) ;
#32358 = CARTESIAN_POINT ( 'NONE',  ( 19.09188309203661049, 16.29687499999999645, -19.09188309203694445 ) ) ;
#32359 = CARTESIAN_POINT ( 'NONE',  ( 27.16883889988623935, 44.32500000273117990, -19.73931689729374384 ) ) ;
#32360 = CARTESIAN_POINT ( 'NONE',  ( 11.25946833292375793, 73.67500000273119554, 8.180482586598731842 ) ) ;
#32361 = CARTESIAN_POINT ( 'NONE',  ( 27.16883889988623935, 48.57500000273119412, -19.73931689729374384 ) ) ;
#32362 = CARTESIAN_POINT ( 'NONE',  ( 20.75514604977249178, 26.07500000273119767, 28.56700777964553950 ) ) ;
#32363 = LINE ( 'NONE', #8857, #23488 ) ;
#32364 = CARTESIAN_POINT ( 'NONE',  ( 26.07999730980477437, 20.02083333333332860, -6.988114217768290004 ) ) ;
#32365 = CARTESIAN_POINT ( 'NONE',  ( -15.00000000000000000, 80.25000000546239676, 0.000000000000000000 ) ) ;
#32366 = CARTESIAN_POINT ( 'NONE',  ( -2.165007332552593587E-13, 45.00000000546237544, 32.50000000000000000 ) ) ;
#32367 = CARTESIAN_POINT ( 'NONE',  ( -26.29305231718579350, 69.80000000000001137, -19.10302069950537884 ) ) ;
#32368 = CARTESIAN_POINT ( 'NONE',  ( -27.16883889988624290, 10.92500000273120797, -19.73931689729374028 ) ) ;
#32369 = CARTESIAN_POINT ( 'NONE',  ( -18.94512977948575738, 3.424999997268807217, -13.76444248337723231 ) ) ;
#32370 = DIRECTION ( 'NONE',  ( 0.000000000000000000, -1.000000000000000000, 0.000000000000000000 ) ) ;
#32371 = CARTESIAN_POINT ( 'NONE',  ( 26.06988505166722803, 25.45795166574268364, -7.025853678916862854 ) ) ;
#32372 = CARTESIAN_POINT ( 'NONE',  ( -1.089172066684569321E-14, 76.75000000546238255, 15.00000000000000000 ) ) ;
#32373 = CARTESIAN_POINT ( 'NONE',  ( 10.37757302488624056, 16.52500000273118985, -31.93888565452638417 ) ) ;
#32374 = CARTESIAN_POINT ( 'NONE',  ( 1.507698388325705758E-15, 3.624999997268822938, -24.62258325217400312 ) ) ;
#32375 = CARTESIAN_POINT ( 'NONE',  ( -26.07999730980477437, 56.11458333333332860, 6.988114217768305103 ) ) ;
#32376 = ORIENTED_EDGE ( 'NONE', *, *, #32118, .T. ) ;
#32377 = CARTESIAN_POINT ( 'NONE',  ( -33.58253175000000113, 59.22500000273119269, 10.91162601494193929 ) ) ;
#32378 = CARTESIAN_POINT ( 'NONE',  ( -20.75514604977248112, 29.67500000273119909, 28.56700777964554661 ) ) ;
#32379 = ORIENTED_EDGE ( 'NONE', *, *, #6700, .T. ) ;
#32380 = CARTESIAN_POINT ( 'NONE',  ( 7.505752307972854531, 26.32291666666666075, -28.01184896238303423 ) ) ;
#32381 = CARTESIAN_POINT ( 'NONE',  ( -0.04044903254990864921, 22.46131916759064850, 30.02300923189239867 ) ) ;
#32382 = AXIS2_PLACEMENT_3D ( 'NONE', #11466, #16627, #24509 ) ;
#32383 = CARTESIAN_POINT ( 'NONE',  ( -32.50000000000000000, 10.00000000000000888, 0.000000000000000000 ) ) ;
#32384 = CARTESIAN_POINT ( 'NONE',  ( 7.570916362186213000, 16.14999999453761603, -23.30088464923126423 ) ) ;
#32385 = CARTESIAN_POINT ( 'NONE',  ( -18.94512977948575738, 7.424999997268811214, -13.76444248337723231 ) ) ;
#32386 = CARTESIAN_POINT ( 'NONE',  ( -2.162160676586881955E-15, 28.87500000273119838, -35.31076352940723240 ) ) ;
#32387 = CARTESIAN_POINT ( 'NONE',  ( 10.04305231718578817, 27.90000000546238823, -30.90933677959249337 ) ) ;
#32388 = CARTESIAN_POINT ( 'NONE',  ( -2.092463501923844636E-15, 73.49999999999998579, -34.17252228774368916 ) ) ;
#32389 = CARTESIAN_POINT ( 'NONE',  ( 26.29305231718578995, 47.70000000546237118, -19.10302069950538240 ) ) ;
#32390 = CARTESIAN_POINT ( 'NONE',  ( 4.635254915624209993, 73.40000000000001990, -14.26584774442730463 ) ) ;
#32391 = CARTESIAN_POINT ( 'NONE',  ( 7.468012846824777284, 60.13059000092398065, 28.02196122052045268 ) ) ;
#32392 = CARTESIAN_POINT ( 'NONE',  ( 33.58253175000000113, 40.47500000273118559, -10.91162601494193751 ) ) ;
#32393 = CARTESIAN_POINT ( 'NONE',  ( -18.94512977948576093, 8.324999997268822227, 13.76444248337722698 ) ) ;
#32394 = CARTESIAN_POINT ( 'NONE',  ( 26.29305231718579350, 14.79999999999997939, 19.10302069950537529 ) ) ;
#32395 = VECTOR ( 'NONE', #12893, 1000.000000000000000 ) ;
#32396 = CARTESIAN_POINT ( 'NONE',  ( -7.570916362186210335, 12.59999999999999964, -23.30088464923126779 ) ) ;
#32397 = CARTESIAN_POINT ( 'NONE',  ( -13.94119854578892514, 40.49701416574269786, 24.22776226481266448 ) ) ;
#32398 = CARTESIAN_POINT ( 'NONE',  ( -33.58253175000000113, 63.02500000273118985, -10.91162601494193218 ) ) ;
#32399 = CARTESIAN_POINT ( 'NONE',  ( -33.58253175000000113, 49.47500000273118559, 10.91162601494193929 ) ) ;
#32400 = CARTESIAN_POINT ( 'NONE',  ( -18.94512977948576093, 11.82499999726882578, 13.76444248337722698 ) ) ;
#32401 = CARTESIAN_POINT ( 'NONE',  ( -33.58253175000000113, 7.225000002731182924, 10.91162601494193929 ) ) ;
#32402 = CARTESIAN_POINT ( 'NONE',  ( -7.025853678916393008, 39.79204833425731636, 26.06988505166735592 ) ) ;
#32403 = CARTESIAN_POINT ( 'NONE',  ( 17.11581322672471117, 16.99999999999997868, -16.00041235009445018 ) ) ;
#32404 = CARTESIAN_POINT ( 'NONE',  ( -26.29305231718579350, 19.79999999999998295, -19.10302069950537884 ) ) ;
#32405 = CARTESIAN_POINT ( 'NONE',  ( 33.58253175000000823, 26.02500000273120406, 10.91162601494192863 ) ) ;
#32406 = AXIS2_PLACEMENT_3D ( 'NONE', #18838, #32024, #28064 ) ;
#32408 = AXIS2_PLACEMENT_3D ( 'NONE', #20248, #15265, #4443 ) ;
#32407 = LINE ( 'NONE', #11317, #23183 ) ;
#32409 = CARTESIAN_POINT ( 'NONE',  ( -10.04305231718579172, 58.10000000546239107, -30.90933677959248982 ) ) ;
#32410 = CARTESIAN_POINT ( 'NONE',  ( -30.02300923189239867, 51.38243083240936215, 0.04044903255044988294 ) ) ;
#32411 = CARTESIAN_POINT ( 'NONE',  ( 26.29305231718579350, 47.30000000546237260, 19.10302069950537529 ) ) ;
#32412 = CARTESIAN_POINT ( 'NONE',  ( 32.50000000000000000, 49.09999999999999432, -10.55989012756945833 ) ) ;
#32413 =( BOUNDED_CURVE ( )  B_SPLINE_CURVE ( 2, ( #22536, #6918, #17400, #27864, #21956, #667, #8734, #18884, #32404, #24197, #11155, #32242, #3425 ),
 .UNSPECIFIED., .F., .T. ) 
 B_SPLINE_CURVE_WITH_KNOTS ( ( 3, 2, 2, 2, 2, 2, 3 ),
 ( 0.7628205128205127750, 0.7641025641025640525, 0.7666666666666667185, 0.7692307692307692735, 0.7717948717948718285, 0.7743589743589743835, 0.7756410256410256610 ),
 .UNSPECIFIED. ) 
 CURVE ( )  GEOMETRIC_REPRESENTATION_ITEM ( )  RATIONAL_B_SPLINE_CURVE ( ( 0.9755282581475768211, 0.9755282581475768211, 1.000000000000000000, 0.9510565162951535312, 1.000000000000000000, 0.9510565162951535312, 1.000000000000000000, 0.9510565162951535312, 1.000000000000000000, 0.9510565162951535312, 1.000000000000000000, 0.9755282581475768211, 0.9755282581475768211 ) ) 
 REPRESENTATION_ITEM ( '' )  );
#32414 = FILL_AREA_STYLE_COLOUR ( '', #26584 ) ;
#32415 = CARTESIAN_POINT ( 'NONE',  ( -19.09188309203660694, 28.32812499999999645, 19.09188309203694800 ) ) ;
#32416 = CARTESIAN_POINT ( 'NONE',  ( 10.37757302488624056, 72.52500000273118985, -31.93888565452638417 ) ) ;
#32417 = CARTESIAN_POINT ( 'NONE',  ( -26.00068869287340334, 28.47135416666666075, 15.01150461594643382 ) ) ;
#32418 = DIRECTION ( 'NONE',  ( 0.000000000000000000, 0.000000000000000000, -1.000000000000000000 ) ) ;
#32419 = ORIENTED_EDGE ( 'NONE', *, *, #33984, .T. ) ;
#32420 = CARTESIAN_POINT ( 'NONE',  ( 20.47846945139902530, 46.09413166759064495, 20.53372385742071771 ) ) ;
#32421 = CARTESIAN_POINT ( 'NONE',  ( -26.29305231718578995, 10.70000000546238184, 19.10302069950538595 ) ) ;
#32422 = CARTESIAN_POINT ( 'NONE',  ( 7.505752307972854531, 64.13541666666667140, -28.01184896238303423 ) ) ;
#32423 = CARTESIAN_POINT ( 'NONE',  ( -32.50000000000000000, 64.60000000546239107, 10.55989012756946366 ) ) ;
#32424 = CARTESIAN_POINT ( 'NONE',  ( -27.16883889988623935, 49.57500000273118701, 19.73931689729374739 ) ) ;
#32425 = CARTESIAN_POINT ( 'NONE',  ( 32.50000000000000711, 51.40000000546238823, 10.55989012756945122 ) ) ;
#32426 = EDGE_CURVE ( 'NONE', #1865, #19851, #26910, .T. ) ;
#32427 = CARTESIAN_POINT ( 'NONE',  ( -13.91746824999999532, 75.47500000273116427, 4.522059556121122093 ) ) ;
#32428 = CARTESIAN_POINT ( 'NONE',  ( -27.16883889988624290, 32.92500000273118843, -19.73931689729374028 ) ) ;
#32429 = CARTESIAN_POINT ( 'NONE',  ( 5.147494310547428675, 77.05125428700924317, 32.50000000000000000 ) ) ;
#32430 = CARTESIAN_POINT ( 'NONE',  ( -33.58253175000000113, 61.37500000273119127, 0.000000000000000000 ) ) ;
#32431 = CARTESIAN_POINT ( 'NONE',  ( -20.08610463437156923, 36.29999999999997584, 27.64615127144130113 ) ) ;
#32432 = CARTESIAN_POINT ( 'NONE',  ( 10.04305231718579705, 38.59999999999999432, 30.90933677959248982 ) ) ;
#32433 = CARTESIAN_POINT ( 'NONE',  ( -18.94512977948575738, 13.42499999726881654, -13.76444248337723231 ) ) ;
#32434 = CARTESIAN_POINT ( 'NONE',  ( 10.37757302488624767, 3.975000002731182924, 31.93888565452638417 ) ) ;
#32435 = CARTESIAN_POINT ( 'NONE',  ( -2.815509657234710744E-16, -20.70096189432334555, 0.000000000000000000 ) ) ;
#32436 = CARTESIAN_POINT ( 'NONE',  ( -11.25946833292375793, 79.57500000273121543, 8.180482586598737171 ) ) ;
#32437 = CARTESIAN_POINT ( 'NONE',  ( -33.58253175000000113, 71.37500000273119838, 0.000000000000000000 ) ) ;
#32438 = CARTESIAN_POINT ( 'NONE',  ( 24.50000000000000000, 3.849999994537637082, -7.960532557706203605 ) ) ;
#32439 = CARTESIAN_POINT ( 'NONE',  ( -10.37757302488623701, 69.77500000273118985, 31.93888565452638417 ) ) ;
#32440 = ORIENTED_EDGE ( 'NONE', *, *, #21679, .T. ) ;
#32441 = CARTESIAN_POINT ( 'NONE',  ( -7.570916362186210335, 4.349999994537640191, -23.30088464923126779 ) ) ;
#32442 = CARTESIAN_POINT ( 'NONE',  ( 2.584737979205441561E-13, 65.71093749999997158, 27.95245687107222921 ) ) ;
#32443 = VECTOR ( 'NONE', #12716, 1000.000000000000114 ) ;
#32444 = CARTESIAN_POINT ( 'NONE',  ( -33.58253175000000113, 47.02500000273116854, -10.91162601494193218 ) ) ;
#32445 = CARTESIAN_POINT ( 'NONE',  ( 33.58253175000000113, 10.47500000273118204, -10.91162601494193751 ) ) ;
#32446 = CARTESIAN_POINT ( 'NONE',  ( 27.16883889988624290, 60.17500000273119554, 19.73931689729373673 ) ) ;
#32447 = CARTESIAN_POINT ( 'NONE',  ( 6.988114217768294445, 48.38020833333332860, 26.07999730980477437 ) ) ;
#32448 = CARTESIAN_POINT ( 'NONE',  ( 15.04653450569292872, 41.65402750092398065, -25.98046417659857710 ) ) ;
#32449 = CARTESIAN_POINT ( 'NONE',  ( -7.543491769121917656, 28.03607666574268364, -28.00173670424536354 ) ) ;
#32450 = CARTESIAN_POINT ( 'NONE',  ( -32.50000000000000000, 66.40000000546238823, -10.55989012756945478 ) ) ;
#32451 = CARTESIAN_POINT ( 'NONE',  ( -13.91746824999999532, 80.77500000273118985, -4.522059556121115875 ) ) ;
#32452 = CARTESIAN_POINT ( 'NONE',  ( -24.18731323226221974, 57.97097249907601935, 14.01125832528330406 ) ) ;
#32453 = CARTESIAN_POINT ( 'NONE',  ( -32.50000000000000000, 58.10000000000000142, 10.55989012756946366 ) ) ;
#32454 = CARTESIAN_POINT ( 'NONE',  ( -4.223320258572819786E-15, 17.50000000000000000, 24.50000000000000000 ) ) ;
#32455 = ORIENTED_EDGE ( 'NONE', *, *, #14537, .F. ) ;
#32456 = CARTESIAN_POINT ( 'NONE',  ( 20.75514604977249178, 44.07500000273117990, 28.56700777964553950 ) ) ;
#32457 = CARTESIAN_POINT ( 'NONE',  ( 2.489536152421872915E-14, 75.50000000000001421, -32.49999999999999289 ) ) ;
#32458 = CARTESIAN_POINT ( 'NONE',  ( 10.04305231718578817, 27.90000000546237402, -30.90933677959249337 ) ) ;
#32459 = ORIENTED_EDGE ( 'NONE', *, *, #16924, .F. ) ;
#32460 = CARTESIAN_POINT ( 'NONE',  ( 33.58253175000000823, 16.02500000273119340, 10.91162601494192863 ) ) ;
#32461 = CARTESIAN_POINT ( 'NONE',  ( -2.584737979205441561E-13, 29.61718749999999645, -30.02300923189239512 ) ) ;
#32462 = EDGE_LOOP ( 'NONE', ( #9164, #18426, #33443, #12513 ) ) ;
#32463 = CARTESIAN_POINT ( 'NONE',  ( -7.570916362186210335, 12.34999999453761887, -23.30088464923126779 ) ) ;
#32464 = CARTESIAN_POINT ( 'NONE',  ( -33.58253175000000113, 55.12500000273118417, 0.000000000000000000 ) ) ;
#32465 = CARTESIAN_POINT ( 'NONE',  ( -15.01150461594642138, 56.83072916666665009, -26.00068869287340334 ) ) ;
#32466 = CARTESIAN_POINT ( 'NONE',  ( -2.092463501923844636E-15, 12.00000000546238610, -34.17252228774368916 ) ) ;
#32467 = CARTESIAN_POINT ( 'NONE',  ( 7.313012447739250820E-14, 11.49999999999999112, 24.50000000000000000 ) ) ;
#32468 = CARTESIAN_POINT ( 'NONE',  ( -23.41746824999999887, 18.02499999726880731, -7.608796670333730638 ) ) ;
#32469 = CARTESIAN_POINT ( 'NONE',  ( 32.50000000000000711, 56.90000000000001279, 10.55989012756945122 ) ) ;
#32470 = CARTESIAN_POINT ( 'NONE',  ( 10.37757302488624767, 25.97500000273117493, 31.93888565452638417 ) ) ;
#32471 = CARTESIAN_POINT ( 'NONE',  ( -8.891200544363830713E-16, 77.50000000000001421, -15.00000000000000000 ) ) ;
#32472 = CARTESIAN_POINT ( 'NONE',  ( -0.04044903255042732459, 14.42930583240935505, -27.95245687107223986 ) ) ;
#32473 = CARTESIAN_POINT ( 'NONE',  ( 4.300734207923757602, 74.27500000273118985, -13.23629886949340673 ) ) ;
#32474 = CARTESIAN_POINT ( 'NONE',  ( 32.50000000000000711, 64.89999999999999147, 10.55989012756945122 ) ) ;
#32475 = CARTESIAN_POINT ( 'NONE',  ( 0.000000000000000000, 122.0000000000000000, 0.000000000000000000 ) ) ;
#32476 = CARTESIAN_POINT ( 'NONE',  ( -32.50000000000000000, 9.999999999999994671, 0.000000000000000000 ) ) ;
#32477 = ORIENTED_EDGE ( 'NONE', *, *, #6000, .F. ) ;
#32478 = CARTESIAN_POINT ( 'NONE',  ( -14.47279130897151589, 9.824999997268802687, -19.92008829642072598 ) ) ;
#32479 = CARTESIAN_POINT ( 'NONE',  ( -13.91746824999999532, 76.97500000273119269, 4.522059556121122093 ) ) ;
#32480 = CARTESIAN_POINT ( 'NONE',  ( -26.07999730980490583, 39.21354166666666430, -6.988114217767815717 ) ) ;
#32481 = CARTESIAN_POINT ( 'NONE',  ( 20.75514604977248467, 20.42500000273120619, -28.56700777964554305 ) ) ;
#32482 = CARTESIAN_POINT ( 'NONE',  ( -2.162160676586881955E-15, 64.62500000273121259, -35.31076352940723240 ) ) ;
#32483 = CARTESIAN_POINT ( 'NONE',  ( -20.75514604977248112, 29.67500000273119909, 28.56700777964554661 ) ) ;
#32484 = CARTESIAN_POINT ( 'NONE',  ( -10.37757302488624411, 16.97500000273118204, -31.93888565452638417 ) ) ;
#32485 = CARTESIAN_POINT ( 'NONE',  ( 27.16883889988623935, 6.575000002731201221, -19.73931689729374384 ) ) ;
#32486 = CARTESIAN_POINT ( 'NONE',  ( 0.04044903254992426173, 13.86756916759064318, -30.02300923189239867 ) ) ;
#32487 = CARTESIAN_POINT ( 'NONE',  ( -15.01150461594595775, 55.68489583333332860, 26.00068869287368756 ) ) ;
#32488 = CARTESIAN_POINT ( 'NONE',  ( 19.82091636218621034, 5.799999999999999822, 14.40073868116559730 ) ) ;
#32489 = EDGE_CURVE ( 'NONE', #22185, #13788, #33941, .T. ) ;
#32490 = CARTESIAN_POINT ( 'NONE',  ( 11.25946833292375793, 78.57500000273121543, -8.180482586598735395 ) ) ;
#32491 = VECTOR ( 'NONE', #3639, 1000.000000000000000 ) ;
#32492 = CARTESIAN_POINT ( 'NONE',  ( -26.29305231718578995, 50.20000000000000995, 19.10302069950538595 ) ) ;
#32493 = CARTESIAN_POINT ( 'NONE',  ( -24.50000000000000000, 2.749999994537621895, -3.000384657911015469E-15 ) ) ;
#32494 = CARTESIAN_POINT ( 'NONE',  ( -10.37757302488623701, 53.52500000273118985, 31.93888565452638417 ) ) ;
#32495 = EDGE_CURVE ( 'NONE', #14665, #19251, #6840, .T. ) ;
#32496 = CARTESIAN_POINT ( 'NONE',  ( 7.236395654485760609, 15.52499999726880731, -22.27133577429736633 ) ) ;
#32497 = ORIENTED_EDGE ( 'NONE', *, *, #29282, .F. ) ;
#32498 = CARTESIAN_POINT ( 'NONE',  ( -2.162160676586881955E-15, 62.87500000273120548, -35.31076352940723240 ) ) ;
#32499 = CARTESIAN_POINT ( 'NONE',  ( -7.236395654485763274, 8.024999997268800200, 22.27133577429736633 ) ) ;
#32500 = CARTESIAN_POINT ( 'NONE',  ( 19.06425588902592239, 22.03163166759064495, 19.11951029504763611 ) ) ;
#32501 = EDGE_LOOP ( 'NONE', ( #8549, #9760, #29396, #19848 ) ) ;
#32502 = CARTESIAN_POINT ( 'NONE',  ( 27.16883889988624290, 37.92500000273117422, 19.73931689729373673 ) ) ;
#32503 = CARTESIAN_POINT ( 'NONE',  ( 3.880418787951140036, 6.448745718453147369, -24.49999999999999645 ) ) ;
#32504 = ORIENTED_EDGE ( 'NONE', *, *, #3708, .T. ) ;
#32505 = CARTESIAN_POINT ( 'NONE',  ( -20.50609665440969209, 55.82812499999999289, 20.50609665441005092 ) ) ;
#32506 = CARTESIAN_POINT ( 'NONE',  ( -33.58253175000000113, 63.37500000273119127, 0.000000000000000000 ) ) ;
#32507 = CARTESIAN_POINT ( 'NONE',  ( -10.04305231718578462, 0.9000000054623785717, 30.90933677959249337 ) ) ;
#32508 = CARTESIAN_POINT ( 'NONE',  ( 33.58253175000000113, 72.12500000273119838, -4.112674001490185761E-15 ) ) ;
#32509 = CARTESIAN_POINT ( 'NONE',  ( 28.01184896238304134, 34.05729166666666430, 7.505752307972846538 ) ) ;
#32510 = CARTESIAN_POINT ( 'NONE',  ( -19.82091636218621034, 4.799999999999998934, -14.40073868116559552 ) ) ;
#32511 = CARTESIAN_POINT ( 'NONE',  ( -20.75514604977248112, 3.675000002731179549, 28.56700777964554661 ) ) ;
#32512 = CARTESIAN_POINT ( 'NONE',  ( 20.75514604977248467, 18.42500000273117422, -28.56700777964554305 ) ) ;
#32513 = CARTESIAN_POINT ( 'NONE',  ( 4.300734207923761154, 75.47500000273119269, 13.23629886949340495 ) ) ;
#32514 = CARTESIAN_POINT ( 'NONE',  ( 28.00173670424535644, 42.64545166574268364, -7.543491769121920321 ) ) ;
#32515 = CARTESIAN_POINT ( 'NONE',  ( 4.300734207923757602, 72.77500000273118985, -13.23629886949340673 ) ) ;
#32516 = CARTESIAN_POINT ( 'NONE',  ( -20.50609665440969209, 62.70312500000000000, 20.50609665441005092 ) ) ;
#32517 = VECTOR ( 'NONE', #25715, 1000.000000000000000 ) ;
#32518 = CARTESIAN_POINT ( 'NONE',  ( 4.445600272181915325E-13, 27.50000000000000355, -32.50000000000000000 ) ) ;
#32519 = CARTESIAN_POINT ( 'NONE',  ( -7.570916362186215665, 9.149999994537639125, 23.30088464923126423 ) ) ;
#32520 = CARTESIAN_POINT ( 'NONE',  ( 20.08610463437157279, 49.80000000546238681, -27.64615127144129758 ) ) ;
#32521 = CARTESIAN_POINT ( 'NONE',  ( -19.09188309203694445, 15.43749999999999645, -19.09188309203661049 ) ) ;
#32522 = CARTESIAN_POINT ( 'NONE',  ( 27.16883889988624290, 39.92500000273119554, 19.73931689729373673 ) ) ;
#32523 = CARTESIAN_POINT ( 'NONE',  ( 11.25946833292375793, 74.07500000273120122, -8.180482586598735395 ) ) ;
#32524 = CARTESIAN_POINT ( 'NONE',  ( -10.37757302488623701, 51.77500000273120406, 31.93888565452638417 ) ) ;
#32525 = CARTESIAN_POINT ( 'NONE',  ( -20.75514604977248823, 29.07500000273119056, -28.56700777964554305 ) ) ;
#32526 = CARTESIAN_POINT ( 'NONE',  ( -14.24229347433699289, 16.99999999999998934, 19.84889707891977650 ) ) ;
#32527 = CARTESIAN_POINT ( 'NONE',  ( -13.97622843553588901, 35.05989583333332860, 24.20753774853756823 ) ) ;
#32528 = CARTESIAN_POINT ( 'NONE',  ( -10.04305231718579172, 8.100000005462376862, -30.90933677959248982 ) ) ;
#32529 = EDGE_CURVE ( 'NONE', #4234, #6801, #141, .T. ) ;
#32530 = CARTESIAN_POINT ( 'NONE',  ( -32.50000000000000000, 44.60000000546237686, 10.55989012756946366 ) ) ;
#32531 = CARTESIAN_POINT ( 'NONE',  ( -20.08610463437157989, 67.70000000000000284, -27.64615127144129758 ) ) ;
#32532 = CARTESIAN_POINT ( 'NONE',  ( 27.16883889988623935, 10.32500000273119056, -19.73931689729374384 ) ) ;
#32533 = CARTESIAN_POINT ( 'NONE',  ( -7.236395654485757944, 13.22499999726881015, -22.27133577429736988 ) ) ;
#32534 = CARTESIAN_POINT ( 'NONE',  ( 28.02196122052058413, 29.18190999907601579, 7.468012846824272799 ) ) ;
#32535 = CARTESIAN_POINT ( 'NONE',  ( 5.779280353836490358E-15, 23.00000000546237899, 32.49999999999999289 ) ) ;
#32536 = CARTESIAN_POINT ( 'NONE',  ( -26.06988505166722803, 30.61420166574267654, 7.025853678916877953 ) ) ;
#32537 = CARTESIAN_POINT ( 'NONE',  ( -5.147494310547430452, 65.55125428154684641, -32.49999999999999289 ) ) ;
#32538 = CARTESIAN_POINT ( 'NONE',  ( 27.16883889988623935, 12.32500000273117990, -19.73931689729374384 ) ) ;
#32539 = CARTESIAN_POINT ( 'NONE',  ( 14.47279130897151767, 7.424999997268820096, -19.92008829642072598 ) ) ;
#32540 = AXIS2_PLACEMENT_3D ( 'NONE', #5723, #13274, #2471 ) ;
#32541 = CARTESIAN_POINT ( 'NONE',  ( 19.09188309203661049, 50.67187500000000000, -19.09188309203694445 ) ) ;
#32542 = ORIENTED_EDGE ( 'NONE', *, *, #23533, .T. ) ;
#32543 = CARTESIAN_POINT ( 'NONE',  ( -27.16883889988624290, 54.92500000273118843, -19.73931689729374028 ) ) ;
#32544 = CARTESIAN_POINT ( 'NONE',  ( -2.162160676586881955E-15, 26.87500000273116996, -35.31076352940723240 ) ) ;
#32545 = ORIENTED_EDGE ( 'NONE', *, *, #3089, .F. ) ;
#32546 = CARTESIAN_POINT ( 'NONE',  ( -7.505752307972844761, 28.04166666666666075, 28.01184896238304134 ) ) ;
#32547 = CARTESIAN_POINT ( 'NONE',  ( -7.468012846824771955, 27.47434000092397000, -28.02196122052045624 ) ) ;
#32548 = CARTESIAN_POINT ( 'NONE',  ( -32.50000000000000000, 10.10000000000000142, 10.55989012756946366 ) ) ;
#32549 = CARTESIAN_POINT ( 'NONE',  ( -19.82091636218621389, 18.94999999453761319, 14.40073868116558842 ) ) ;
#32550 = CARTESIAN_POINT ( 'NONE',  ( -18.94512977948576093, 3.824999997268818674, 13.76444248337722698 ) ) ;
#32551 = CARTESIAN_POINT ( 'NONE',  ( -33.58253175000000113, 23.27500000273116854, -10.91162601494193218 ) ) ;
#32552 = CARTESIAN_POINT ( 'NONE',  ( 20.08610463437157279, 31.80000000546237260, -27.64615127144129758 ) ) ;
#32553 = CARTESIAN_POINT ( 'NONE',  ( 26.29305231718579350, 70.79999999999999716, 19.10302069950537529 ) ) ;
#32554 = CARTESIAN_POINT ( 'NONE',  ( -32.50000000000000000, 6.500000005462358565, 0.000000000000000000 ) ) ;
#32555 = DIRECTION ( 'NONE',  ( -0.000000000000000000, -1.000000000000000000, -0.000000000000000000 ) ) ;
#32556 = CARTESIAN_POINT ( 'NONE',  ( -0.04044903254990864921, 53.39881916759064495, 30.02300923189239867 ) ) ;
#32557 = CARTESIAN_POINT ( 'NONE',  ( -27.16883889988623935, 35.57500000273120122, 19.73931689729374739 ) ) ;
#32558 = CARTESIAN_POINT ( 'NONE',  ( 6.486482029760648627E-15, 53.62500000273120548, 35.31076352940722529 ) ) ;
#32559 = CARTESIAN_POINT ( 'NONE',  ( -28.01184896238304134, 18.58854166666666430, -7.505752307972844761 ) ) ;
#32560 = CARTESIAN_POINT ( 'NONE',  ( 14.47279130897151767, 13.42499999726880411, -19.92008829642072598 ) ) ;
#32561 = CARTESIAN_POINT ( 'NONE',  ( -32.50000000000000000, 11.90000000000000391, -10.55989012756945478 ) ) ;
#32562 = CARTESIAN_POINT ( 'NONE',  ( -19.82091636218621034, 12.80000000000000604, -14.40073868116559552 ) ) ;
#32563 = CARTESIAN_POINT ( 'NONE',  ( -0.04044903255042732459, 45.36680583240934794, -27.95245687107223986 ) ) ;
#32564 = CARTESIAN_POINT ( 'NONE',  ( 20.75514604977249178, 59.82500000273117280, 28.56700777964553950 ) ) ;
#32565 = CARTESIAN_POINT ( 'NONE',  ( -10.37757302488624411, 48.97500000273119269, -31.93888565452638417 ) ) ;
#32566 = CARTESIAN_POINT ( 'NONE',  ( 7.236395654485755280, 10.22499999726880837, 22.27133577429736988 ) ) ;
#32567 = CARTESIAN_POINT ( 'NONE',  ( -1.778240108872766143E-15, 68.00000000546238255, -32.49999999999999289 ) ) ;
#32568 = CARTESIAN_POINT ( 'NONE',  ( -10.37757302488624411, 4.725000002731183812, -31.93888565452638417 ) ) ;
#32569 = CARTESIAN_POINT ( 'NONE',  ( 6.950374756619721595, 42.94309000092397355, 26.09010956794232428 ) ) ;
#32570 = CARTESIAN_POINT ( 'NONE',  ( 32.50000000000000711, 25.40000000546237047, 10.55989012756945122 ) ) ;
#32571 = CARTESIAN_POINT ( 'NONE',  ( -32.46022989551241977, 52.00000000000002842, 2.703243202363978526 ) ) ;
#32572 = UNCERTAINTY_MEASURE_WITH_UNIT (LENGTH_MEASURE( 1.000000000000000082E-05 ), #7800, 'distance_accuracy_value', 'NONE');
#32573 = CARTESIAN_POINT ( 'NONE',  ( -20.75514604977248112, 25.42500000273119198, 28.56700777964554661 ) ) ;
#32574 = DIRECTION ( 'NONE',  ( -1.224646799147353454E-16, 1.000000000000000000, -0.000000000000000000 ) ) ;
#32575 = LINE ( 'NONE', #16316, #26521 ) ;
#32576 = CARTESIAN_POINT ( 'NONE',  ( -32.50000000000000000, 30.60000000546238041, 10.55989012756946366 ) ) ;
#32577 = CARTESIAN_POINT ( 'NONE',  ( -7.543491769121917656, 58.97357666574269786, -28.00173670424536354 ) ) ;
#32578 = CARTESIAN_POINT ( 'NONE',  ( 32.50000000000000711, 47.40000000546237402, 10.55989012756945122 ) ) ;
#32579 = CARTESIAN_POINT ( 'NONE',  ( -33.58253175000000113, 39.12500000273119838, 0.000000000000000000 ) ) ;
#32580 = CARTESIAN_POINT ( 'NONE',  ( 27.95245687107222921, 27.03906250000000000, -2.463307335887066074E-13 ) ) ;
#32581 = ORIENTED_EDGE ( 'NONE', *, *, #16639, .F. ) ;
#32582 = CARTESIAN_POINT ( 'NONE',  ( 20.75514604977249178, 77.82500000273120122, 28.56700777964553950 ) ) ;
#32583 = CARTESIAN_POINT ( 'NONE',  ( -7.505752307973343918, 32.91145833333332860, -28.01184896238290989 ) ) ;
#32584 = VECTOR ( 'NONE', #21635, 1000.000000000000000 ) ;
#32585 = DIRECTION ( 'NONE',  ( 0.000000000000000000, -0.000000000000000000, -1.000000000000000000 ) ) ;
#32586 = ORIENTED_EDGE ( 'NONE', *, *, #22144, .T. ) ;
#32587 = CARTESIAN_POINT ( 'NONE',  ( -26.02091320914849959, 53.97173583425732346, 14.97647472619947528 ) ) ;
#32588 = CARTESIAN_POINT ( 'NONE',  ( -2.092463501923844636E-15, 12.00000000546237189, -34.17252228774368916 ) ) ;
#32589 = CARTESIAN_POINT ( 'NONE',  ( -20.50609665441004736, 63.56249999999999289, -20.50609665440969565 ) ) ;
#32590 = CARTESIAN_POINT ( 'NONE',  ( 32.50000000000000000, 20.99999999999998934, -3.980102097228898626E-15 ) ) ;
#32591 = CARTESIAN_POINT ( 'NONE',  ( -33.58253175000000113, 43.27500000273117564, -10.91162601494193218 ) ) ;
#32592 = CARTESIAN_POINT ( 'NONE',  ( 26.29305231718579350, 51.30000000546236549, 19.10302069950537529 ) ) ;
#32593 = CARTESIAN_POINT ( 'NONE',  ( -13.91746824999999532, 73.47500000273117848, 4.522059556121122093 ) ) ;
#32594 = CARTESIAN_POINT ( 'NONE',  ( 27.16883889988624290, 31.92500000273118488, 19.73931689729373673 ) ) ;
#32595 = CARTESIAN_POINT ( 'NONE',  ( 10.04305231718578817, 77.90000000546237402, -30.90933677959249337 ) ) ;
#32596 = CARTESIAN_POINT ( 'NONE',  ( 33.58253175000000823, 56.27500000273116854, 10.91162601494192863 ) ) ;
#32597 = CARTESIAN_POINT ( 'NONE',  ( 32.50000000000000711, 36.89999999999999858, 10.55989012756945122 ) ) ;
#32598 = CARTESIAN_POINT ( 'NONE',  ( -2.092463501923844636E-15, 33.50000000000001421, -34.17252228774368916 ) ) ;
#32599 = CARTESIAN_POINT ( 'NONE',  ( -18.94512977948575738, 11.42499999726881477, -13.76444248337723231 ) ) ;
#32600 = CARTESIAN_POINT ( 'NONE',  ( -33.58253175000000113, 7.275000002731181858, -10.91162601494193218 ) ) ;
#32601 = AXIS2_PLACEMENT_3D ( 'NONE', #26051, #10607, #12840 ) ;
#32602 = CARTESIAN_POINT ( 'NONE',  ( -4.934616302121927505E-14, 71.00000000546238255, 32.50000000000000000 ) ) ;
#32603 = CARTESIAN_POINT ( 'NONE',  ( 13.91746824999999532, 76.47500000273120691, -4.522059556121118540 ) ) ;
#32604 = CARTESIAN_POINT ( 'NONE',  ( 27.16883889988623935, 64.57500000273120122, -19.73931689729374384 ) ) ;
#32605 = CARTESIAN_POINT ( 'NONE',  ( -19.82091636218621034, 4.799999999999998934, -14.40073868116559552 ) ) ;
#32606 = ORIENTED_EDGE ( 'NONE', *, *, #33839, .T. ) ;
#32607 = CARTESIAN_POINT ( 'NONE',  ( -15.14183272437241889, 2.449999994537622960, -20.84094480462497856 ) ) ;
#32608 = VECTOR ( 'NONE', #16087, 1000.000000000000000 ) ;
#32609 = CARTESIAN_POINT ( 'NONE',  ( 6.950374756619721595, 12.00559000092397532, 26.09010956794232428 ) ) ;
#32610 =( BOUNDED_SURFACE ( )  B_SPLINE_SURFACE ( 1, 2, ( 
 ( #28936, #23463, #2696, #2861, #12818, #23291, #33759, #10251, #8171, #29100, #20732, #31172, #7664, #28769, #33925, #10415, #18323, #98, #24464, #3697, #3530, #21895, #19655, #32675, #605, #9171, #5939, #32181, #18994, #29438, #16748, #26872, #16420, #11420, #3367, #27374, #13837, #5773, #16253, #940, #11260, #14170, #11583, #19158, #11097, #21736, #26709, #3206, #13674, #24791, #32345, #3863, #16913, #14335, #9009, #24627, #1270, #24304, #19489, #29938, #21566, #11750, #8839, #29597, #1100, #19322, #32011, #29764, #6442, #22064, #32508, #6099, #22230, #24138, #8506, #778, #16580, #8676, #27035, #14002, #6271, #27206, #1444, #25132, #9332, #22735, #17763, #12258, #9513, #4709, #4540, #1609, #4200, #2132, #9688, #15013, #20169, #27884, #4367, #22555, #30787, #14503, #27711, #14672, #12607, #6940, #23076, #30612, #33008, #25653, #7108, #19818, #12087, #30270, #17251, #24961, #19994, #11921, #17423, #7280, #22392, #30442, #28222, #14842, #32841, #15189, #28052, #6770, #25308, #33185, #17590, #1780, #25484, #1963, #20337, #12437, #22907, #33364, #33537, #9860, #10040, #30097, #6604, #17081, #27541, #4028, #26499, #23424, #29059, #20694, #23761, #18452, #2308, #5564, #31301, #8134, #13464, #23592, #23254, #15873, #33885, #15537, #5397, #10377, #2656, #15364, #26330, #2483, #2818, #25818, #7627, #20855, #226, #28894, #18623, #31136, #10714, #21193, #12781, #16044, #13118, #7794, #13286, #15707, #33717, #57, #31635, #2992, #23931, #18284, #399, #20516, #10214, #30962, #28729, #7460, #17943, #18107, #28393, #28556, #5053, #25989, #12951, #10545, #4882, #21024, #5225, #26163, #31474, #7966, #18953, #16870, #24421, #29720, #898, #8632, #19116, #3326, #11537, #29229, #8464, #29398, #27332, #21691, #3819, #11380, #13796, #6394, #21855, #566, #5898, #11057, #31970, #5734, #24264, #16214, #32137, #22020, #26667, #16377, #32464, #11217, #3163, #8965, #8795, #13634, #29554, #26990, #32302, #26830, #732, #6054, #1057, #19278, #16538, #3489, #19447, #6226, #13958, #16705, #27160, #14129, #3652, #24098, #14292, #24585, #29893, #21522, #24749, #10885, #21360, #31803, #8294, #18785, #28180, #4324, #3986, #30570, #14629, #30225, #20126, #25087, #17377, #30057, #7067, #17207, #17550, #6562, #22350, #1566, #17037, #27666, #22188, #32635, #1225, #20295, #6896, #22862, #12392, #33320, #30743, #28009, #4495, #11877, #1915, #32797, #11705, #6725, #12042, #27497, #9129, #9290, #32964, #19775, #25439, #14459, #25263, #22513, #1737, #9818, #22690, #7234, #4156, #19611, #27840, #24916, #9467, #14798, #17722, #4667, #1401, #15147, #14971, #19949, #30395, #33140, #12217, #9644, #12737, #17899, #20981, #5184, #10339, #23551, #23381, #7753, #5522, #18579, #20468, #29020, #25777, #18065, #4838, #15319, #2614, #23208, #2263, #31259, #33670, #13243, #10167, #25611, #2091, #20815, #31091, #14, #31430, #5008, #20651, #18240, #28352, #15833, #30920, #7588, #33844, #183, #7923, #28686, #28513, #23717, #15491, #15667, #10672, #26117, #12565, #18408, #25945, #28854, #2439, #10502, #33494, #12907, #13077, #5352, #26289, #23036, #2778, #21151, #31592, #8092, #9995, #7413, #8756, #8252, #32096, #8924, #24221, #19240, #26457, #21320, #13919, #24056, #2948, #26949, #18745, #13420, #692, #10842, #3449, #31761, #29187, #16665, #859, #1017, #26791, #27122, #11011, #5692, #3615, #524, #29855, #16001, #11178, #21481, #24386, #21815, #29356, #31928, #21649, #16170, #6183, #26626, #3121, #8591, #24546, #11339, #19076, #8420, #14089, #13592, #29515, #11500, #6019, #19407, #32264, #18910, #29678, #5857, #21979, #23887, #16335, #16495, #32428, #358, #3283, #13751, #19908, #27971, #17000, #22316, #25222, #33101, #32594, #22476, #33280, #14591, #9604, #16835, #11669, #4285, #14423, #27290, #17338, #9093, #3782, #25050, #1187, #27801, #22150, #19575, #7027, #1700, #25397, #17172, #17510, #1359, #30023, #1874, #12177, #22648, #27457, #4454, #3948, #6356, #11838, #6688, #6527, #14253, #24877, #4117, #32761, #30530, #9255, #30357, #27629, #6859, #14931, #14759, #12352, #19740, #24710, #32924, #30185, #1531, #12005, #22821, #9776, #9423, #20258, #20086, #23512, #16257, #28643, #28141, #10127, #17857, #22994, #26079, #10300, #15450, #5140, #28477, #12867, #11101, #24142, #25571, #610, #30876, #23166, #9952, #20427, #7714, #28309, #7373, #2399, #4797, #15276, #31391, #25737, #30702, #2217, #31054, #2051, #7198, #12696, #4973, #33628, #20942, #33453, #20777, #7546, #31221, #5777, #18201, #18371, #20609, #15106, #23345, #18031, #25905, #33806, #3210, #26714, #4627, #28816, #33970, #10464, #13678, #15628, #12526, #2575, #13041, #7881, #17679, #1104, #6276, #19494, #19326, #3702, #1448, #14507, #16424, #24966, #21740, #14006, #782, #11264, #32512, #8680, #32185, #27210, #19164, #9175, #29601, #21570, #32015, #16752, #27040, #29942, #27378, #944, #6103, #14174, #24308, #11754, #26876, #16584, #29768, #30102, #16918, #24631, #24469, #19659, #3534, #11589, #6608, #22068, #8511, #3867, #11424, #14339, #21899, #6446, #29442, #32351, #9013, #24796, #1274, #18998, #22235, #32680, #17085, #8843, #27545, #4032, #5945, #13842, #3371, #4886, #20173, #15194, #22396, #17255, #9864, #19998, #32845, #22912, #4204, #9337, #30616, #6774, #33368, #27716, #14676, #12611, #30791, #30967, #22739, #23080, #6944, #25137, #7465, #17768, #28227, #20341, #30446, #4372, #9517, #2136, #1967, #17427, #12262, #10044, #7284, #33189, #27888, #12442, #25657, #17594, #1613, #17948, #14846, #20521, #12091, #33541, #4713, #22560, #28397, #9692, #15368, #25823, #15018, #33012, #11927, #25312, #1785, #19822, #7112, #28056, #4544, #30274, #25488, #26334, #20698, #25993, #18288, #31140, #10381, #12785, #23258, #2312, #26504, #21029, #29063, #5568, #16050, #21197, #2823, #2997, #12955, #31640, #8138, #28561, #13470, #31479, #5229, #23765, #10548, #15541, #7970, #18627, #232, #10718, #15712, #33721, #10219, #2487, #7631, #23596, #18112, #5057, #28733, #23430, #26168, #2661, #18456, #13121, #33889, #20859, #31306, #13291, #7799, #61, #28899, #5401, #15877, #12554, #17887, #23025, #30731, #7224 ),
 ( #12894, #25932, #27828, #2426, #33127, #25426, #12205, #22676, #9982, #28340, #9807, #4484, #33480, #2249, #4656, #1725, #4996, #1904, #7574, #9631, #12723, #30907, #14786, #18054, #20283, #20636, #32952, #2079, #20113, #4825, #12381, #27997, #15305, #22850, #15136, #4311, #25764, #14960, #23194, #25250, #30558, #33308, #7054, #17710, #19936, #30383, #9454, #28499, #25600, #31079, #10154, #15479, #33656, #7401, #6884, #17537, #17365, #28168, #20456, #10999, #15989, #2765, #18733, #18565, #15654, #26445, #26612, #29175, #5680, #13229, #3110, #8240, #18228, #31916, #23704, #24044, #513, #28674, #29344, #26104, #5169, #18395, #2602, #2936, #21470, #5508, #170, #8409, #31748, #28841, #31418, #5845, #13406, #16158, #23875, #21139, #31580, #15821, #18897, #7739, #20967, #7911, #16324, #10660, #26780, #345, #26275, #3271, #10829, #13063, #5339, #23539, #10490, #33989, #8080, #29008, #21308, #23369, #13582, #33830, #10327, #20803, #31247, #1912, #12214, #7410, #14795, #1734, #25259, #20292, #22687, #2260, #33137, #28509, #14626, #33316, #20123, #20648, #28177, #33490, #4664, #12389, #22858, #7064, #15315, #32961, #9640, #30567, #31089, #25436, #7586, #15144, #17547, #10164, #25608, #4321, #28006, #4492, #14968, #9463, #9815, #19946, #30740, #25774, #30391, #7232, #12734, #17718, #6893, #23205, #25084, #2087, #23033, #12562, #9992, #20465, #30916, #17896, #4835, #28349, #33667, #18064, #1563, #12039, #22509, #17374, #27837, #8250, #10670, #7749, #11009, #7921, #13590, #5182, #18743, #2946, #20813, #24054, #15831, #26623, #31926, #8090, #18238, #356, #18406, #11, #23885, #28851, #21149, #33842, #10840, #20978, #21317, #10337, #26114, #5350, #31257, #31428, #25943, #2437, #5006, #522, #31591, #3119, #16168, #21479, #29185, #13417, #8418, #15665, #5690, #18907, #28684, #15489, #18577, #26287, #31759, #180, #2612, #29018, #12904, #23379, #13075, #2776, #23549, #10500, #13240, #23714, #5520, #15999, #26455, #690, #1357, #32093, #11176, #24384, #8589, #21977, #16997, #11498, #8754, #3946, #3780, #857, #3447, #11337, #11666, #6017, #14251, #3281, #13917, #32425, #32592, #29853, #26789, #1185, #8922, #27455, #16492, #21813, #24708, #22148, #21647, #19405, #22314, #3613, #9091, #5854, #19073, #27288, #32261, #16333, #6354, #29513, #13748, #14086, #24219, #16833, #26947, #19238, #30021, #19573, #14421, #6181, #6525, #29676, #16663, #24874, #11836, #32759, #27120, #9253, #24544, #29354, #1015, #20084, #14588, #19738, #27799, #17507, #6857, #9949, #22474, #9773, #30527, #20256, #28307, #7196, #7370, #4283, #4114, #12350, #32922, #9602, #25395, #25735, #4795, #17170, #17854, #12524, #22992, #15274, #17677, #27627, #33099, #17335, #12003, #15104, #33278, #4452, #28139, #27969, #1872, #33625, #12693, #25048, #23162, #19906, #7025, #14757, #33451, #30355, #25220, #1698, #22819, #12174, #2214, #22646, #30183, #6686, #14929, #30699, #4625, #25569, #2049, #20425, #30874, #9421, #1529, #4969, #10297, #18368, #18706, #5480, #5310, #2570, #8213, #33804, #2736, #31722, #15791, #3080, #15959, #23676, #13038, #5648, #21109, #20774, #5137, #31218, #7711, #15447, #23509, #28474, #31388, #21281, #25902, #18198, #29144, #10461, #2395, #16130, #24013, #28641, #18536, #15624, #31552, #26075, #33967, #20939, #313, #140, #7878, #28812, #26585, #28981, #26248, #13199, #10631, #13377, #8050, #12864, #13550, #26415, #10124, #2909, #23849, #10801, #23341, #20605, #31051, #7543, #18028, #3573, #3244, #29811, #13880, #29476, #19368, #24347, #16624, #29313, #6313, #16457, #16790, #5816, #21608, #819, #16293, #26909, #21441, #31885, #485, #19530, #6139, #22107, #11624, #32552, #3741, #8882, #9051, #649, #14212, #24668, #26751, #29980, #27078, #11299, #27248, #29636, #13712, #14044, #1142, #6485, #16957, #21778, #27416, #3906, #24178, #14375, #32225, #10967, #8381, #11139, #18866, #32053, #8552, #5980, #19037, #24505, #3408, #979, #8714, #19197, #11463, #21937, #32387, #30830, #4409, #9728, #14886, #22600, #33054, #17291, #25527, #9212, #22432, #32879, #7324, #1653, #17808, #17125, #6983, #28266, #9559, #28094, #1312, #30141, #22777, #9378, #11795, #1827, #27582, #22273, #20037, #19695, #12305, #6645, #4071, #2004, #20214, #9904, #12128, #12479, #19859, #14546, #20381, #30654, #7151, #1487, #22949, #30314, #24834, #6811, #25174, #25005, #32715, #27753, #30482, #11961, #15060, #4241, #25347, #17466, #33229, #33407, #17633, #4752, #14715, #27926, #4583, #28434, #5096, #21362, #21693, #24266, #12646, #13798, #8467, #18955, #734, #13636, #23117, #28597, #2349, #7502, #11059, #29231, #402, #24100, #13467, #31805, #29556, #8635, #10079, #19119, #15404, #2994, #12824, #29400, #25860, #23295, #33763, #8296, #10255, #3328, #20736, #15229, #25692, #10888, #31178, #568, #21524, #16046, #7668, #18787, #17986, #5902, #20560, #18155, #23933, #11219, #31972, #5736, #26501, #32139, #4924, #16216, #2173, #26670, #33580, #16379, #3166, #26832, #31005, #24918, #13960, #14131, #22190, #9292, #6565, #3491, #11879, #19613, #27669, #16707, #22022, #1403, #32799, #6727, #1059, #900, #25090, #22352, #19777, #27162, #17211, #3654, #6056, #11540, #6396, #11382, #16540, #24587, #3821, #32466, #30227, #8797, #30059, #16872, #17039, #14632, #27499, #4159, #8967, #24423, #32637, #19280, #29895, #11707, #12046, #1569, #21857, #22516, #32967, #9470, #19952, #3989, #32305, #19449, #27335, #29722, #26992, #14462, #24752, #6228, #14294, #9131, #1227, #23385, #25266, #33847, #30572, #17724, #28011, #23211, #7069, #17552, #4497, #2094, #14973, #18068, #25442, #10342, #30399, #15149, #1917, #4841, #2267, #9820, #12394, #25613, #33142, #20654, #1739, #22865, #4669, #5012, #25779, #12567, #33322, #28517, #20128, #23038, #15494, #33496, #6899, #12740, #20297, #33673, #30746, #15323, #4327, #7236, #9998, #10171, #30923, #27844, #31094, #20471, #25948, #28182, #7416, #7591, #2442, #22692, #17902, #17380, #28355, #12910, #14801, #12218, #9648, #28857, #31262, #31763, #13080, #7757, #5525, #15670, #8256, #2617, #26120, #21484, #5695, #5860, #31595, #8423, #2951, #186, #29359 ) ),
 .UNSPECIFIED., .F., .F., .T. ) 
 B_SPLINE_SURFACE_WITH_KNOTS ( ( 2, 2 ),
 ( 3, 2, 2, 2, 2, 2, 2, 2, 2, 2, 2, 2, 2, 2, 2, 2, 2, 2, 2, 2, 2, 2, 2, 2, 2, 2, 2, 2, 2, 2, 2, 2, 2, 2, 2, 2, 2, 2, 2, 2, 2, 2, 2, 2, 2, 2, 2, 2, 2, 2, 2, 2, 2, 2, 2, 2, 2, 2, 2, 2, 2, 2, 2, 2, 2, 2, 2, 2, 2, 2, 2, 2, 2, 2, 2, 2, 2, 2, 2, 2, 2, 2, 2, 2, 2, 2, 2, 2, 2, 2, 2, 2, 2, 2, 2, 2, 2, 2, 2, 2, 2, 2, 2, 2, 2, 2, 2, 2, 2, 2, 2, 2, 2, 2, 2, 2, 2, 2, 2, 2, 2, 2, 2, 2, 2, 2, 2, 2, 2, 2, 2, 2, 2, 2, 2, 2, 2, 2, 2, 2, 2, 2, 2, 2, 2, 2, 2, 2, 2, 2, 2, 2, 2, 2, 2, 2, 2, 2, 2, 2, 2, 2, 2, 2, 2, 2, 2, 2, 2, 2, 2, 2, 2, 2, 2, 2, 2, 2, 2, 2, 2, 2, 2, 2, 2, 2, 2, 2, 2, 2, 2, 2, 2, 2, 2, 2, 2, 2, 2, 2, 2, 2, 2, 2, 2, 2, 2, 2, 2, 2, 2, 2, 2, 2, 2, 2, 2, 2, 2, 2, 2, 2, 2, 2, 2, 2, 2, 2, 2, 2, 2, 2, 2, 2, 2, 2, 2, 2, 2, 2, 2, 2, 2, 2, 2, 2, 2, 2, 2, 2, 2, 2, 2, 2, 2, 2, 2, 2, 2, 2, 2, 2, 2, 2, 2, 2, 2, 2, 2, 2, 2, 2, 2, 2, 2, 2, 2, 2, 2, 2, 2, 2, 2, 2, 2, 2, 2, 2, 2, 2, 2, 2, 2, 2, 2, 2, 2, 2, 2, 2, 2, 2, 2, 2, 2, 2, 2, 2, 2, 2, 2, 2, 2, 2, 2, 2, 2, 2, 2, 2, 2, 2, 2, 2, 2, 2, 2, 2, 2, 2, 2, 2, 2, 2, 2, 2, 2, 2, 2, 2, 2, 2, 2, 2, 2, 2, 2, 2, 2, 2, 2, 2, 2, 2, 2, 2, 2, 2, 2, 2, 2, 2, 2, 2, 2, 2, 2, 2, 2, 2, 2, 2, 2, 2, 2, 2, 2, 2, 2, 2, 2, 2, 2, 2, 2, 2, 2, 2, 2, 2, 3 ),
 ( 0.000000000000000000, 1.000000000000000000 ),
 ( 0.000000000000000000, 0.002564102564102564100, 0.005128205128205128201, 0.007692307692307692735, 0.01025641025641025640, 0.01282051282051282007, 0.01538461538461538547, 0.01794871794871794740, 0.02051282051282051280, 0.02307692307692307820, 0.02564102564102564014, 0.02820512820512820554, 0.03076923076923077094, 0.03333333333333333287, 0.03589743589743589480, 0.03846153846153846367, 0.04102564102564102561, 0.04358974358974358754, 0.04615384615384615641, 0.04871794871794871834, 0.05128205128205128027, 0.05384615384615384914, 0.05641025641025641107, 0.05897435897435897301, 0.06153846153846154188, 0.06410256410256409687, 0.06666666666666666574, 0.06923076923076923461, 0.07179487179487178961, 0.07435897435897435848, 0.07692307692307692735, 0.07948717948717948234, 0.08205128205128205121, 0.08461538461538462008, 0.08717948717948717507, 0.08974358974358974395, 0.09230769230769231282, 0.09487179487179486781, 0.09743589743589743668, 0.1000000000000000056, 0.1025641025641025605, 0.1051282051282051294, 0.1076923076923076983, 0.1102564102564102533, 0.1128205128205128221, 0.1153846153846153910, 0.1179487179487179460, 0.1205128205128205149, 0.1230769230769230838, 0.1256410256410256387, 0.1282051282051281937, 0.1307692307692307765, 0.1333333333333333315, 0.1358974358974358865, 0.1384615384615384692, 0.1410256410256410242, 0.1435897435897435792, 0.1461538461538461620, 0.1487179487179487170, 0.1512820512820512719, 0.1538461538461538547, 0.1564102564102564097, 0.1589743589743589647, 0.1615384615384615474, 0.1641025641025641024, 0.1666666666666666574, 0.1692307692307692402, 0.1717948717948717952, 0.1743589743589743501, 0.1769230769230769329, 0.1794871794871794879, 0.1820512820512820429, 0.1846153846153846256, 0.1871794871794871806, 0.1897435897435897356, 0.1923076923076923184, 0.1948717948717948734, 0.1974358974358974284, 0.2000000000000000111, 0.2025641025641025661, 0.2051282051282051211, 0.2076923076923077038, 0.2102564102564102588, 0.2128205128205128138, 0.2153846153846153966, 0.2179487179487179516, 0.2205128205128205066, 0.2230769230769230893, 0.2256410256410256443, 0.2282051282051281993, 0.2307692307692307820, 0.2333333333333333370, 0.2358974358974358920, 0.2384615384615384748, 0.2410256410256410298, 0.2435897435897435848, 0.2461538461538461675, 0.2487179487179487225, 0.2512820512820512775, 0.2538461538461538325, 0.2564102564102563875, 0.2589743589743589980, 0.2615384615384615530, 0.2641025641025641080, 0.2666666666666666630, 0.2692307692307692180, 0.2717948717948717730, 0.2743589743589743835, 0.2769230769230769384, 0.2794871794871794934, 0.2820512820512820484, 0.2846153846153846034, 0.2871794871794871584, 0.2897435897435897689, 0.2923076923076923239, 0.2948717948717948789, 0.2974358974358974339, 0.2999999999999999889, 0.3025641025641025439, 0.3051282051282051544, 0.3076923076923077094, 0.3102564102564102644, 0.3128205128205128194, 0.3153846153846153744, 0.3179487179487179294, 0.3205128205128205399, 0.3230769230769230949, 0.3256410256410256499, 0.3282051282051282048, 0.3307692307692307598, 0.3333333333333333148, 0.3358974358974358698, 0.3384615384615384803, 0.3410256410256410353, 0.3435897435897435903, 0.3461538461538461453, 0.3487179487179487003, 0.3512820512820512553, 0.3538461538461538658, 0.3564102564102564208, 0.3589743589743589758, 0.3615384615384615308, 0.3641025641025640858, 0.3666666666666666408, 0.3692307692307692513, 0.3717948717948718063, 0.3743589743589743613, 0.3769230769230769162, 0.3794871794871794712, 0.3820512820512820262, 0.3846153846153846367, 0.3871794871794871917, 0.3897435897435897467, 0.3923076923076923017, 0.3948717948717948567, 0.3974358974358974117, 0.4000000000000000222, 0.4025641025641025772, 0.4051282051282051322, 0.4076923076923076872, 0.4102564102564102422, 0.4128205128205127972, 0.4153846153846154077, 0.4179487179487179627, 0.4205128205128205177, 0.4230769230769230727, 0.4256410256410256276, 0.4282051282051281826, 0.4307692307692307931, 0.4333333333333333481, 0.4358974358974359031, 0.4384615384615384581, 0.4410256410256410131, 0.4435897435897435681, 0.4461538461538461786, 0.4487179487179487336, 0.4512820512820512886, 0.4538461538461538436, 0.4564102564102563986, 0.4589743589743589536, 0.4615384615384615641, 0.4641025641025641191, 0.4666666666666666741, 0.4692307692307692291, 0.4717948717948717841, 0.4743589743589743390, 0.4769230769230769496, 0.4794871794871795045, 0.4820512820512820595, 0.4846153846153846145, 0.4871794871794871695, 0.4897435897435897245, 0.4923076923076923350, 0.4948717948717948900, 0.4974358974358974450, 0.5000000000000000000, 0.5025641025641025550, 0.5051282051282051100, 0.5076923076923076650, 0.5102564102564102200, 0.5128205128205127750, 0.5153846153846153300, 0.5179487179487179960, 0.5205128205128205510, 0.5230769230769231060, 0.5256410256410256610, 0.5282051282051282159, 0.5307692307692307709, 0.5333333333333333259, 0.5358974358974358809, 0.5384615384615384359, 0.5410256410256409909, 0.5435897435897435459, 0.5461538461538461009, 0.5487179487179487669, 0.5512820512820513219, 0.5538461538461538769, 0.5564102564102564319, 0.5589743589743589869, 0.5615384615384615419, 0.5641025641025640969, 0.5666666666666666519, 0.5692307692307692069, 0.5717948717948717618, 0.5743589743589743168, 0.5769230769230768718, 0.5794871794871795379, 0.5820512820512820928, 0.5846153846153846478, 0.5871794871794872028, 0.5897435897435897578, 0.5923076923076923128, 0.5948717948717948678, 0.5974358974358974228, 0.5999999999999999778, 0.6025641025641025328, 0.6051282051282050878, 0.6076923076923076428, 0.6102564102564103088, 0.6128205128205128638, 0.6153846153846154188, 0.6179487179487179738, 0.6205128205128205288, 0.6230769230769230838, 0.6256410256410256387, 0.6282051282051281937, 0.6307692307692307487, 0.6333333333333333037, 0.6358974358974358587, 0.6384615384615384137, 0.6410256410256410797, 0.6435897435897436347, 0.6461538461538461897, 0.6487179487179487447, 0.6512820512820512997, 0.6538461538461538547, 0.6564102564102564097, 0.6589743589743589647, 0.6615384615384615197, 0.6641025641025640747, 0.6666666666666666297, 0.6692307692307691847, 0.6717948717948717396, 0.6743589743589744057, 0.6769230769230769607, 0.6794871794871795156, 0.6820512820512820706, 0.6846153846153846256, 0.6871794871794871806, 0.6897435897435897356, 0.6923076923076922906, 0.6948717948717948456, 0.6974358974358974006, 0.6999999999999999556, 0.7025641025641025106, 0.7051282051282051766, 0.7076923076923077316, 0.7102564102564102866, 0.7128205128205128416, 0.7153846153846153966, 0.7179487179487179516, 0.7205128205128205066, 0.7230769230769230616, 0.7256410256410256165, 0.7282051282051281715, 0.7307692307692307265, 0.7333333333333332815, 0.7358974358974359475, 0.7384615384615385025, 0.7410256410256410575, 0.7435897435897436125, 0.7461538461538461675, 0.7487179487179487225, 0.7512820512820512775, 0.7538461538461538325, 0.7564102564102563875, 0.7589743589743589425, 0.7615384615384614975, 0.7641025641025640525, 0.7666666666666667185, 0.7692307692307692735, 0.7717948717948718285, 0.7743589743589743835, 0.7769230769230769384, 0.7794871794871794934, 0.7820512820512820484, 0.7846153846153846034, 0.7871794871794871584, 0.7897435897435897134, 0.7923076923076922684, 0.7948717948717948234, 0.7974358974358974894, 0.8000000000000000444, 0.8025641025641025994, 0.8051282051282051544, 0.8076923076923077094, 0.8102564102564102644, 0.8128205128205128194, 0.8153846153846153744, 0.8179487179487179294, 0.8205128205128204844, 0.8230769230769230393, 0.8256410256410255943, 0.8282051282051282604, 0.8307692307692308153, 0.8333333333333333703, 0.8358974358974359253, 0.8384615384615384803, 0.8410256410256410353, 0.8435897435897435903, 0.8461538461538461453, 0.8487179487179487003, 0.8512820512820512553, 0.8538461538461538103, 0.8564102564102563653, 0.8589743589743589203, 0.8615384615384615863, 0.8641025641025641413, 0.8666666666666666963, 0.8692307692307692513, 0.8717948717948718063, 0.8743589743589743613, 0.8769230769230769162, 0.8794871794871794712, 0.8820512820512820262, 0.8846153846153845812, 0.8871794871794871362, 0.8897435897435896912, 0.8923076923076923572, 0.8948717948717949122, 0.8974358974358974672, 0.9000000000000000222, 0.9025641025641025772, 0.9051282051282051322, 0.9076923076923076872, 0.9102564102564102422, 0.9128205128205127972, 0.9153846153846153522, 0.9179487179487179072, 0.9205128205128204621, 0.9230769230769231282, 0.9256410256410256832, 0.9282051282051282382, 0.9307692307692307931, 0.9333333333333333481, 0.9358974358974359031, 0.9384615384615384581, 0.9410256410256410131, 0.9435897435897435681, 0.9461538461538461231, 0.9487179487179486781, 0.9512820512820512331, 0.9538461538461538991, 0.9564102564102564541, 0.9589743589743590091, 0.9615384615384615641, 0.9641025641025641191, 0.9666666666666666741, 0.9692307692307692291, 0.9717948717948717841, 0.9743589743589743390, 0.9769230769230768940, 0.9794871794871794490, 0.9820512820512820040, 0.9846153846153846700, 0.9871794871794872250, 0.9897435897435897800, 0.9923076923076923350, 0.9948717948717948900, 0.9974358974358974450, 1.000000000000000000 ),
 .UNSPECIFIED. ) 
 GEOMETRIC_REPRESENTATION_ITEM ( )  RATIONAL_B_SPLINE_SURFACE ( (
 ( 1.000000000000000000, 0.9510565162951535312, 1.000000000000000000, 0.9510565162951535312, 1.000000000000000000, 0.9510565162951535312, 1.000000000000000000, 0.9510565162951535312, 1.000000000000000000, 0.9510565162951535312, 1.000000000000000000, 0.9510565162951535312, 1.000000000000000000, 0.9510565162951535312, 1.000000000000000000, 0.9510565162951535312, 1.000000000000000000, 0.9510565162951535312, 1.000000000000000000, 0.9510565162951535312, 1.000000000000000000, 0.9510565162951535312, 1.000000000000000000, 0.9510565162951535312, 1.000000000000000000, 0.9510565162951535312, 1.000000000000000000, 0.9510565162951535312, 1.000000000000000000, 0.9510565162951535312, 1.000000000000000000, 0.9510565162951535312, 1.000000000000000000, 0.9510565162951535312, 1.000000000000000000, 0.9510565162951535312, 1.000000000000000000, 0.9510565162951535312, 1.000000000000000000, 0.9510565162951535312, 1.000000000000000000, 0.9510565162951535312, 1.000000000000000000, 0.9510565162951535312, 1.000000000000000000, 0.9510565162951535312, 1.000000000000000000, 0.9510565162951535312, 1.000000000000000000, 0.9510565162951535312, 1.000000000000000000, 0.9510565162951535312, 1.000000000000000000, 0.9510565162951535312, 1.000000000000000000, 0.9510565162951535312, 1.000000000000000000, 0.9510565162951535312, 1.000000000000000000, 0.9510565162951535312, 1.000000000000000000, 0.9510565162951535312, 1.000000000000000000, 0.9510565162951535312, 1.000000000000000000, 0.9510565162951535312, 1.000000000000000000, 0.9510565162951535312, 1.000000000000000000, 0.9510565162951535312, 1.000000000000000000, 0.9510565162951535312, 1.000000000000000000, 0.9510565162951535312, 1.000000000000000000, 0.9510565162951535312, 1.000000000000000000, 0.9510565162951535312, 1.000000000000000000, 0.9510565162951535312, 1.000000000000000000, 0.9510565162951535312, 1.000000000000000000, 0.9510565162951535312, 1.000000000000000000, 0.9510565162951535312, 1.000000000000000000, 0.9510565162951535312, 1.000000000000000000, 0.9510565162951535312, 1.000000000000000000, 0.9510565162951535312, 1.000000000000000000, 0.9510565162951535312, 1.000000000000000000, 0.9510565162951535312, 1.000000000000000000, 0.9510565162951535312, 1.000000000000000000, 0.9510565162951535312, 1.000000000000000000, 0.9510565162951535312, 1.000000000000000000, 0.9510565162951535312, 1.000000000000000000, 0.9510565162951535312, 1.000000000000000000, 0.9510565162951535312, 1.000000000000000000, 0.9510565162951535312, 1.000000000000000000, 0.9510565162951535312, 1.000000000000000000, 0.9510565162951535312, 1.000000000000000000, 0.9510565162951535312, 1.000000000000000000, 0.9510565162951535312, 1.000000000000000000, 0.9510565162951535312, 1.000000000000000000, 0.9510565162951535312, 1.000000000000000000, 0.9510565162951535312, 1.000000000000000000, 0.9510565162951535312, 1.000000000000000000, 0.9510565162951535312, 1.000000000000000000, 0.9510565162951535312, 1.000000000000000000, 0.9510565162951535312, 1.000000000000000000, 0.9510565162951535312, 1.000000000000000000, 0.9510565162951535312, 1.000000000000000000, 0.9510565162951535312, 1.000000000000000000, 0.9510565162951535312, 1.000000000000000000, 0.9510565162951535312, 1.000000000000000000, 0.9510565162951535312, 1.000000000000000000, 0.9510565162951535312, 1.000000000000000000, 0.9510565162951535312, 1.000000000000000000, 0.9510565162951535312, 1.000000000000000000, 0.9510565162951535312, 1.000000000000000000, 0.9510565162951535312, 1.000000000000000000, 0.9510565162951535312, 1.000000000000000000, 0.9510565162951535312, 1.000000000000000000, 0.9510565162951535312, 1.000000000000000000, 0.9510565162951535312, 1.000000000000000000, 0.9510565162951535312, 1.000000000000000000, 0.9510565162951535312, 1.000000000000000000, 0.9510565162951535312, 1.000000000000000000, 0.9510565162951535312, 1.000000000000000000, 0.9510565162951535312, 1.000000000000000000, 0.9510565162951535312, 1.000000000000000000, 0.9510565162951535312, 1.000000000000000000, 0.9510565162951535312, 1.000000000000000000, 0.9510565162951535312, 1.000000000000000000, 0.9510565162951535312, 1.000000000000000000, 0.9510565162951535312, 1.000000000000000000, 0.9510565162951535312, 1.000000000000000000, 0.9510565162951535312, 1.000000000000000000, 0.9510565162951535312, 1.000000000000000000, 0.9510565162951535312, 1.000000000000000000, 0.9510565162951535312, 1.000000000000000000, 0.9510565162951535312, 1.000000000000000000, 0.9510565162951535312, 1.000000000000000000, 0.9510565162951535312, 1.000000000000000000, 0.9510565162951535312, 1.000000000000000000, 0.9510565162951535312, 1.000000000000000000, 0.9510565162951535312, 1.000000000000000000, 0.9510565162951535312, 1.000000000000000000, 0.9510565162951535312, 1.000000000000000000, 0.9510565162951535312, 1.000000000000000000, 0.9510565162951535312, 1.000000000000000000, 0.9510565162951535312, 1.000000000000000000, 0.9510565162951535312, 1.000000000000000000, 0.9510565162951535312, 1.000000000000000000, 0.9510565162951535312, 1.000000000000000000, 0.9510565162951535312, 1.000000000000000000, 0.9510565162951535312, 1.000000000000000000, 0.9510565162951535312, 1.000000000000000000, 0.9510565162951535312, 1.000000000000000000, 0.9510565162951535312, 1.000000000000000000, 0.9510565162951535312, 1.000000000000000000, 0.9510565162951535312, 1.000000000000000000, 0.9510565162951535312, 1.000000000000000000, 0.9510565162951535312, 1.000000000000000000, 0.9510565162951535312, 1.000000000000000000, 0.9510565162951535312, 1.000000000000000000, 0.9510565162951535312, 1.000000000000000000, 0.9510565162951535312, 1.000000000000000000, 0.9510565162951535312, 1.000000000000000000, 0.9510565162951535312, 1.000000000000000000, 0.9510565162951535312, 1.000000000000000000, 0.9510565162951535312, 1.000000000000000000, 0.9510565162951535312, 1.000000000000000000, 0.9510565162951535312, 1.000000000000000000, 0.9510565162951535312, 1.000000000000000000, 0.9510565162951535312, 1.000000000000000000, 0.9510565162951535312, 1.000000000000000000, 0.9510565162951535312, 1.000000000000000000, 0.9510565162951535312, 1.000000000000000000, 0.9510565162951535312, 1.000000000000000000, 0.9510565162951535312, 1.000000000000000000, 0.9510565162951535312, 1.000000000000000000, 0.9510565162951535312, 1.000000000000000000, 0.9510565162951535312, 1.000000000000000000, 0.9510565162951535312, 1.000000000000000000, 0.9510565162951535312, 1.000000000000000000, 0.9510565162951535312, 1.000000000000000000, 0.9510565162951535312, 1.000000000000000000, 0.9510565162951535312, 1.000000000000000000, 0.9510565162951535312, 1.000000000000000000, 0.9510565162951535312, 1.000000000000000000, 0.9510565162951535312, 1.000000000000000000, 0.9510565162951535312, 1.000000000000000000, 0.9510565162951535312, 1.000000000000000000, 0.9510565162951535312, 1.000000000000000000, 0.9510565162951535312, 1.000000000000000000, 0.9510565162951535312, 1.000000000000000000, 0.9510565162951535312, 1.000000000000000000, 0.9510565162951535312, 1.000000000000000000, 0.9510565162951535312, 1.000000000000000000, 0.9510565162951535312, 1.000000000000000000, 0.9510565162951535312, 1.000000000000000000, 0.9510565162951535312, 1.000000000000000000, 0.9510565162951535312, 1.000000000000000000, 0.9510565162951535312, 1.000000000000000000, 0.9510565162951535312, 1.000000000000000000, 0.9510565162951535312, 1.000000000000000000, 0.9510565162951535312, 1.000000000000000000, 0.9510565162951535312, 1.000000000000000000, 0.9510565162951535312, 1.000000000000000000, 0.9510565162951535312, 1.000000000000000000, 0.9510565162951535312, 1.000000000000000000, 0.9510565162951535312, 1.000000000000000000, 0.9510565162951535312, 1.000000000000000000, 0.9510565162951535312, 1.000000000000000000, 0.9510565162951535312, 1.000000000000000000, 0.9510565162951535312, 1.000000000000000000, 0.9510565162951535312, 1.000000000000000000, 0.9510565162951535312, 1.000000000000000000, 0.9510565162951535312, 1.000000000000000000, 0.9510565162951535312, 1.000000000000000000, 0.9510565162951535312, 1.000000000000000000, 0.9510565162951535312, 1.000000000000000000, 0.9510565162951535312, 1.000000000000000000, 0.9510565162951535312, 1.000000000000000000, 0.9510565162951535312, 1.000000000000000000, 0.9510565162951535312, 1.000000000000000000, 0.9510565162951535312, 1.000000000000000000, 0.9510565162951535312, 1.000000000000000000, 0.9510565162951535312, 1.000000000000000000, 0.9510565162951535312, 1.000000000000000000, 0.9510565162951535312, 1.000000000000000000, 0.9510565162951535312, 1.000000000000000000, 0.9510565162951535312, 1.000000000000000000, 0.9510565162951535312, 1.000000000000000000, 0.9510565162951535312, 1.000000000000000000, 0.9510565162951535312, 1.000000000000000000, 0.9510565162951535312, 1.000000000000000000, 0.9510565162951535312, 1.000000000000000000, 0.9510565162951535312, 1.000000000000000000, 0.9510565162951535312, 1.000000000000000000, 0.9510565162951535312, 1.000000000000000000, 0.9510565162951535312, 1.000000000000000000, 0.9510565162951535312, 1.000000000000000000, 0.9510565162951535312, 1.000000000000000000, 0.9510565162951535312, 1.000000000000000000, 0.9510565162951535312, 1.000000000000000000, 0.9510565162951535312, 1.000000000000000000, 0.9510565162951535312, 1.000000000000000000, 0.9510565162951535312, 1.000000000000000000, 0.9510565162951535312, 1.000000000000000000, 0.9510565162951535312, 1.000000000000000000, 0.9510565162951535312, 1.000000000000000000, 0.9510565162951535312, 1.000000000000000000, 0.9510565162951535312, 1.000000000000000000, 0.9510565162951535312, 1.000000000000000000, 0.9510565162951535312, 1.000000000000000000, 0.9510565162951535312, 1.000000000000000000, 0.9510565162951535312, 1.000000000000000000, 0.9510565162951535312, 1.000000000000000000, 0.9510565162951535312, 1.000000000000000000, 0.9510565162951535312, 1.000000000000000000, 0.9510565162951535312, 1.000000000000000000, 0.9510565162951535312, 1.000000000000000000, 0.9510565162951535312, 1.000000000000000000, 0.9510565162951535312, 1.000000000000000000, 0.9510565162951535312, 1.000000000000000000, 0.9510565162951535312, 1.000000000000000000, 0.9510565162951535312, 1.000000000000000000, 0.9510565162951535312, 1.000000000000000000, 0.9510565162951535312, 1.000000000000000000, 0.9510565162951535312, 1.000000000000000000, 0.9510565162951535312, 1.000000000000000000, 0.9510565162951535312, 1.000000000000000000, 0.9510565162951535312, 1.000000000000000000, 0.9510565162951535312, 1.000000000000000000, 0.9510565162951535312, 1.000000000000000000, 0.9510565162951535312, 1.000000000000000000, 0.9510565162951535312, 1.000000000000000000, 0.9510565162951535312, 1.000000000000000000, 0.9510565162951535312, 1.000000000000000000, 0.9510565162951535312, 1.000000000000000000, 0.9510565162951535312, 1.000000000000000000, 0.9510565162951535312, 1.000000000000000000, 0.9510565162951535312, 1.000000000000000000, 0.9510565162951535312, 1.000000000000000000, 0.9510565162951535312, 1.000000000000000000, 0.9510565162951535312, 1.000000000000000000, 0.9510565162951535312, 1.000000000000000000, 0.9510565162951535312, 1.000000000000000000, 0.9510565162951535312, 1.000000000000000000, 0.9510565162951535312, 1.000000000000000000, 0.9510565162951535312, 1.000000000000000000, 0.9510565162951535312, 1.000000000000000000, 0.9510565162951535312, 1.000000000000000000, 0.9510565162951535312, 1.000000000000000000, 0.9510565162951535312, 1.000000000000000000, 0.9510565162951535312, 1.000000000000000000, 0.9510565162951535312, 1.000000000000000000, 0.9510565162951535312, 1.000000000000000000, 0.9510565162951535312, 1.000000000000000000, 0.9510565162951535312, 1.000000000000000000, 0.9510565162951535312, 1.000000000000000000, 0.9510565162951535312, 1.000000000000000000, 0.9510565162951535312, 1.000000000000000000, 0.9510565162951535312, 1.000000000000000000, 0.9510565162951535312, 1.000000000000000000, 0.9510565162951535312, 1.000000000000000000, 0.9510565162951535312, 1.000000000000000000, 0.9510565162951535312, 1.000000000000000000, 0.9510565162951535312, 1.000000000000000000, 0.9510565162951535312, 1.000000000000000000, 0.9510565162951535312, 1.000000000000000000, 0.9510565162951535312, 1.000000000000000000, 0.9510565162951535312, 1.000000000000000000, 0.9510565162951535312, 1.000000000000000000, 0.9510565162951535312, 1.000000000000000000, 0.9510565162951535312, 1.000000000000000000, 0.9510565162951535312, 1.000000000000000000, 0.9510565162951535312, 1.000000000000000000, 0.9510565162951535312, 1.000000000000000000, 0.9510565162951535312, 1.000000000000000000, 0.9510565162951535312, 1.000000000000000000, 0.9510565162951535312, 1.000000000000000000, 0.9510565162951535312, 1.000000000000000000, 0.9510565162951535312, 1.000000000000000000, 0.9510565162951535312, 1.000000000000000000, 0.9510565162951535312, 1.000000000000000000, 0.9510565162951535312, 1.000000000000000000, 0.9510565162951535312, 1.000000000000000000, 0.9510565162951535312, 1.000000000000000000, 0.9510565162951535312, 1.000000000000000000, 0.9510565162951535312, 1.000000000000000000, 0.9510565162951535312, 1.000000000000000000, 0.9510565162951535312, 1.000000000000000000, 0.9510565162951535312, 1.000000000000000000, 0.9510565162951535312, 1.000000000000000000, 0.9510565162951535312, 1.000000000000000000, 0.9510565162951535312, 1.000000000000000000, 0.9510565162951535312, 1.000000000000000000, 0.9510565162951535312, 1.000000000000000000, 0.9510565162951535312, 1.000000000000000000, 0.9510565162951535312, 1.000000000000000000, 0.9510565162951535312, 1.000000000000000000, 0.9510565162951535312, 1.000000000000000000, 0.9510565162951535312, 1.000000000000000000, 0.9510565162951535312, 1.000000000000000000, 0.9510565162951535312, 1.000000000000000000, 0.9510565162951535312, 1.000000000000000000, 0.9510565162951535312, 1.000000000000000000, 0.9510565162951535312, 1.000000000000000000, 0.9510565162951535312, 1.000000000000000000, 0.9510565162951535312, 1.000000000000000000, 0.9510565162951535312, 1.000000000000000000, 0.9510565162951535312, 1.000000000000000000, 0.9510565162951535312, 1.000000000000000000, 0.9510565162951535312, 1.000000000000000000, 0.9510565162951535312, 1.000000000000000000, 0.9510565162951535312, 1.000000000000000000, 0.9510565162951535312, 1.000000000000000000, 0.9510565162951535312, 1.000000000000000000, 0.9510565162951535312, 1.000000000000000000, 0.9510565162951535312, 1.000000000000000000, 0.9510565162951535312, 1.000000000000000000, 0.9510565162951535312, 1.000000000000000000, 0.9510565162951535312, 1.000000000000000000, 0.9510565162951535312, 1.000000000000000000, 0.9510565162951535312, 1.000000000000000000, 0.9510565162951535312, 1.000000000000000000, 0.9510565162951535312, 1.000000000000000000, 0.9510565162951535312, 1.000000000000000000, 0.9510565162951535312, 1.000000000000000000, 0.9510565162951535312, 1.000000000000000000, 0.9510565162951535312, 1.000000000000000000, 0.9510565162951535312, 1.000000000000000000, 0.9510565162951535312, 1.000000000000000000, 0.9510565162951535312, 1.000000000000000000, 0.9510565162951535312, 1.000000000000000000, 0.9510565162951535312, 1.000000000000000000, 0.9510565162951535312, 1.000000000000000000, 0.9510565162951535312, 1.000000000000000000, 0.9510565162951535312, 1.000000000000000000, 0.9510565162951535312, 1.000000000000000000, 0.9510565162951535312, 1.000000000000000000, 0.9510565162951535312, 1.000000000000000000, 0.9510565162951535312, 1.000000000000000000, 0.9510565162951535312, 1.000000000000000000, 0.9510565162951535312, 1.000000000000000000, 0.9510565162951535312, 1.000000000000000000, 0.9510565162951535312, 1.000000000000000000, 0.9510565162951535312, 1.000000000000000000, 0.9510565162951535312, 1.000000000000000000, 0.9510565162951535312, 1.000000000000000000, 0.9510565162951535312, 1.000000000000000000, 0.9510565162951535312, 1.000000000000000000, 0.9510565162951535312, 1.000000000000000000, 0.9510565162951535312, 1.000000000000000000, 0.9510565162951535312, 1.000000000000000000, 0.9510565162951535312, 1.000000000000000000, 0.9510565162951535312, 1.000000000000000000, 0.9510565162951535312, 1.000000000000000000, 0.9510565162951535312, 1.000000000000000000, 0.9510565162951535312, 1.000000000000000000, 0.9510565162951535312, 1.000000000000000000, 0.9510565162951535312, 1.000000000000000000, 0.9510565162951535312, 1.000000000000000000, 0.9510565162951535312, 1.000000000000000000, 0.9510565162951535312, 1.000000000000000000, 0.9510565162951535312, 1.000000000000000000, 0.9510565162951535312, 1.000000000000000000, 0.9510565162951535312, 1.000000000000000000, 0.9510565162951535312, 1.000000000000000000, 0.9510565162951535312, 1.000000000000000000, 0.9510565162951535312, 1.000000000000000000, 0.9510565162951535312, 1.000000000000000000, 0.9510565162951535312, 1.000000000000000000, 0.9510565162951535312, 1.000000000000000000, 0.9510565162951535312, 1.000000000000000000, 0.9510565162951535312, 1.000000000000000000, 0.9510565162951535312, 1.000000000000000000, 0.9510565162951535312, 1.000000000000000000, 0.9510565162951535312, 1.000000000000000000, 0.9510565162951535312, 1.000000000000000000, 0.9510565162951535312, 1.000000000000000000, 0.9510565162951535312, 1.000000000000000000, 0.9510565162951535312, 1.000000000000000000, 0.9510565162951535312, 1.000000000000000000, 0.9510565162951535312, 1.000000000000000000, 0.9510565162951535312, 1.000000000000000000, 0.9510565162951535312, 1.000000000000000000, 0.9510565162951535312, 1.000000000000000000, 0.9510565162951535312, 1.000000000000000000, 0.9510565162951535312, 1.000000000000000000, 0.9510565162951535312, 1.000000000000000000),
 ( 1.000000000000000000, 0.9510565162951535312, 1.000000000000000000, 0.9510565162951535312, 1.000000000000000000, 0.9510565162951535312, 1.000000000000000000, 0.9510565162951535312, 1.000000000000000000, 0.9510565162951535312, 1.000000000000000000, 0.9510565162951535312, 1.000000000000000000, 0.9510565162951535312, 1.000000000000000000, 0.9510565162951535312, 1.000000000000000000, 0.9510565162951535312, 1.000000000000000000, 0.9510565162951535312, 1.000000000000000000, 0.9510565162951535312, 1.000000000000000000, 0.9510565162951535312, 1.000000000000000000, 0.9510565162951535312, 1.000000000000000000, 0.9510565162951535312, 1.000000000000000000, 0.9510565162951535312, 1.000000000000000000, 0.9510565162951535312, 1.000000000000000000, 0.9510565162951535312, 1.000000000000000000, 0.9510565162951535312, 1.000000000000000000, 0.9510565162951535312, 1.000000000000000000, 0.9510565162951535312, 1.000000000000000000, 0.9510565162951535312, 1.000000000000000000, 0.9510565162951535312, 1.000000000000000000, 0.9510565162951535312, 1.000000000000000000, 0.9510565162951535312, 1.000000000000000000, 0.9510565162951535312, 1.000000000000000000, 0.9510565162951535312, 1.000000000000000000, 0.9510565162951535312, 1.000000000000000000, 0.9510565162951535312, 1.000000000000000000, 0.9510565162951535312, 1.000000000000000000, 0.9510565162951535312, 1.000000000000000000, 0.9510565162951535312, 1.000000000000000000, 0.9510565162951535312, 1.000000000000000000, 0.9510565162951535312, 1.000000000000000000, 0.9510565162951535312, 1.000000000000000000, 0.9510565162951535312, 1.000000000000000000, 0.9510565162951535312, 1.000000000000000000, 0.9510565162951535312, 1.000000000000000000, 0.9510565162951535312, 1.000000000000000000, 0.9510565162951535312, 1.000000000000000000, 0.9510565162951535312, 1.000000000000000000, 0.9510565162951535312, 1.000000000000000000, 0.9510565162951535312, 1.000000000000000000, 0.9510565162951535312, 1.000000000000000000, 0.9510565162951535312, 1.000000000000000000, 0.9510565162951535312, 1.000000000000000000, 0.9510565162951535312, 1.000000000000000000, 0.9510565162951535312, 1.000000000000000000, 0.9510565162951535312, 1.000000000000000000, 0.9510565162951535312, 1.000000000000000000, 0.9510565162951535312, 1.000000000000000000, 0.9510565162951535312, 1.000000000000000000, 0.9510565162951535312, 1.000000000000000000, 0.9510565162951535312, 1.000000000000000000, 0.9510565162951535312, 1.000000000000000000, 0.9510565162951535312, 1.000000000000000000, 0.9510565162951535312, 1.000000000000000000, 0.9510565162951535312, 1.000000000000000000, 0.9510565162951535312, 1.000000000000000000, 0.9510565162951535312, 1.000000000000000000, 0.9510565162951535312, 1.000000000000000000, 0.9510565162951535312, 1.000000000000000000, 0.9510565162951535312, 1.000000000000000000, 0.9510565162951535312, 1.000000000000000000, 0.9510565162951535312, 1.000000000000000000, 0.9510565162951535312, 1.000000000000000000, 0.9510565162951535312, 1.000000000000000000, 0.9510565162951535312, 1.000000000000000000, 0.9510565162951535312, 1.000000000000000000, 0.9510565162951535312, 1.000000000000000000, 0.9510565162951535312, 1.000000000000000000, 0.9510565162951535312, 1.000000000000000000, 0.9510565162951535312, 1.000000000000000000, 0.9510565162951535312, 1.000000000000000000, 0.9510565162951535312, 1.000000000000000000, 0.9510565162951535312, 1.000000000000000000, 0.9510565162951535312, 1.000000000000000000, 0.9510565162951535312, 1.000000000000000000, 0.9510565162951535312, 1.000000000000000000, 0.9510565162951535312, 1.000000000000000000, 0.9510565162951535312, 1.000000000000000000, 0.9510565162951535312, 1.000000000000000000, 0.9510565162951535312, 1.000000000000000000, 0.9510565162951535312, 1.000000000000000000, 0.9510565162951535312, 1.000000000000000000, 0.9510565162951535312, 1.000000000000000000, 0.9510565162951535312, 1.000000000000000000, 0.9510565162951535312, 1.000000000000000000, 0.9510565162951535312, 1.000000000000000000, 0.9510565162951535312, 1.000000000000000000, 0.9510565162951535312, 1.000000000000000000, 0.9510565162951535312, 1.000000000000000000, 0.9510565162951535312, 1.000000000000000000, 0.9510565162951535312, 1.000000000000000000, 0.9510565162951535312, 1.000000000000000000, 0.9510565162951535312, 1.000000000000000000, 0.9510565162951535312, 1.000000000000000000, 0.9510565162951535312, 1.000000000000000000, 0.9510565162951535312, 1.000000000000000000, 0.9510565162951535312, 1.000000000000000000, 0.9510565162951535312, 1.000000000000000000, 0.9510565162951535312, 1.000000000000000000, 0.9510565162951535312, 1.000000000000000000, 0.9510565162951535312, 1.000000000000000000, 0.9510565162951535312, 1.000000000000000000, 0.9510565162951535312, 1.000000000000000000, 0.9510565162951535312, 1.000000000000000000, 0.9510565162951535312, 1.000000000000000000, 0.9510565162951535312, 1.000000000000000000, 0.9510565162951535312, 1.000000000000000000, 0.9510565162951535312, 1.000000000000000000, 0.9510565162951535312, 1.000000000000000000, 0.9510565162951535312, 1.000000000000000000, 0.9510565162951535312, 1.000000000000000000, 0.9510565162951535312, 1.000000000000000000, 0.9510565162951535312, 1.000000000000000000, 0.9510565162951535312, 1.000000000000000000, 0.9510565162951535312, 1.000000000000000000, 0.9510565162951535312, 1.000000000000000000, 0.9510565162951535312, 1.000000000000000000, 0.9510565162951535312, 1.000000000000000000, 0.9510565162951535312, 1.000000000000000000, 0.9510565162951535312, 1.000000000000000000, 0.9510565162951535312, 1.000000000000000000, 0.9510565162951535312, 1.000000000000000000, 0.9510565162951535312, 1.000000000000000000, 0.9510565162951535312, 1.000000000000000000, 0.9510565162951535312, 1.000000000000000000, 0.9510565162951535312, 1.000000000000000000, 0.9510565162951535312, 1.000000000000000000, 0.9510565162951535312, 1.000000000000000000, 0.9510565162951535312, 1.000000000000000000, 0.9510565162951535312, 1.000000000000000000, 0.9510565162951535312, 1.000000000000000000, 0.9510565162951535312, 1.000000000000000000, 0.9510565162951535312, 1.000000000000000000, 0.9510565162951535312, 1.000000000000000000, 0.9510565162951535312, 1.000000000000000000, 0.9510565162951535312, 1.000000000000000000, 0.9510565162951535312, 1.000000000000000000, 0.9510565162951535312, 1.000000000000000000, 0.9510565162951535312, 1.000000000000000000, 0.9510565162951535312, 1.000000000000000000, 0.9510565162951535312, 1.000000000000000000, 0.9510565162951535312, 1.000000000000000000, 0.9510565162951535312, 1.000000000000000000, 0.9510565162951535312, 1.000000000000000000, 0.9510565162951535312, 1.000000000000000000, 0.9510565162951535312, 1.000000000000000000, 0.9510565162951535312, 1.000000000000000000, 0.9510565162951535312, 1.000000000000000000, 0.9510565162951535312, 1.000000000000000000, 0.9510565162951535312, 1.000000000000000000, 0.9510565162951535312, 1.000000000000000000, 0.9510565162951535312, 1.000000000000000000, 0.9510565162951535312, 1.000000000000000000, 0.9510565162951535312, 1.000000000000000000, 0.9510565162951535312, 1.000000000000000000, 0.9510565162951535312, 1.000000000000000000, 0.9510565162951535312, 1.000000000000000000, 0.9510565162951535312, 1.000000000000000000, 0.9510565162951535312, 1.000000000000000000, 0.9510565162951535312, 1.000000000000000000, 0.9510565162951535312, 1.000000000000000000, 0.9510565162951535312, 1.000000000000000000, 0.9510565162951535312, 1.000000000000000000, 0.9510565162951535312, 1.000000000000000000, 0.9510565162951535312, 1.000000000000000000, 0.9510565162951535312, 1.000000000000000000, 0.9510565162951535312, 1.000000000000000000, 0.9510565162951535312, 1.000000000000000000, 0.9510565162951535312, 1.000000000000000000, 0.9510565162951535312, 1.000000000000000000, 0.9510565162951535312, 1.000000000000000000, 0.9510565162951535312, 1.000000000000000000, 0.9510565162951535312, 1.000000000000000000, 0.9510565162951535312, 1.000000000000000000, 0.9510565162951535312, 1.000000000000000000, 0.9510565162951535312, 1.000000000000000000, 0.9510565162951535312, 1.000000000000000000, 0.9510565162951535312, 1.000000000000000000, 0.9510565162951535312, 1.000000000000000000, 0.9510565162951535312, 1.000000000000000000, 0.9510565162951535312, 1.000000000000000000, 0.9510565162951535312, 1.000000000000000000, 0.9510565162951535312, 1.000000000000000000, 0.9510565162951535312, 1.000000000000000000, 0.9510565162951535312, 1.000000000000000000, 0.9510565162951535312, 1.000000000000000000, 0.9510565162951535312, 1.000000000000000000, 0.9510565162951535312, 1.000000000000000000, 0.9510565162951535312, 1.000000000000000000, 0.9510565162951535312, 1.000000000000000000, 0.9510565162951535312, 1.000000000000000000, 0.9510565162951535312, 1.000000000000000000, 0.9510565162951535312, 1.000000000000000000, 0.9510565162951535312, 1.000000000000000000, 0.9510565162951535312, 1.000000000000000000, 0.9510565162951535312, 1.000000000000000000, 0.9510565162951535312, 1.000000000000000000, 0.9510565162951535312, 1.000000000000000000, 0.9510565162951535312, 1.000000000000000000, 0.9510565162951535312, 1.000000000000000000, 0.9510565162951535312, 1.000000000000000000, 0.9510565162951535312, 1.000000000000000000, 0.9510565162951535312, 1.000000000000000000, 0.9510565162951535312, 1.000000000000000000, 0.9510565162951535312, 1.000000000000000000, 0.9510565162951535312, 1.000000000000000000, 0.9510565162951535312, 1.000000000000000000, 0.9510565162951535312, 1.000000000000000000, 0.9510565162951535312, 1.000000000000000000, 0.9510565162951535312, 1.000000000000000000, 0.9510565162951535312, 1.000000000000000000, 0.9510565162951535312, 1.000000000000000000, 0.9510565162951535312, 1.000000000000000000, 0.9510565162951535312, 1.000000000000000000, 0.9510565162951535312, 1.000000000000000000, 0.9510565162951535312, 1.000000000000000000, 0.9510565162951535312, 1.000000000000000000, 0.9510565162951535312, 1.000000000000000000, 0.9510565162951535312, 1.000000000000000000, 0.9510565162951535312, 1.000000000000000000, 0.9510565162951535312, 1.000000000000000000, 0.9510565162951535312, 1.000000000000000000, 0.9510565162951535312, 1.000000000000000000, 0.9510565162951535312, 1.000000000000000000, 0.9510565162951535312, 1.000000000000000000, 0.9510565162951535312, 1.000000000000000000, 0.9510565162951535312, 1.000000000000000000, 0.9510565162951535312, 1.000000000000000000, 0.9510565162951535312, 1.000000000000000000, 0.9510565162951535312, 1.000000000000000000, 0.9510565162951535312, 1.000000000000000000, 0.9510565162951535312, 1.000000000000000000, 0.9510565162951535312, 1.000000000000000000, 0.9510565162951535312, 1.000000000000000000, 0.9510565162951535312, 1.000000000000000000, 0.9510565162951535312, 1.000000000000000000, 0.9510565162951535312, 1.000000000000000000, 0.9510565162951535312, 1.000000000000000000, 0.9510565162951535312, 1.000000000000000000, 0.9510565162951535312, 1.000000000000000000, 0.9510565162951535312, 1.000000000000000000, 0.9510565162951535312, 1.000000000000000000, 0.9510565162951535312, 1.000000000000000000, 0.9510565162951535312, 1.000000000000000000, 0.9510565162951535312, 1.000000000000000000, 0.9510565162951535312, 1.000000000000000000, 0.9510565162951535312, 1.000000000000000000, 0.9510565162951535312, 1.000000000000000000, 0.9510565162951535312, 1.000000000000000000, 0.9510565162951535312, 1.000000000000000000, 0.9510565162951535312, 1.000000000000000000, 0.9510565162951535312, 1.000000000000000000, 0.9510565162951535312, 1.000000000000000000, 0.9510565162951535312, 1.000000000000000000, 0.9510565162951535312, 1.000000000000000000, 0.9510565162951535312, 1.000000000000000000, 0.9510565162951535312, 1.000000000000000000, 0.9510565162951535312, 1.000000000000000000, 0.9510565162951535312, 1.000000000000000000, 0.9510565162951535312, 1.000000000000000000, 0.9510565162951535312, 1.000000000000000000, 0.9510565162951535312, 1.000000000000000000, 0.9510565162951535312, 1.000000000000000000, 0.9510565162951535312, 1.000000000000000000, 0.9510565162951535312, 1.000000000000000000, 0.9510565162951535312, 1.000000000000000000, 0.9510565162951535312, 1.000000000000000000, 0.9510565162951535312, 1.000000000000000000, 0.9510565162951535312, 1.000000000000000000, 0.9510565162951535312, 1.000000000000000000, 0.9510565162951535312, 1.000000000000000000, 0.9510565162951535312, 1.000000000000000000, 0.9510565162951535312, 1.000000000000000000, 0.9510565162951535312, 1.000000000000000000, 0.9510565162951535312, 1.000000000000000000, 0.9510565162951535312, 1.000000000000000000, 0.9510565162951535312, 1.000000000000000000, 0.9510565162951535312, 1.000000000000000000, 0.9510565162951535312, 1.000000000000000000, 0.9510565162951535312, 1.000000000000000000, 0.9510565162951535312, 1.000000000000000000, 0.9510565162951535312, 1.000000000000000000, 0.9510565162951535312, 1.000000000000000000, 0.9510565162951535312, 1.000000000000000000, 0.9510565162951535312, 1.000000000000000000, 0.9510565162951535312, 1.000000000000000000, 0.9510565162951535312, 1.000000000000000000, 0.9510565162951535312, 1.000000000000000000, 0.9510565162951535312, 1.000000000000000000, 0.9510565162951535312, 1.000000000000000000, 0.9510565162951535312, 1.000000000000000000, 0.9510565162951535312, 1.000000000000000000, 0.9510565162951535312, 1.000000000000000000, 0.9510565162951535312, 1.000000000000000000, 0.9510565162951535312, 1.000000000000000000, 0.9510565162951535312, 1.000000000000000000, 0.9510565162951535312, 1.000000000000000000, 0.9510565162951535312, 1.000000000000000000, 0.9510565162951535312, 1.000000000000000000, 0.9510565162951535312, 1.000000000000000000, 0.9510565162951535312, 1.000000000000000000, 0.9510565162951535312, 1.000000000000000000, 0.9510565162951535312, 1.000000000000000000, 0.9510565162951535312, 1.000000000000000000, 0.9510565162951535312, 1.000000000000000000, 0.9510565162951535312, 1.000000000000000000, 0.9510565162951535312, 1.000000000000000000, 0.9510565162951535312, 1.000000000000000000, 0.9510565162951535312, 1.000000000000000000, 0.9510565162951535312, 1.000000000000000000, 0.9510565162951535312, 1.000000000000000000, 0.9510565162951535312, 1.000000000000000000, 0.9510565162951535312, 1.000000000000000000, 0.9510565162951535312, 1.000000000000000000, 0.9510565162951535312, 1.000000000000000000, 0.9510565162951535312, 1.000000000000000000, 0.9510565162951535312, 1.000000000000000000, 0.9510565162951535312, 1.000000000000000000, 0.9510565162951535312, 1.000000000000000000, 0.9510565162951535312, 1.000000000000000000, 0.9510565162951535312, 1.000000000000000000, 0.9510565162951535312, 1.000000000000000000, 0.9510565162951535312, 1.000000000000000000, 0.9510565162951535312, 1.000000000000000000, 0.9510565162951535312, 1.000000000000000000, 0.9510565162951535312, 1.000000000000000000, 0.9510565162951535312, 1.000000000000000000, 0.9510565162951535312, 1.000000000000000000, 0.9510565162951535312, 1.000000000000000000, 0.9510565162951535312, 1.000000000000000000, 0.9510565162951535312, 1.000000000000000000, 0.9510565162951535312, 1.000000000000000000, 0.9510565162951535312, 1.000000000000000000, 0.9510565162951535312, 1.000000000000000000, 0.9510565162951535312, 1.000000000000000000, 0.9510565162951535312, 1.000000000000000000, 0.9510565162951535312, 1.000000000000000000, 0.9510565162951535312, 1.000000000000000000, 0.9510565162951535312, 1.000000000000000000, 0.9510565162951535312, 1.000000000000000000, 0.9510565162951535312, 1.000000000000000000, 0.9510565162951535312, 1.000000000000000000, 0.9510565162951535312, 1.000000000000000000, 0.9510565162951535312, 1.000000000000000000, 0.9510565162951535312, 1.000000000000000000, 0.9510565162951535312, 1.000000000000000000, 0.9510565162951535312, 1.000000000000000000, 0.9510565162951535312, 1.000000000000000000, 0.9510565162951535312, 1.000000000000000000, 0.9510565162951535312, 1.000000000000000000, 0.9510565162951535312, 1.000000000000000000, 0.9510565162951535312, 1.000000000000000000, 0.9510565162951535312, 1.000000000000000000, 0.9510565162951535312, 1.000000000000000000, 0.9510565162951535312, 1.000000000000000000, 0.9510565162951535312, 1.000000000000000000, 0.9510565162951535312, 1.000000000000000000, 0.9510565162951535312, 1.000000000000000000, 0.9510565162951535312, 1.000000000000000000, 0.9510565162951535312, 1.000000000000000000, 0.9510565162951535312, 1.000000000000000000, 0.9510565162951535312, 1.000000000000000000, 0.9510565162951535312, 1.000000000000000000, 0.9510565162951535312, 1.000000000000000000, 0.9510565162951535312, 1.000000000000000000, 0.9510565162951535312, 1.000000000000000000, 0.9510565162951535312, 1.000000000000000000, 0.9510565162951535312, 1.000000000000000000, 0.9510565162951535312, 1.000000000000000000, 0.9510565162951535312, 1.000000000000000000, 0.9510565162951535312, 1.000000000000000000, 0.9510565162951535312, 1.000000000000000000, 0.9510565162951535312, 1.000000000000000000, 0.9510565162951535312, 1.000000000000000000, 0.9510565162951535312, 1.000000000000000000, 0.9510565162951535312, 1.000000000000000000, 0.9510565162951535312, 1.000000000000000000, 0.9510565162951535312, 1.000000000000000000, 0.9510565162951535312, 1.000000000000000000, 0.9510565162951535312, 1.000000000000000000, 0.9510565162951535312, 1.000000000000000000, 0.9510565162951535312, 1.000000000000000000, 0.9510565162951535312, 1.000000000000000000, 0.9510565162951535312, 1.000000000000000000, 0.9510565162951535312, 1.000000000000000000, 0.9510565162951535312, 1.000000000000000000, 0.9510565162951535312, 1.000000000000000000, 0.9510565162951535312, 1.000000000000000000) ) ) 
 REPRESENTATION_ITEM ( '' )  SURFACE ( )  );
#32611 = CYLINDRICAL_SURFACE ( 'NONE', #18479, 33.00000000000000000 ) ;
#32612 = CARTESIAN_POINT ( 'NONE',  ( 10.37757302488624056, 46.52500000273117564, -31.93888565452638417 ) ) ;
#32613 = CARTESIAN_POINT ( 'NONE',  ( 10.37757302488624767, 3.975000002731182924, 31.93888565452638417 ) ) ;
#32614 = CARTESIAN_POINT ( 'NONE',  ( 33.58253175000000113, 64.47500000273120691, -10.91162601494193574 ) ) ;
#32615 = CARTESIAN_POINT ( 'NONE',  ( -2.428612866367529427E-13, 46.80468750000000000, -27.95245687107223276 ) ) ;
#32616 = CARTESIAN_POINT ( 'NONE',  ( -28.02196122052045268, 40.36496500092396644, 7.468012846824790607 ) ) ;
#32617 = CARTESIAN_POINT ( 'NONE',  ( 30.02300923189239867, 29.03868083240935505, -0.04044903255044467877 ) ) ;
#32618 = CARTESIAN_POINT ( 'NONE',  ( 32.50000000000000000, 67.50000000546239676, -3.980102097228898626E-15 ) ) ;
#32619 = PLANE ( 'NONE',  #21014 ) ;
#32620 = AXIS2_PLACEMENT_3D ( 'NONE', #17689, #22483, #22828 ) ;
#32621 = CARTESIAN_POINT ( 'NONE',  ( -26.09010956794245217, 54.96315999907602645, -6.950374756619243755 ) ) ;
#32622 = EDGE_CURVE ( 'NONE', #27495, #23590, #24397, .T. ) ;
#32623 = CARTESIAN_POINT ( 'NONE',  ( -3.880418787951142701, 5.198745712990781698, 24.49999999999999645 ) ) ;
#32624 = EDGE_LOOP ( 'NONE', ( #538, #22941, #22364, #9850 ) ) ;
#32625 = CARTESIAN_POINT ( 'NONE',  ( -27.16883889988624290, 41.17500000273118133, -19.73931689729374028 ) ) ;
#32626 = CARTESIAN_POINT ( 'NONE',  ( 1.076200423132605543E-16, 66.99999999999998579, -46.18802153517007980 ) ) ;
#32627 = CARTESIAN_POINT ( 'NONE',  ( 32.50000000000000000, 29.60000000546238041, -10.55989012756945833 ) ) ;
#32628 = ORIENTED_EDGE ( 'NONE', *, *, #15361, .T. ) ;
#32629 = EDGE_CURVE ( 'NONE', #5219, #1686, #25817, .T. ) ;
#32630 = EDGE_CURVE ( 'NONE', #28636, #22217, #2363, .T. ) ;
#32631 = CARTESIAN_POINT ( 'NONE',  ( 15.01150461594643204, 37.92447916666666430, 26.00068869287340334 ) ) ;
#32632 = ORIENTED_EDGE ( 'NONE', *, *, #6845, .F. ) ;
#32633 = ORIENTED_EDGE ( 'NONE', *, *, #5798, .T. ) ;
#32634 = DIRECTION ( 'NONE',  ( -1.224646799147353454E-16, 1.000000000000000000, -0.000000000000000000 ) ) ;
#32635 = CARTESIAN_POINT ( 'NONE',  ( 20.75514604977249178, 49.82500000273117990, 28.56700777964553950 ) ) ;
#32636 = CARTESIAN_POINT ( 'NONE',  ( 7.505752307972854531, 57.26041666666666430, -28.01184896238303423 ) ) ;
#32637 = CARTESIAN_POINT ( 'NONE',  ( -10.04305231718578462, 10.90000000546237402, 30.90933677959249337 ) ) ;
#32638 = DIRECTION ( 'NONE',  ( -1.224646799147353207E-16, -1.499759782661857882E-32, 1.000000000000000000 ) ) ;
#32639 = CARTESIAN_POINT ( 'NONE',  ( 23.41746824999999887, 15.22499999726880482, -7.608796670333727974 ) ) ;
#32640 = CARTESIAN_POINT ( 'NONE',  ( -10.04305231718579172, 55.59999999999998010, -30.90933677959248982 ) ) ;
#32641 = CARTESIAN_POINT ( 'NONE',  ( -27.16883889988623935, 23.57500000273119056, 19.73931689729374739 ) ) ;
#32642 = CARTESIAN_POINT ( 'NONE',  ( -6.668400408272875007E-16, 0.5000000000000068834, -24.50000000000000355 ) ) ;
#32643 = CARTESIAN_POINT ( 'NONE',  ( -26.09010956794245217, 17.15065999907602290, -6.950374756619243755 ) ) ;
#32644 = CARTESIAN_POINT ( 'NONE',  ( 4.300734207923757602, 72.27500000273117564, -13.23629886949340673 ) ) ;
#32645 = CARTESIAN_POINT ( 'NONE',  ( -8.891200544363830713E-16, 77.75000000546236834, -15.00000000000000000 ) ) ;
#32646 = DIRECTION ( 'NONE',  ( -1.000000000000000000, -1.111257322145974683E-16, 0.000000000000000000 ) ) ;
#32647 = CARTESIAN_POINT ( 'NONE',  ( 32.50000000000000000, 3.000000000000002665, -3.980102097228898626E-15 ) ) ;
#32648 = EDGE_LOOP ( 'NONE', ( #22465, #32542, #18658, #24784 ) ) ;
#32649 = CARTESIAN_POINT ( 'NONE',  ( 23.41746824999999887, 9.124999997268817609, 0.000000000000000000 ) ) ;
#32650 = PLANE ( 'NONE',  #1368 ) ;
#32651 = CARTESIAN_POINT ( 'NONE',  ( -13.97622843553632421, 43.08072916666666430, -24.20753774853731599 ) ) ;
#32652 = CARTESIAN_POINT ( 'NONE',  ( -10.37757302488623701, 63.52500000273118985, 31.93888565452638417 ) ) ;
#32653 = CARTESIAN_POINT ( 'NONE',  ( 10.37757302488624767, 27.97500000273118914, 31.93888565452638417 ) ) ;
#32654 = CARTESIAN_POINT ( 'NONE',  ( 27.16883889988624290, 16.17500000273118488, 19.73931689729373673 ) ) ;
#32655 = CARTESIAN_POINT ( 'NONE',  ( 20.75514604977248467, 8.675000002731195536, -28.56700777964554305 ) ) ;
#32656 = CARTESIAN_POINT ( 'NONE',  ( 15.04653450569292872, 10.71652750092397888, -25.98046417659857710 ) ) ;
#32657 = CARTESIAN_POINT ( 'NONE',  ( 26.00068869287340334, 50.81510416666667140, -15.01150461594642316 ) ) ;
#32658 = DIRECTION ( 'NONE',  ( 0.7071067811865465735, 0.7071067811865484609, 8.659560562354922997E-17 ) ) ;
#32659 = CARTESIAN_POINT ( 'NONE',  ( -8.601468415847518756, 79.07500000273121543, -11.83890561707634603 ) ) ;
#32660 = CARTESIAN_POINT ( 'NONE',  ( 32.50000000000000000, 49.00000000000000000, -3.980102097228898626E-15 ) ) ;
#32661 = CARTESIAN_POINT ( 'NONE',  ( 15.14183272437242422, 8.049999994537621717, -20.84094480462497856 ) ) ;
#32662 = CARTESIAN_POINT ( 'NONE',  ( 10.37757302488624056, 50.52500000273118985, -31.93888565452638417 ) ) ;
#32663 = CARTESIAN_POINT ( 'NONE',  ( 7.236395654485760609, 3.024999997268823293, -22.27133577429736633 ) ) ;
#32664 = ORIENTED_EDGE ( 'NONE', *, *, #21544, .T. ) ;
#32665 = CARTESIAN_POINT ( 'NONE',  ( 33.58253175000000113, 58.47500000273118559, -10.91162601494193751 ) ) ;
#32666 = LINE ( 'NONE', #4190, #33829 ) ;
#32667 = CARTESIAN_POINT ( 'NONE',  ( 18.94512977948576093, 14.82499999726882933, -13.76444248337722875 ) ) ;
#32668 = CARTESIAN_POINT ( 'NONE',  ( 13.94119854578937812, 35.92486083425730214, 24.22776226481240514 ) ) ;
#32669 = EDGE_LOOP ( 'NONE', ( #17799, #24762, #10245, #14873 ) ) ;
#32670 = CARTESIAN_POINT ( 'NONE',  ( -2.162160676586881955E-15, 28.62500000273118062, -35.31076352940723240 ) ) ;
#32671 = VERTEX_POINT ( 'NONE', #31710 ) ;
#32672 = CARTESIAN_POINT ( 'NONE',  ( 15.01150461594643204, 65.42447916666667140, 26.00068869287340334 ) ) ;
#32673 = CARTESIAN_POINT ( 'NONE',  ( -10.37757302488624411, 62.97500000273120691, -31.93888565452638417 ) ) ;
#32674 = CARTESIAN_POINT ( 'NONE',  ( -9.270509831248423538, 75.69999999999998863, -12.75976212528059861 ) ) ;
#32675 = CARTESIAN_POINT ( 'NONE',  ( -20.75514604977248823, 76.82500000273120122, -28.56700777964554305 ) ) ;
#32676 = CARTESIAN_POINT ( 'NONE',  ( 20.50609665440969565, 33.48437500000000000, -20.50609665441004736 ) ) ;
#32677 = CARTESIAN_POINT ( 'NONE',  ( 15.14183272437242245, 4.300000000000009592, -20.84094480462497856 ) ) ;
#32678 = FACE_OUTER_BOUND ( 'NONE', #31981, .T. ) ;
#32679 = ADVANCED_FACE ( 'NONE', ( #5297 ), #7697, .T. ) ;
#32680 = CARTESIAN_POINT ( 'NONE',  ( 33.58253175000000113, 14.12500000273120193, -4.112674001490185761E-15 ) ) ;
#32681 = CARTESIAN_POINT ( 'NONE',  ( 8.601468415847520532, 71.57500000273118701, 11.83890561707634603 ) ) ;
#32682 = CARTESIAN_POINT ( 'NONE',  ( -26.02091320914878025, 44.79388916574269075, -14.97647472619899389 ) ) ;
#32683 = CARTESIAN_POINT ( 'NONE',  ( -4.635254915624211769, 79.60000000000000853, -14.26584774442730286 ) ) ;
#32684 = CARTESIAN_POINT ( 'NONE',  ( 26.00068869287341045, 61.12760416666666430, -15.01150461594642493 ) ) ;
#32685 = CARTESIAN_POINT ( 'NONE',  ( -15.14183272437242067, 8.449999994537638059, -20.84094480462497856 ) ) ;
#32686 = CARTESIAN_POINT ( 'NONE',  ( 24.50000000000000000, 9.749999994537628112, 0.000000000000000000 ) ) ;
#32687 = CARTESIAN_POINT ( 'NONE',  ( -4.635254915624208216, 76.65000000546237402, 14.26584774442730463 ) ) ;
#32688 = CARTESIAN_POINT ( 'NONE',  ( 27.95245687107223276, 66.85118083240935505, -0.04044903255042905932 ) ) ;
#32689 = CARTESIAN_POINT ( 'NONE',  ( 10.37757302488624767, 35.72500000273118559, 31.93888565452638417 ) ) ;
#32690 = CARTESIAN_POINT ( 'NONE',  ( -4.300734207923755825, 73.27500000273118985, 13.23629886949340673 ) ) ;
#32691 = CARTESIAN_POINT ( 'NONE',  ( -10.37757302488623701, 47.77500000273120406, 31.93888565452638417 ) ) ;
#32692 = CARTESIAN_POINT ( 'NONE',  ( -10.37757302488623701, 27.77500000273119696, 31.93888565452638417 ) ) ;
#32693 = FACE_OUTER_BOUND ( 'NONE', #31713, .T. ) ;
#32694 = CARTESIAN_POINT ( 'NONE',  ( 6.988114217768294445, 34.63020833333332860, 26.07999730980477437 ) ) ;
#32695 = CARTESIAN_POINT ( 'NONE',  ( -26.29305231718578995, 18.19999999999999574, 19.10302069950538595 ) ) ;
#32696 = CYLINDRICAL_SURFACE ( 'NONE', #16223, 24.49999999999999645 ) ;
#32697 = CARTESIAN_POINT ( 'NONE',  ( -32.50000000000000000, 64.10000000000000853, 10.55989012756946366 ) ) ;
#32698 = CARTESIAN_POINT ( 'NONE',  ( 18.94512977948575738, 8.424999997268811214, 13.76444248337723408 ) ) ;
#32699 = CARTESIAN_POINT ( 'NONE',  ( -26.02091320914878025, 27.60638916574269075, -14.97647472619899389 ) ) ;
#32700 = CARTESIAN_POINT ( 'NONE',  ( -9.270509831248423538, 77.69999999999998863, -12.75976212528059861 ) ) ;
#32701 = CARTESIAN_POINT ( 'NONE',  ( -0.04044903255042732459, 41.92930583240936215, -27.95245687107223986 ) ) ;
#32702 = CARTESIAN_POINT ( 'NONE',  ( -20.75514604977248823, 12.82500000273118168, -28.56700777964554305 ) ) ;
#32703 = CARTESIAN_POINT ( 'NONE',  ( -23.41746824999999887, 6.124999997268814944, -2.867812753649727150E-15 ) ) ;
#32704 = CARTESIAN_POINT ( 'NONE',  ( 27.95245687107222921, 64.85156249999998579, -2.463307335887066074E-13 ) ) ;
#32705 = ORIENTED_EDGE ( 'NONE', *, *, #19118, .T. ) ;
#32706 = CARTESIAN_POINT ( 'NONE',  ( 6.486482029760649416E-15, 53.62500000273119838, 35.31076352940723240 ) ) ;
#32707 = CARTESIAN_POINT ( 'NONE',  ( -27.16883889988624290, 29.17500000273119554, -19.73931689729374028 ) ) ;
#32708 = ORIENTED_EDGE ( 'NONE', *, *, #7884, .T. ) ;
#32709 = CARTESIAN_POINT ( 'NONE',  ( -15.01150461594595775, 21.30989583333331794, 26.00068869287368756 ) ) ;
#32710 = CARTESIAN_POINT ( 'NONE',  ( -30.02300923189239867, 26.75819416759064495, -0.04044903254991731589 ) ) ;
#32711 = CARTESIAN_POINT ( 'NONE',  ( -5.147494310547423346, 72.94874572391552192, 32.50000000000000000 ) ) ;
#32712 = CARTESIAN_POINT ( 'NONE',  ( 24.50000000000000355, 17.84999999453763309, -7.960532557706203605 ) ) ;
#32713 = CARTESIAN_POINT ( 'NONE',  ( 18.94512977948576093, 4.824999997268819563, -13.76444248337722875 ) ) ;
#32714 = CARTESIAN_POINT ( 'NONE',  ( -33.58253175000000113, 23.37500000273118417, 0.000000000000000000 ) ) ;
#32715 = CARTESIAN_POINT ( 'NONE',  ( -10.04305231718578462, 22.90000000546238468, 30.90933677959249337 ) ) ;
#32716 = EDGE_CURVE ( 'NONE', #29542, #3689, #17707, .T. ) ;
#32717 = CARTESIAN_POINT ( 'NONE',  ( 20.08610463437157279, 75.30000000000001137, -27.64615127144129758 ) ) ;
#32718 = CARTESIAN_POINT ( 'NONE',  ( -1.778240108872766143E-15, 48.00000000546238255, -32.49999999999999289 ) ) ;
#32719 = CARTESIAN_POINT ( 'NONE',  ( 4.805950183054497948, 74.00000000000001421, 13.09988514501729284 ) ) ;
#32720 = CARTESIAN_POINT ( 'NONE',  ( 15.04653450569292872, 55.40402750092397355, -25.98046417659857710 ) ) ;
#32721 = CARTESIAN_POINT ( 'NONE',  ( -33.58253175000000113, 37.37500000273119838, 0.000000000000000000 ) ) ;
#32722 = CARTESIAN_POINT ( 'NONE',  ( 6.486482029760648627E-15, 57.62500000273119127, 35.31076352940722529 ) ) ;
#32723 = CARTESIAN_POINT ( 'NONE',  ( -20.50609665441004736, 32.62500000000000000, -20.50609665440969565 ) ) ;
#32724 =( NAMED_UNIT ( * ) SI_UNIT ( $, .STERADIAN. ) SOLID_ANGLE_UNIT ( ) );
#32725 = EDGE_CURVE ( 'NONE', #32333, #5219, #5677, .T. ) ;
#32726 = VECTOR ( 'NONE', #20603, 1000.000000000000000 ) ;
#32727 = CARTESIAN_POINT ( 'NONE',  ( 14.47279130897151767, 11.42499999726880944, -19.92008829642072598 ) ) ;
#32728 = CARTESIAN_POINT ( 'NONE',  ( -20.08610463437157989, 15.69999999999999929, -27.64615127144129758 ) ) ;
#32729 = CARTESIAN_POINT ( 'NONE',  ( 19.82091636218621389, 12.19999999999998863, -14.40073868116559197 ) ) ;
#32730 = CARTESIAN_POINT ( 'NONE',  ( 7.025853678916867295, 43.50482666574268364, 26.06988505166722803 ) ) ;
#32731 = CARTESIAN_POINT ( 'NONE',  ( -33.58253175000000113, 57.02500000273118275, -10.91162601494193218 ) ) ;
#32732 = CARTESIAN_POINT ( 'NONE',  ( -33.58253175000000113, 49.37500000273120548, 0.000000000000000000 ) ) ;
#32733 = CARTESIAN_POINT ( 'NONE',  ( 18.94512977948575738, 8.424999997268811214, 13.76444248337723408 ) ) ;
#32734 = CARTESIAN_POINT ( 'NONE',  ( 0.000000000000000000, 80.00000000000001421, -32.50000000000000000 ) ) ;
#32735 = CARTESIAN_POINT ( 'NONE',  ( -32.50000000000000000, 6.099999999999980993, 10.55989012756946366 ) ) ;
#32736 = CARTESIAN_POINT ( 'NONE',  ( 19.11951029504763611, 52.10975666759065206, -19.06425588902591173 ) ) ;
#32737 = CARTESIAN_POINT ( 'NONE',  ( 22.63754132413425069, 16.99999999999998934, 6.041913861037119915 ) ) ;
#32738 = DIRECTION ( 'NONE',  ( 0.000000000000000000, 0.000000000000000000, -1.000000000000000000 ) ) ;
#32739 = CARTESIAN_POINT ( 'NONE',  ( -33.58253175000000113, 19.12500000273119483, 0.000000000000000000 ) ) ;
#32740 = DIRECTION ( 'NONE',  ( 0.000000000000000000, 0.000000000000000000, -1.000000000000000000 ) ) ;
#32741 = CARTESIAN_POINT ( 'NONE',  ( -2.375766604868045029, 77.80125428700921475, -14.99999999999999822 ) ) ;
#32742 = CARTESIAN_POINT ( 'NONE',  ( -4.223320258572819786E-15, 13.50000000000000355, 24.50000000000000000 ) ) ;
#32743 = CARTESIAN_POINT ( 'NONE',  ( -20.47846945139866648, 64.70274333240935505, 20.53372385742108008 ) ) ;
#32744 = CARTESIAN_POINT ( 'NONE',  ( -10.04305231718578462, 48.90000000546239534, 30.90933677959249337 ) ) ;
#32745 = CARTESIAN_POINT ( 'NONE',  ( 32.50000000000000000, 11.09999999999999787, -10.55989012756945833 ) ) ;
#32746 = CARTESIAN_POINT ( 'NONE',  ( -27.16883889988623935, 35.32500000273120122, 19.73931689729374739 ) ) ;
#32747 = CARTESIAN_POINT ( 'NONE',  ( -13.97622843553588901, 24.74739583333332504, 24.20753774853756823 ) ) ;
#32748 = EDGE_LOOP ( 'NONE', ( #30519, #19982, #8671, #3363 ) ) ;
#32749 = CARTESIAN_POINT ( 'NONE',  ( 20.75514604977248467, 76.42500000273118133, -28.56700777964554305 ) ) ;
#32750 = CARTESIAN_POINT ( 'NONE',  ( 20.50609665440969565, 43.79687500000000000, -20.50609665441004736 ) ) ;
#32751 = VECTOR ( 'NONE', #1503, 1000.000000000000000 ) ;
#32752 = DIRECTION ( 'NONE',  ( 0.000000000000000000, 1.000000000000000000, 0.000000000000000000 ) ) ;
#32753 = EDGE_LOOP ( 'NONE', ( #14790, #4108 ) ) ;
#32754 = CARTESIAN_POINT ( 'NONE',  ( 28.00173670424549499, 49.24517333425730925, 7.543491769121417612 ) ) ;
#32755 = CARTESIAN_POINT ( 'NONE',  ( -26.29305231718579350, 12.30000000546237260, -19.10302069950537884 ) ) ;
#32756 = CARTESIAN_POINT ( 'NONE',  ( 26.00068869287340334, 64.56510416666667140, -15.01150461594642316 ) ) ;
#32757 = CARTESIAN_POINT ( 'NONE',  ( 5.779280353836490358E-15, 20.49999999999999645, 32.49999999999999289 ) ) ;
#32758 = CARTESIAN_POINT ( 'NONE',  ( 33.58253175000000113, 40.37500000273119838, -4.112674001490185761E-15 ) ) ;
#32759 = CARTESIAN_POINT ( 'NONE',  ( 32.50000000000000000, 47.60000000546239818, -10.55989012756945833 ) ) ;
#32760 = CARTESIAN_POINT ( 'NONE',  ( -9.270509831248425314, 81.69999999999998863, -12.75976212528059861 ) ) ;
#32761 = CARTESIAN_POINT ( 'NONE',  ( 33.58253175000000113, 28.12500000273118772, -4.112674001490185761E-15 ) ) ;
#32762 = CARTESIAN_POINT ( 'NONE',  ( -33.58253175000000113, 57.27500000273120406, -10.91162601494193218 ) ) ;
#32763 = SURFACE_SIDE_STYLE ('',( #16498 ) ) ;
#32764 = EDGE_CURVE ( 'NONE', #19947, #33131, #5634, .T. ) ;
#32765 = CARTESIAN_POINT ( 'NONE',  ( 26.29305231718578995, 35.19999999999999574, -19.10302069950538240 ) ) ;
#32766 = CARTESIAN_POINT ( 'NONE',  ( -20.08610463437157989, 33.70000000000001705, -27.64615127144129758 ) ) ;
#32767 = CARTESIAN_POINT ( 'NONE',  ( -7.236395654485763274, 10.02499999726880198, 22.27133577429736633 ) ) ;
#32768 = CARTESIAN_POINT ( 'NONE',  ( -33.58253175000000113, 77.02500000273118985, -10.91162601494193218 ) ) ;
#32769 = CARTESIAN_POINT ( 'NONE',  ( 23.09401076758502569, 86.00000000000001421, -6.857326241137392698E-15 ) ) ;
#32770 = CARTESIAN_POINT ( 'NONE',  ( 13.91746824999999887, 78.37500000273116996, -1.704398294459741270E-15 ) ) ;
#32771 = CARTESIAN_POINT ( 'NONE',  ( -27.16883889988624290, 65.17500000273118133, -19.73931689729374028 ) ) ;
#32772 = CARTESIAN_POINT ( 'NONE',  ( -15.00000000000000000, 80.25000000546239676, 0.000000000000000000 ) ) ;
#32773 = LINE ( 'NONE', #12364, #2978 ) ;
#32774 = CARTESIAN_POINT ( 'NONE',  ( 19.82091636218621034, 3.549999994537617276, 14.40073868116559730 ) ) ;
#32775 = CARTESIAN_POINT ( 'NONE',  ( 26.06988505166735592, 11.43267333425730925, 7.025853678916393896 ) ) ;
#32776 = CARTESIAN_POINT ( 'NONE',  ( -4.635254915624208216, 74.65000000546240244, 14.26584774442730463 ) ) ;
#32777 = CARTESIAN_POINT ( 'NONE',  ( -20.75514604977248112, 45.42500000273119554, 28.56700777964554661 ) ) ;
#32778 = CARTESIAN_POINT ( 'NONE',  ( 33.58253175000000113, 6.375000002731182391, -4.112674001490185761E-15 ) ) ;
#32779 = CARTESIAN_POINT ( 'NONE',  ( -27.16883889988623935, 53.57500000273117280, 19.73931689729374739 ) ) ;
#32780 = CARTESIAN_POINT ( 'NONE',  ( 26.07999730980490227, 54.68229166666665719, 6.988114217767821046 ) ) ;
#32781 = CARTESIAN_POINT ( 'NONE',  ( 0.04044903254992426173, 37.93006916759064495, -30.02300923189239867 ) ) ;
#32782 = CARTESIAN_POINT ( 'NONE',  ( 7.543491769121922985, 26.31732666574268364, 28.00173670424535644 ) ) ;
#32783 = CARTESIAN_POINT ( 'NONE',  ( -32.50000000000000000, 64.60000000546237686, 10.55989012756946366 ) ) ;
#32784 = EDGE_CURVE ( 'NONE', #2770, #18447, #29314, .T. ) ;
#32785 = CARTESIAN_POINT ( 'NONE',  ( 4.300734207923761154, 73.47500000273116427, 13.23629886949340495 ) ) ;
#32786 = CARTESIAN_POINT ( 'NONE',  ( 13.94119854578893580, 52.52826416574268364, -24.22776226481265383 ) ) ;
#32787 = LINE ( 'NONE', #9118, #7242 ) ;
#32788 = CARTESIAN_POINT ( 'NONE',  ( -7.570916362186210335, 4.349999994537640191, -23.30088464923126779 ) ) ;
#32789 = ORIENTED_EDGE ( 'NONE', *, *, #4651, .T. ) ;
#32790 = CARTESIAN_POINT ( 'NONE',  ( -2.162160676586881955E-15, 38.87500000273120548, -35.31076352940723240 ) ) ;
#32791 = CARTESIAN_POINT ( 'NONE',  ( -23.41746825000000243, 2.224999997268808816, 7.608796670333725309 ) ) ;
#32792 = CARTESIAN_POINT ( 'NONE',  ( -26.29305231718579350, 30.30000000546238681, -19.10302069950537884 ) ) ;
#32793 = VERTEX_POINT ( 'NONE', #8868 ) ;
#32794 = CARTESIAN_POINT ( 'NONE',  ( -15.01150461594642138, 32.76822916666666430, -26.00068869287340334 ) ) ;
#32795 = ORIENTED_EDGE ( 'NONE', *, *, #26764, .F. ) ;
#32796 = CARTESIAN_POINT ( 'NONE',  ( -26.29305231718579350, 74.30000000546237970, -19.10302069950537884 ) ) ;
#32797 = CARTESIAN_POINT ( 'NONE',  ( -2.162160676586881955E-15, 48.62500000273118417, -35.31076352940723240 ) ) ;
#32798 = CARTESIAN_POINT ( 'NONE',  ( -15.01150461594642138, 60.26822916666665009, -26.00068869287340334 ) ) ;
#32799 = CARTESIAN_POINT ( 'NONE',  ( 26.29305231718578995, 13.70000000546239782, -19.10302069950538240 ) ) ;
#32800 = CARTESIAN_POINT ( 'NONE',  ( -2.162160676586882350E-15, 66.62500000273119838, -35.31076352940722529 ) ) ;
#32801 = CARTESIAN_POINT ( 'NONE',  ( -14.47279130897152299, 16.42499999726882720, 19.92008829642072243 ) ) ;
#32802 = CARTESIAN_POINT ( 'NONE',  ( 20.08610463437158344, 54.69999999999998863, 27.64615127144129403 ) ) ;
#32803 = LINE ( 'NONE', #9296, #32909 ) ;
#32804 = CARTESIAN_POINT ( 'NONE',  ( 10.37757302488624767, 17.97500000273119625, 31.93888565452638417 ) ) ;
#32805 = CARTESIAN_POINT ( 'NONE',  ( 5.779280353836490358E-15, 5.000000005462372776, 32.49999999999999289 ) ) ;
#32806 = CARTESIAN_POINT ( 'NONE',  ( -26.09010956794245217, 24.02565999907602290, -6.950374756619243755 ) ) ;
#32807 = CARTESIAN_POINT ( 'NONE',  ( 13.91746824999999532, 71.97500000273120691, -4.522059556121118540 ) ) ;
#32808 = CARTESIAN_POINT ( 'NONE',  ( 15.00000000000000000, 75.25000000546239676, -1.836970198721029589E-15 ) ) ;
#32809 = DIRECTION ( 'NONE',  ( 0.000000000000000000, 0.000000000000000000, 1.000000000000000000 ) ) ;
#32810 = CARTESIAN_POINT ( 'NONE',  ( -32.50000000000000000, 5.900000000000002132, -10.55989012756945478 ) ) ;
#32811 = ORIENTED_EDGE ( 'NONE', *, *, #24665, .T. ) ;
#32812 = CARTESIAN_POINT ( 'NONE',  ( -14.47279130897152122, 6.424999997268821872, 19.92008829642072243 ) ) ;
#32813 = CARTESIAN_POINT ( 'NONE',  ( -1.778240108872766143E-15, 40.00000000546237544, -32.49999999999999289 ) ) ;
#32814 = CARTESIAN_POINT ( 'NONE',  ( 27.95245687107222921, 37.35156249999997868, -2.463307335887066074E-13 ) ) ;
#32815 = CARTESIAN_POINT ( 'NONE',  ( -2.162160676586881955E-15, 68.62500000273119838, -35.31076352940723240 ) ) ;
#32816 = B_SPLINE_CURVE_WITH_KNOTS ( 'NONE', 3,
 ( #21913, #29955, #21584, #1116, #16437, #19672, #6288, #19012, #3547, #11601, #16764, #3386, #16599, #16271, #29783, #32199, #26889, #22082, #24322, #11115, #14019, #24811, #19508, #6459, #32030, #27391, #795, #13691, #8527, #8693, #956, #13856, #24642, #16933, #32526, #19177, #3880, #14353 ),
 .UNSPECIFIED., .F., .F.,
 ( 4, 2, 2, 2, 2, 2, 2, 2, 2, 2, 2, 2, 2, 2, 2, 2, 2, 2, 4 ),
 ( 0.000000000000000000, 0.001480261321998002991, 0.002960522643996005981, 0.005921045287992017167, 0.008881567931988023148, 0.01036182925398602614, 0.01184209057598402913, 0.01776313586397604283, 0.01924339718597405449, 0.02072365850797205922, 0.02368418115196807908, 0.02664470379596409547, 0.02960522643996011533, 0.03256574908395613172, 0.03404601040595413991, 0.03552627172795214117, 0.04144731701594418782, 0.04440783965994021115, 0.04736836230393623448 ),
 .UNSPECIFIED. ) ;
#32817 = CARTESIAN_POINT ( 'NONE',  ( -2.162160676586881955E-15, 26.87500000273116996, -35.31076352940723240 ) ) ;
#32818 = CARTESIAN_POINT ( 'NONE',  ( 20.75514604977248467, 14.67500000273117955, -28.56700777964554305 ) ) ;
#32819 = CARTESIAN_POINT ( 'NONE',  ( -20.75514604977248112, 9.675000002731193760, 28.56700777964554661 ) ) ;
#32820 = CARTESIAN_POINT ( 'NONE',  ( -19.06425588902591173, 65.00038166759063074, -19.11951029504763611 ) ) ;
#32821 = EDGE_CURVE ( 'NONE', #6391, #11531, #11773, .T. ) ;
#32822 = CARTESIAN_POINT ( 'NONE',  ( -26.00068869287368756, 49.66927083333330728, -15.01150461594595775 ) ) ;
#32823 = CARTESIAN_POINT ( 'NONE',  ( 5.147494310547426899, 3.448745718453164244, -32.50000000000000000 ) ) ;
#32824 = CARTESIAN_POINT ( 'NONE',  ( -32.50000000000000000, 49.89999999999999147, -10.55989012756945478 ) ) ;
#32825 = CARTESIAN_POINT ( 'NONE',  ( 24.50000000000000000, 7.749999994537626336, 0.000000000000000000 ) ) ;
#32826 = CARTESIAN_POINT ( 'NONE',  ( 6.486482029760648627E-15, 51.62500000273120548, 35.31076352940722529 ) ) ;
#32827 = CARTESIAN_POINT ( 'NONE',  ( -23.41746825000000243, 5.524999997268821517, -7.608796670333730638 ) ) ;
#32828 = EDGE_CURVE ( 'NONE', #9459, #29733, #11572, .T. ) ;
#32829 = ORIENTED_EDGE ( 'NONE', *, *, #5711, .T. ) ;
#32830 = CARTESIAN_POINT ( 'NONE',  ( 20.75514604977248467, 62.67500000273117422, -28.56700777964554305 ) ) ;
#32831 = CARTESIAN_POINT ( 'NONE',  ( 5.779280353836490358E-15, 18.50000000000000000, 32.49999999999999289 ) ) ;
#32832 = CARTESIAN_POINT ( 'NONE',  ( 23.41746825000000243, 14.72499999726881903, -7.608796670333727974 ) ) ;
#32833 = CARTESIAN_POINT ( 'NONE',  ( -0.04044903254992426173, 36.21131916759064495, 27.95245687107223276 ) ) ;
#32834 = ORIENTED_EDGE ( 'NONE', *, *, #10703, .F. ) ;
#32835 = CARTESIAN_POINT ( 'NONE',  ( -10.37757302488624411, 30.72500000273119269, -31.93888565452638417 ) ) ;
#32836 = CARTESIAN_POINT ( 'NONE',  ( -15.00000000000010125, 74.09999999999999432, 4.873795443493460944 ) ) ;
#32837 = ORIENTED_EDGE ( 'NONE', *, *, #25382, .T. ) ;
#32838 = CARTESIAN_POINT ( 'NONE',  ( -15.01150461594642138, 56.83072916666665009, -26.00068869287340334 ) ) ;
#32839 = CARTESIAN_POINT ( 'NONE',  ( -33.58253175000000113, 57.47500000273119269, 10.91162601494193929 ) ) ;
#32840 = CARTESIAN_POINT ( 'NONE',  ( -2.375766604868045029, 75.55125428154684641, -14.99999999999999822 ) ) ;
#32841 = CARTESIAN_POINT ( 'NONE',  ( -10.37757302488624411, 66.72500000273117848, -31.93888565452638417 ) ) ;
#32842 = CARTESIAN_POINT ( 'NONE',  ( -15.01150461594595775, 28.18489583333332860, 26.00068869287368756 ) ) ;
#32843 = CARTESIAN_POINT ( 'NONE',  ( 24.50000000000000355, 9.900000000000007461, 7.960532557706212486 ) ) ;
#32844 = CARTESIAN_POINT ( 'NONE',  ( -10.37757302488624411, 4.975000002731183812, -31.93888565452638417 ) ) ;
#32845 = CARTESIAN_POINT ( 'NONE',  ( -2.162160676586881955E-15, 12.62500000273118772, -35.31076352940723240 ) ) ;
#32846 = CARTESIAN_POINT ( 'NONE',  ( -8.960552108402744065E-16, 74.37500000273118417, -14.63369212191046209 ) ) ;
#32847 = CARTESIAN_POINT ( 'NONE',  ( -14.97647472619899389, 43.93451416574269075, 26.02091320914878025 ) ) ;
#32848 = CARTESIAN_POINT ( 'NONE',  ( -15.00000000000000000, 80.00000000000001421, 0.000000000000000000 ) ) ;
#32849 = CARTESIAN_POINT ( 'NONE',  ( 20.50609665440969565, 57.54687500000000000, -20.50609665441004736 ) ) ;
#32850 = CARTESIAN_POINT ( 'NONE',  ( 1.577395562988744260E-15, 4.249999994537624559, -25.76082449383753925 ) ) ;
#32851 = CARTESIAN_POINT ( 'NONE',  ( -15.00000000000000000, 76.15000000546235981, -4.873795443493594171 ) ) ;
#32852 = CARTESIAN_POINT ( 'NONE',  ( 24.18731323226221974, 66.56472249907604066, -14.01125832528328985 ) ) ;
#32853 = CARTESIAN_POINT ( 'NONE',  ( 6.486482029760649416E-15, 37.62500000273118417, 35.31076352940723240 ) ) ;
#32854 = CARTESIAN_POINT ( 'NONE',  ( 11.25946833292375793, 77.67500000273119554, 8.180482586598731842 ) ) ;
#32855 = CARTESIAN_POINT ( 'NONE',  ( -27.16883889988623935, 45.57500000273119412, 19.73931689729374739 ) ) ;
#32856 = CARTESIAN_POINT ( 'NONE',  ( 6.486482029760648627E-15, 27.87500000273120193, 35.31076352940722529 ) ) ;
#32857 = CARTESIAN_POINT ( 'NONE',  ( -32.50000000000000000, 12.50000000546236478, 0.000000000000000000 ) ) ;
#32858 = DIRECTION ( 'NONE',  ( 0.000000000000000000, -1.000000000000000000, 0.000000000000000000 ) ) ;
#32859 = CARTESIAN_POINT ( 'NONE',  ( 32.50000000000000000, 33.10000000000000142, -10.55989012756945833 ) ) ;
#32860 = CARTESIAN_POINT ( 'NONE',  ( 26.29305231718578995, 67.20000000000000284, -19.10302069950538240 ) ) ;
#32861 = CARTESIAN_POINT ( 'NONE',  ( 14.47279130897151944, 12.92499999726881832, -19.92008829642072598 ) ) ;
#32862 = CARTESIAN_POINT ( 'NONE',  ( 14.97647472619900455, 21.59076416574269430, -26.02091320914876960 ) ) ;
#32863 = CARTESIAN_POINT ( 'NONE',  ( 18.94512977948575738, 4.924999997268808549, 13.76444248337723408 ) ) ;
#32864 = CARTESIAN_POINT ( 'NONE',  ( -13.94119854578892514, 40.49701416574269786, 24.22776226481266448 ) ) ;
#32865 = DIRECTION ( 'NONE',  ( 0.000000000000000000, 0.000000000000000000, -1.000000000000000000 ) ) ;
#32866 = CARTESIAN_POINT ( 'NONE',  ( -27.16883889988623935, 15.32500000273118168, 19.73931689729374739 ) ) ;
#32867 = CARTESIAN_POINT ( 'NONE',  ( -7.236395654485757944, 11.72499999726880837, -22.27133577429736988 ) ) ;
#32868 = CARTESIAN_POINT ( 'NONE',  ( 6.988114217768294445, 58.69270833333332860, 26.07999730980477437 ) ) ;
#32869 = ORIENTED_EDGE ( 'NONE', *, *, #28667, .T. ) ;
#32870 = CARTESIAN_POINT ( 'NONE',  ( -27.16883889988624290, 52.92500000273118843, -19.73931689729374028 ) ) ;
#32871 = CARTESIAN_POINT ( 'NONE',  ( -33.58253175000000113, 23.37500000273119838, 0.000000000000000000 ) ) ;
#32872 = ORIENTED_EDGE ( 'NONE', *, *, #24746, .T. ) ;
#32873 = CARTESIAN_POINT ( 'NONE',  ( 7.505752307973351023, 31.19270833333333215, 28.01184896238290278 ) ) ;
#32874 = CARTESIAN_POINT ( 'NONE',  ( -30.02300923189239867, 30.19569416759064140, -0.04044903254991731589 ) ) ;
#32875 = CARTESIAN_POINT ( 'NONE',  ( -24.50000000000000000, 3.000000000000002665, -3.000384657911015469E-15 ) ) ;
#32876 = CARTESIAN_POINT ( 'NONE',  ( -7.570916362186215665, 17.14999999453761959, 23.30088464923126423 ) ) ;
#32877 = CARTESIAN_POINT ( 'NONE',  ( 7.236395654485760609, 7.024999997268799312, -22.27133577429736633 ) ) ;
#32878 = CARTESIAN_POINT ( 'NONE',  ( 20.75514604977248467, 20.67500000273119909, -28.56700777964554305 ) ) ;
#32879 = CARTESIAN_POINT ( 'NONE',  ( -20.08610463437156923, 26.80000000546238681, 27.64615127144130113 ) ) ;
#32880 = CARTESIAN_POINT ( 'NONE',  ( 10.04305231718579705, 70.59999999999999432, 30.90933677959248982 ) ) ;
#32881 = DIRECTION ( 'NONE',  ( -1.224646799147353454E-16, 1.000000000000000000, -0.000000000000000000 ) ) ;
#32882 = CARTESIAN_POINT ( 'NONE',  ( -14.97879338252777259, 74.00000000000004263, 0.5967302757886839837 ) ) ;
#32883 = CARTESIAN_POINT ( 'NONE',  ( 15.04653450569292872, 58.84152750092397355, -25.98046417659857710 ) ) ;
#32884 = CARTESIAN_POINT ( 'NONE',  ( -20.75514604977248112, 39.67500000273118133, 28.56700777964554661 ) ) ;
#32885 = CARTESIAN_POINT ( 'NONE',  ( -33.58253175000000113, 53.12500000273119838, 0.000000000000000000 ) ) ;
#32886 = CARTESIAN_POINT ( 'NONE',  ( 28.01184896238290278, 30.33333333333332860, -7.505752307973347470 ) ) ;
#32887 = CARTESIAN_POINT ( 'NONE',  ( -14.47279130897151589, 11.82499999726882578, -19.92008829642072598 ) ) ;
#32888 = CARTESIAN_POINT ( 'NONE',  ( -2.092463501923844636E-15, 15.50000000000000533, -34.17252228774368916 ) ) ;
#32889 = CARTESIAN_POINT ( 'NONE',  ( -1.778240108872766143E-15, 10.00000000546236834, -32.49999999999999289 ) ) ;
#32890 = CARTESIAN_POINT ( 'NONE',  ( 19.11951029504797006, 43.21836833240935505, 19.06425588902558133 ) ) ;
#32891 = CARTESIAN_POINT ( 'NONE',  ( -20.75514604977248112, 55.42500000273119554, 28.56700777964554661 ) ) ;
#32892 = CARTESIAN_POINT ( 'NONE',  ( 33.58253175000000113, 46.37500000273120548, -4.112674001490185761E-15 ) ) ;
#32893 = DIRECTION ( 'NONE',  ( -0.000000000000000000, -1.000000000000000000, -0.000000000000000000 ) ) ;
#32894 = DIRECTION ( 'NONE',  ( -0.000000000000000000, 1.000000000000000000, -0.000000000000000000 ) ) ;
#32895 = DIRECTION ( 'NONE',  ( 0.4999999999999998335, 0.000000000000000000, -0.8660254037844387076 ) ) ;
#32896 = CARTESIAN_POINT ( 'NONE',  ( -13.94119854578936923, 44.51861083425730214, -24.22776226481241224 ) ) ;
#32897 =( BOUNDED_CURVE ( )  B_SPLINE_CURVE ( 2, ( #30508, #12332, #17490, #14570, #4096, #1855, #17151 ),
 .UNSPECIFIED., .F., .T. ) 
 B_SPLINE_CURVE_WITH_KNOTS ( ( 3, 2, 2, 3 ),
 ( 0.000000000000000000, 0.002564102564102564100, 0.005128205128205128201, 0.006410256410256410901 ),
 .UNSPECIFIED. ) 
 CURVE ( )  GEOMETRIC_REPRESENTATION_ITEM ( )  RATIONAL_B_SPLINE_CURVE ( ( 1.000000000000000000, 0.9510565162951535312, 1.000000000000000000, 0.9510565162951535312, 1.000000000000000000, 0.9755282581475768211, 0.9755282581475768211 ) ) 
 REPRESENTATION_ITEM ( '' )  );
#32898 = CARTESIAN_POINT ( 'NONE',  ( -23.91461052556157441, 16.99999999999998579, -4.889261515958251536 ) ) ;
#32899 = FACE_OUTER_BOUND ( 'NONE', #26903, .T. ) ;
#32900 = CARTESIAN_POINT ( 'NONE',  ( 33.58253175000000113, 24.12500000273119838, -4.112674001490185761E-15 ) ) ;
#32901 = CARTESIAN_POINT ( 'NONE',  ( 3.469446951953614189E-15, -45.00000000000000000, 0.000000000000000000 ) ) ;
#32902 = CARTESIAN_POINT ( 'NONE',  ( 26.29305231718578995, 53.20000000000000995, -19.10302069950538240 ) ) ;
#32903 = LINE ( 'NONE', #15083, #11036 ) ;
#32904 = CARTESIAN_POINT ( 'NONE',  ( -20.53372385742107653, 65.56211833240934084, -20.47846945139867003 ) ) ;
#32905 = CARTESIAN_POINT ( 'NONE',  ( 10.04305231718578817, 43.90000000546238823, -30.90933677959249337 ) ) ;
#32906 = EDGE_CURVE ( 'NONE', #11992, #564, #12684, .T. ) ;
#32907 = CARTESIAN_POINT ( 'NONE',  ( 5.147494310547426899, 11.44874571845314293, -32.50000000000000000 ) ) ;
#32908 = CARTESIAN_POINT ( 'NONE',  ( 33.58253175000000823, 34.02500000273118275, 10.91162601494192685 ) ) ;
#32909 = VECTOR ( 'NONE', #6733, 1000.000000000000000 ) ;
#32910 = CARTESIAN_POINT ( 'NONE',  ( -2.428612866367529427E-13, 33.05468750000000000, -27.95245687107222921 ) ) ;
#32911 = EDGE_CURVE ( 'NONE', #21391, #1603, #7396, .T. ) ;
#32912 = CARTESIAN_POINT ( 'NONE',  ( -20.75514604977248823, 68.82500000273118701, -28.56700777964554305 ) ) ;
#32913 = CARTESIAN_POINT ( 'NONE',  ( -7.505752307972844761, 38.35416666666666430, 28.01184896238304134 ) ) ;
#32914 = DIRECTION ( 'NONE',  ( -0.000000000000000000, -1.000000000000000000, -0.000000000000000000 ) ) ;
#32915 = VERTEX_POINT ( 'NONE', #22093 ) ;
#32916 = CARTESIAN_POINT ( 'NONE',  ( 14.97647472619947351, 63.42486083425730925, 26.02091320914850314 ) ) ;
#32917 = CARTESIAN_POINT ( 'NONE',  ( -26.09010956794232428, 64.42746500092397355, 6.950374756619732253 ) ) ;
#32918 = CARTESIAN_POINT ( 'NONE',  ( -10.04305231718578462, 8.900000005462358033, 30.90933677959249337 ) ) ;
#32919 = CARTESIAN_POINT ( 'NONE',  ( -7.505752307972844761, 65.85416666666665719, 28.01184896238304134 ) ) ;
#32920 = CARTESIAN_POINT ( 'NONE',  ( 0.000000000000000000, 16.99999999999998579, -24.50000000000000000 ) ) ;
#32921 = CARTESIAN_POINT ( 'NONE',  ( -20.75514604977248112, 41.67500000273117422, 28.56700777964554661 ) ) ;
#32922 = CARTESIAN_POINT ( 'NONE',  ( 26.29305231718579350, 45.30000000546238681, 19.10302069950537529 ) ) ;
#32923 = CARTESIAN_POINT ( 'NONE',  ( 13.91746824999999532, 74.47500000273120691, -4.522059556121118540 ) ) ;
#32924 = CARTESIAN_POINT ( 'NONE',  ( -33.58253175000000113, 27.02500000273119696, -10.91162601494193218 ) ) ;
#32925 = CARTESIAN_POINT ( 'NONE',  ( 26.29305231718579350, 31.30000000546237615, 19.10302069950537529 ) ) ;
#32926 = CARTESIAN_POINT ( 'NONE',  ( 6.486482029760649416E-15, 57.87500000273117706, 35.31076352940723240 ) ) ;
#32927 = FILL_AREA_STYLE ('',( #28144 ) ) ;
#32928 = CARTESIAN_POINT ( 'NONE',  ( 32.50000000000000000, 33.00000000000001421, -3.980102097228898626E-15 ) ) ;
#32929 = CARTESIAN_POINT ( 'NONE',  ( 20.08610463437158344, 34.70000000000001705, 27.64615127144129403 ) ) ;
#32930 = CARTESIAN_POINT ( 'NONE',  ( -18.94512977948576093, 17.82499999726880446, 13.76444248337722698 ) ) ;
#32931 = CARTESIAN_POINT ( 'NONE',  ( -33.58253175000000113, 75.22500000273119269, 10.91162601494193929 ) ) ;
#32932 = LINE ( 'NONE', #9432, #12377 ) ;
#32933 = AXIS2_PLACEMENT_3D ( 'NONE', #17906, #22869, #30404 ) ;
#32934 = CIRCLE ( 'NONE', #19270, 27.00000000000000000 ) ;
#32935 = CARTESIAN_POINT ( 'NONE',  ( -8.601468415847518756, 79.07500000273118701, -11.83890561707634603 ) ) ;
#32936 = CARTESIAN_POINT ( 'NONE',  ( -20.75514604977248112, 67.67500000273116711, 28.56700777964554661 ) ) ;
#32937 = CARTESIAN_POINT ( 'NONE',  ( 9.270509831248425314, 76.95000000546237118, 12.75976212528059683 ) ) ;
#32938 = LINE ( 'NONE', #27472, #24334 ) ;
#32939 = CARTESIAN_POINT ( 'NONE',  ( -19.82091636218621034, 6.549999994537619941, -14.40073868116559552 ) ) ;
#32940 = CARTESIAN_POINT ( 'NONE',  ( -19.11951029504763611, 22.89100666759064495, 19.06425588902592239 ) ) ;
#32941 = CARTESIAN_POINT ( 'NONE',  ( 3.880418787951140036, 8.198745712990779921, -24.49999999999999645 ) ) ;
#32942 = CARTESIAN_POINT ( 'NONE',  ( -33.58253175000000113, 41.22500000273118559, 10.91162601494193929 ) ) ;
#32943 = CARTESIAN_POINT ( 'NONE',  ( -33.58253175000000113, 3.375000002731193049, 0.000000000000000000 ) ) ;
#32944 = CARTESIAN_POINT ( 'NONE',  ( 10.37757302488624767, 53.97500000273118559, 31.93888565452638417 ) ) ;
#32945 = CARTESIAN_POINT ( 'NONE',  ( -26.02091320914849959, 47.09673583425730214, 14.97647472619947528 ) ) ;
#32946 = CARTESIAN_POINT ( 'NONE',  ( -28.00173670424535644, 34.05170166574267654, 7.543491769121936308 ) ) ;
#32947 = CARTESIAN_POINT ( 'NONE',  ( 26.29305231718579350, 63.30000000546235839, 19.10302069950537529 ) ) ;
#32948 = CARTESIAN_POINT ( 'NONE',  ( -11.25946833292375793, 73.07500000273120122, 8.180482586598737171 ) ) ;
#32949 = CARTESIAN_POINT ( 'NONE',  ( 24.18731323226221974, 63.12722249907601224, -14.01125832528328985 ) ) ;
#32950 = CARTESIAN_POINT ( 'NONE',  ( -10.04305231718578462, 54.39999999999999147, 30.90933677959249337 ) ) ;
#32951 = B_SPLINE_CURVE_WITH_KNOTS ( 'NONE', 3,
 ( #33288, #20435, #15284, #17345, #14767, #25744, #12185, #2226, #7034, #4125, #14600, #17517, #27978, #4463, #324, #10811, #21291, #8060, #28823, #18209, #31731, #18545, #23352, #8222, #4980, #26087, #8390, #28991, #18716, #2745, #13562, #29152, #33814, #28652, #24025, #31230, #5658, #5321, #2407, #15635, #21119, #12875, #494, #10977 ),
 .UNSPECIFIED., .F., .F.,
 ( 4, 2, 2, 2, 2, 2, 2, 2, 2, 2, 2, 2, 2, 2, 2, 2, 2, 2, 2, 2, 2, 4 ),
 ( 0.000000000000000000, 0.004057857163981326565, 0.008115714327962653130, 0.01217357149194398663, 0.01420250007393465339, 0.01623142865592532014, 0.02028928581990665364, 0.02231821440189732039, 0.02434714298388798714, 0.02840500014786932065, 0.03246285731185065415, 0.03652071447583198766, 0.03854964305782265094, 0.04057857163981331422, 0.04463642880379464078, 0.04869428596777596735, 0.05072321454976663063, 0.05275214313175728698, 0.05681000029573861354, 0.05883892887772927682, 0.06086785745971993317, 0.06492571462370128055 ),
 .UNSPECIFIED. ) ;
#32952 = CARTESIAN_POINT ( 'NONE',  ( 10.04305231718578817, 75.90000000546237402, -30.90933677959249337 ) ) ;
#32953 = CARTESIAN_POINT ( 'NONE',  ( 28.01184896238304134, 13.43229166666666607, 7.505752307972846538 ) ) ;
#32954 = CARTESIAN_POINT ( 'NONE',  ( -10.37757302488624411, 40.97500000273117138, -31.93888565452638417 ) ) ;
#32955 = CARTESIAN_POINT ( 'NONE',  ( 7.236395654485755280, 2.724999997268801266, 22.27133577429736988 ) ) ;
#32956 = EDGE_LOOP ( 'NONE', ( #24134, #6912, #26319, #12735 ) ) ;
#32957 = AXIS2_PLACEMENT_3D ( 'NONE', #27889, #20342, #4373 ) ;
#32958 = CARTESIAN_POINT ( 'NONE',  ( -2.092463501923844636E-15, 28.00000000546237544, -34.17252228774368916 ) ) ;
#32959 = ORIENTED_EDGE ( 'NONE', *, *, #2231, .F. ) ;
#32960 = CARTESIAN_POINT ( 'NONE',  ( -28.01184896238304134, 35.77604166666666430, -7.505752307972844761 ) ) ;
#32961 = CARTESIAN_POINT ( 'NONE',  ( -2.092463501923844636E-15, 64.00000000546236834, -34.17252228774368916 ) ) ;
#32962 = ORIENTED_EDGE ( 'NONE', *, *, #13074, .F. ) ;
#32963 = CARTESIAN_POINT ( 'NONE',  ( -32.50000000000000000, 55.90000000000000568, -10.55989012756945300 ) ) ;
#32964 = CARTESIAN_POINT ( 'NONE',  ( 27.16883889988624290, 47.92500000273120264, 19.73931689729373673 ) ) ;
#32965 = CARTESIAN_POINT ( 'NONE',  ( 10.04305231718579705, 55.10000000546239107, 30.90933677959248982 ) ) ;
#32966 = CARTESIAN_POINT ( 'NONE',  ( -7.505752307973343918, 63.84895833333332860, -28.01184896238290989 ) ) ;
#32967 = CARTESIAN_POINT ( 'NONE',  ( -10.04305231718579172, 10.10000000546237864, -30.90933677959248982 ) ) ;
#32968 = CARTESIAN_POINT ( 'NONE',  ( -1.089172066684569321E-14, 78.49999999999998579, 15.00000000000000000 ) ) ;
#32969 = CARTESIAN_POINT ( 'NONE',  ( -7.236395654485757944, 15.72499999726881192, -22.27133577429736988 ) ) ;
#32970 = CARTESIAN_POINT ( 'NONE',  ( 26.29305231718578995, 55.19999999999999574, -19.10302069950538240 ) ) ;
#32971 = CARTESIAN_POINT ( 'NONE',  ( 23.41746824999999887, 0.6249999972688102812, 0.000000000000000000 ) ) ;
#32972 = CARTESIAN_POINT ( 'NONE',  ( -33.58253175000000113, 17.47500000273117848, 10.91162601494193929 ) ) ;
#32973 = CARTESIAN_POINT ( 'NONE',  ( -19.82091636218621034, 6.800000000000000711, -14.40073868116559552 ) ) ;
#32974 = CARTESIAN_POINT ( 'NONE',  ( 0.04044903255044120238, 26.46055583240935505, 27.95245687107223276 ) ) ;
#32975 = CARTESIAN_POINT ( 'NONE',  ( -8.601468415847515203, 75.17500000273118133, 11.83890561707634959 ) ) ;
#32976 = CARTESIAN_POINT ( 'NONE',  ( -5.147494310547430452, 55.55125428154683220, -32.49999999999999289 ) ) ;
#32977 = CARTESIAN_POINT ( 'NONE',  ( -32.50000000000000000, 21.90000000000000568, -10.55989012756945300 ) ) ;
#32978 = CARTESIAN_POINT ( 'NONE',  ( -32.50000000000000000, 2.000000000000001776, 0.000000000000000000 ) ) ;
#32979 = ORIENTED_EDGE ( 'NONE', *, *, #26764, .T. ) ;
#32980 = CARTESIAN_POINT ( 'NONE',  ( -23.41746825000000598, 6.224999997268799490, 7.608796670333726198 ) ) ;
#32981 = CARTESIAN_POINT ( 'NONE',  ( 23.09401076758502569, 96.00000000000002842, -6.857326241137392698E-15 ) ) ;
#32982 = CARTESIAN_POINT ( 'NONE',  ( 26.07999730980477437, 47.52083333333332860, -6.988114217768290004 ) ) ;
#32983 = CARTESIAN_POINT ( 'NONE',  ( 6.486482029760649416E-15, 61.62500000273118417, 35.31076352940723240 ) ) ;
#32984 = CARTESIAN_POINT ( 'NONE',  ( 20.75514604977249178, 26.07500000273119767, 28.56700777964553950 ) ) ;
#32985 = CARTESIAN_POINT ( 'NONE',  ( -33.58253175000000113, 11.37500000273118594, 0.000000000000000000 ) ) ;
#32986 = CARTESIAN_POINT ( 'NONE',  ( 27.16883889988623935, 2.575000002731198112, -19.73931689729374384 ) ) ;
#32987 = CARTESIAN_POINT ( 'NONE',  ( 7.468012846824777284, 12.00559000092397532, 28.02196122052045268 ) ) ;
#32988 = CARTESIAN_POINT ( 'NONE',  ( 7.505752307973351023, 62.13020833333334281, 28.01184896238290278 ) ) ;
#32989 = CARTESIAN_POINT ( 'NONE',  ( 26.29305231718579350, 44.79999999999999005, 19.10302069950537529 ) ) ;
#32990 = CARTESIAN_POINT ( 'NONE',  ( 33.58253175000000113, 52.22500000273118559, -10.91162601494193574 ) ) ;
#32991 = CARTESIAN_POINT ( 'NONE',  ( -7.236395654485763274, 4.024999997268824181, 22.27133577429736633 ) ) ;
#32992 = DIRECTION ( 'NONE',  ( 0.000000000000000000, -0.000000000000000000, 1.000000000000000000 ) ) ;
#32993 = ORIENTED_EDGE ( 'NONE', *, *, #1170, .F. ) ;
#32994 = CARTESIAN_POINT ( 'NONE',  ( -20.75514604977248112, 61.67500000273117422, 28.56700777964554661 ) ) ;
#32995 = CARTESIAN_POINT ( 'NONE',  ( -32.50000000000000000, 2.099999999999991651, 10.55989012756946366 ) ) ;
#32996 = VECTOR ( 'NONE', #6668, 1000.000000000000000 ) ;
#32997 = CARTESIAN_POINT ( 'NONE',  ( -7.236395654485757944, 11.22499999726880837, -22.27133577429736988 ) ) ;
#32998 = CARTESIAN_POINT ( 'NONE',  ( -19.11951029504763611, 36.64100666759062364, 19.06425588902592239 ) ) ;
#32999 = ORIENTED_EDGE ( 'NONE', *, *, #5476, .T. ) ;
#33000 = CARTESIAN_POINT ( 'NONE',  ( -10.37757302488623701, 33.52500000273118985, 31.93888565452638417 ) ) ;
#33001 = AXIS2_PLACEMENT_3D ( 'NONE', #22511, #30569, #9466 ) ;
#33002 = CARTESIAN_POINT ( 'NONE',  ( 24.50000000000000000, 5.899999999999987921, 7.960532557706212486 ) ) ;
#33003 = ORIENTED_EDGE ( 'NONE', *, *, #5476, .F. ) ;
#33005 = CARTESIAN_POINT ( 'NONE',  ( 7.505752307972854531, 57.26041666666666430, -28.01184896238303423 ) ) ;
#33004 =( BOUNDED_CURVE ( )  B_SPLINE_CURVE ( 2, ( #24554, #16843, #3624, #14098, #1370, #24886, #3957, #19748, #14431, #30031, #21988, #6365, #11347, #8935, #11677, #11846, #19415, #3791, #32436, #9102, #1027, #30366, #27299, #32935, #11508, #27638, #22325, #6192, #9433, #32271, #32770, #14262, #29864, #6536, #19583, #19247, #30196, #19918, #24720, #17009, #29686, #6697, #1196, #14601, #17180, #8764, #25058, #16673, #22160, #32603, #12015, #27468, #22484, #6867, #17346, #27809, #4293, #24392, #866, #18040, #4466, #4806, #25579, #15285, #23353, #2227, #2409, #33289, #33110, #7382, #27979, #4636, #12704, #17518, #9961 ),
 .UNSPECIFIED., .F., .T. ) 
 B_SPLINE_CURVE_WITH_KNOTS ( ( 3, 2, 2, 2, 2, 2, 2, 2, 2, 2, 2, 2, 2, 2, 2, 2, 2, 2, 2, 2, 2, 2, 2, 2, 2, 2, 2, 2, 2, 2, 2, 2, 2, 2, 2, 2, 2, 3 ),
 ( 0.000000000000000000, 0.02000000000000000042, 0.04000000000000000083, 0.05999999999999999778, 0.08000000000000000167, 0.1000000000000000056, 0.1199999999999999956, 0.1400000000000000133, 0.1600000000000000033, 0.1799999999999999933, 0.2000000000000000111, 0.2200000000000000011, 0.2399999999999999911, 0.2600000000000000089, 0.2800000000000000266, 0.2999999999999999889, 0.3200000000000000067, 0.3400000000000000244, 0.3599999999999999867, 0.3800000000000000044, 0.4000000000000000222, 0.4199999999999999845, 0.4400000000000000022, 0.4600000000000000200, 0.4799999999999999822, 0.5000000000000000000, 0.5200000000000000178, 0.5400000000000000355, 0.5600000000000000533, 0.5799999999999999600, 0.5999999999999999778, 0.6199999999999999956, 0.6400000000000000133, 0.6600000000000000311, 0.6800000000000000488, 0.6999999999999999556, 0.7199999999999999734, 0.7374174419963591687 ),
 .UNSPECIFIED. ) 
 CURVE ( )  GEOMETRIC_REPRESENTATION_ITEM ( )  RATIONAL_B_SPLINE_CURVE ( ( 1.000000000000000000, 0.9510565162951535312, 1.000000000000000000, 0.9510565162951535312, 1.000000000000000000, 0.9510565162951535312, 1.000000000000000000, 0.9510565162951535312, 1.000000000000000000, 0.9510565162951535312, 1.000000000000000000, 0.9510565162951535312, 1.000000000000000000, 0.9510565162951535312, 1.000000000000000000, 0.9510565162951535312, 1.000000000000000000, 0.9510565162951535312, 1.000000000000000000, 0.9510565162951535312, 1.000000000000000000, 0.9510565162951535312, 1.000000000000000000, 0.9510565162951535312, 1.000000000000000000, 0.9510565162951535312, 1.000000000000000000, 0.9510565162951535312, 1.000000000000000000, 0.9510565162951535312, 1.000000000000000000, 0.9510565162951535312, 1.000000000000000000, 0.9510565162951535312, 1.000000000000000000, 0.9510565162951535312, 1.000000000000000000, 0.9510565162951535312, 1.000000000000000000, 0.9510565162951535312, 1.000000000000000000, 0.9510565162951535312, 1.000000000000000000, 0.9510565162951535312, 1.000000000000000000, 0.9510565162951535312, 1.000000000000000000, 0.9510565162951535312, 1.000000000000000000, 0.9510565162951535312, 1.000000000000000000, 0.9510565162951535312, 1.000000000000000000, 0.9510565162951535312, 1.000000000000000000, 0.9510565162951535312, 1.000000000000000000, 0.9510565162951535312, 1.000000000000000000, 0.9510565162951535312, 1.000000000000000000, 0.9510565162951535312, 1.000000000000000000, 0.9510565162951535312, 1.000000000000000000, 0.9510565162951535312, 1.000000000000000000, 0.9510565162951535312, 1.000000000000000000, 0.9510565162951535312, 1.000000000000000000, 0.9510565162951535312, 1.000000000000000000, 0.9573764855735540369, 0.9889922301674687333 ) ) 
 REPRESENTATION_ITEM ( '' )  );
#33006 = CARTESIAN_POINT ( 'NONE',  ( -27.16883889988623935, 57.57500000273119412, 19.73931689729374739 ) ) ;
#33007 = CARTESIAN_POINT ( 'NONE',  ( -26.29305231718579350, 36.30000000546237970, -19.10302069950537884 ) ) ;
#33008 = CARTESIAN_POINT ( 'NONE',  ( 27.16883889988623935, 68.32500000273117280, -19.73931689729374384 ) ) ;
#33009 = CARTESIAN_POINT ( 'NONE',  ( 28.01184896238290278, 40.64583333333332860, -7.505752307973347470 ) ) ;
#33010 = CARTESIAN_POINT ( 'NONE',  ( 24.50000000000000355, 12.09999999999999787, -7.960532557706203605 ) ) ;
#33011 = FACE_OUTER_BOUND ( 'NONE', #27069, .T. ) ;
#33012 = CARTESIAN_POINT ( 'NONE',  ( 27.16883889988624290, 7.925000002731191984, 19.73931689729373673 ) ) ;
#33013 = DIRECTION ( 'NONE',  ( 0.000000000000000000, 1.000000000000000000, 0.000000000000000000 ) ) ;
#33014 = CARTESIAN_POINT ( 'NONE',  ( 15.04653450569339945, 53.67409749907601935, 25.98046417659831775 ) ) ;
#33015 = CARTESIAN_POINT ( 'NONE',  ( -4.635254915624208216, 72.40000000000001990, 14.26584774442730463 ) ) ;
#33016 = CARTESIAN_POINT ( 'NONE',  ( 30.02300923189239867, 54.53906249999999289, -2.619432448724978208E-13 ) ) ;
#33017 = CARTESIAN_POINT ( 'NONE',  ( -24.50000000000000000, 14.74999999453763166, -3.000384657911015469E-15 ) ) ;
#33018 = CARTESIAN_POINT ( 'NONE',  ( 5.147494310547426899, 23.44874571845314648, -32.50000000000000000 ) ) ;
#33019 = CARTESIAN_POINT ( 'NONE',  ( 15.14183272437242245, 4.049999994537630599, -20.84094480462497856 ) ) ;
#33020 = CARTESIAN_POINT ( 'NONE',  ( -9.270509831248421762, 76.55000000546237970, 12.75976212528060039 ) ) ;
#33021 = CARTESIAN_POINT ( 'NONE',  ( -26.07999730980477437, 18.30208333333332860, 6.988114217768305103 ) ) ;
#33022 = CARTESIAN_POINT ( 'NONE',  ( 20.75514604977248467, 38.42500000273118133, -28.56700777964554305 ) ) ;
#33023 = VECTOR ( 'NONE', #18093, 1000.000000000000000 ) ;
#33024 = CARTESIAN_POINT ( 'NONE',  ( 11.25946833292375793, 72.07500000273120122, -8.180482586598735395 ) ) ;
#33025 = CARTESIAN_POINT ( 'NONE',  ( -33.58253175000000113, 43.37500000273118417, 0.000000000000000000 ) ) ;
#33026 = CARTESIAN_POINT ( 'NONE',  ( 6.486482029760648627E-15, 25.87500000273117351, 35.31076352940722529 ) ) ;
#33027 = CARTESIAN_POINT ( 'NONE',  ( -15.14183272437242778, 17.04999999453762527, 20.84094480462497856 ) ) ;
#33028 = AXIS2_PLACEMENT_3D ( 'NONE', #14506, #9691, #7283 ) ;
#33029 = FACE_OUTER_BOUND ( 'NONE', #14580, .T. ) ;
#33030 = CARTESIAN_POINT ( 'NONE',  ( 20.08610463437158344, 78.69999999999998863, 27.64615127144129403 ) ) ;
#33031 = CARTESIAN_POINT ( 'NONE',  ( -20.08610463437156923, 66.30000000000001137, 27.64615127144130113 ) ) ;
#33032 = CARTESIAN_POINT ( 'NONE',  ( -7.236395654485757944, 11.22499999726880837, -22.27133577429736988 ) ) ;
#33033 = CARTESIAN_POINT ( 'NONE',  ( -7.468012846824272799, 26.60378499907601579, 28.02196122052058413 ) ) ;
#33034 = CARTESIAN_POINT ( 'NONE',  ( 1.507698388325705758E-15, 1.624999997268827823, -24.62258325217400312 ) ) ;
#33035 = CARTESIAN_POINT ( 'NONE',  ( 7.025853678916867295, 40.06732666574268364, 26.06988505166722803 ) ) ;
#33036 = ADVANCED_FACE ( 'NONE', ( #11287 ), #14198, .T. ) ;
#33037 = CARTESIAN_POINT ( 'NONE',  ( -1.778240108872766143E-15, 30.00000000546237189, -32.49999999999999289 ) ) ;
#33038 = CARTESIAN_POINT ( 'NONE',  ( 10.37757302488624767, 13.72500000273119092, 31.93888565452638417 ) ) ;
#33039 = CARTESIAN_POINT ( 'NONE',  ( 23.41746825000000243, 15.22499999726880482, -7.608796670333727974 ) ) ;
#33040 = CARTESIAN_POINT ( 'NONE',  ( 26.07999730980477437, 61.27083333333332860, -6.988114217768290004 ) ) ;
#33041 = EDGE_CURVE ( 'NONE', #19228, #14205, #4106, .T. ) ;
#33042 = ORIENTED_EDGE ( 'NONE', *, *, #6322, .F. ) ;
#33043 = CARTESIAN_POINT ( 'NONE',  ( 27.16883889988623935, 48.32500000273119412, -19.73931689729374384 ) ) ;
#33044 = CARTESIAN_POINT ( 'NONE',  ( 10.37757302488624056, 24.77500000273118275, -31.93888565452638417 ) ) ;
#33045 = VERTEX_POINT ( 'NONE', #29301 ) ;
#33046 = CARTESIAN_POINT ( 'NONE',  ( 15.01150461594643204, 31.04947916666666075, 26.00068869287340334 ) ) ;
#33047 = CARTESIAN_POINT ( 'NONE',  ( -7.468012846824771955, 30.91184000092396644, -28.02196122052045624 ) ) ;
#33048 = CARTESIAN_POINT ( 'NONE',  ( -26.29305231718578995, 72.70000000546239960, 19.10302069950538595 ) ) ;
#33049 = CARTESIAN_POINT ( 'NONE',  ( -24.50000000000000000, 18.74999999453763522, -3.000384657911015469E-15 ) ) ;
#33050 = AXIS2_PLACEMENT_3D ( 'NONE', #21129, #31069, #12885 ) ;
#33051 = EDGE_CURVE ( 'NONE', #4618, #22505, #1636, .T. ) ;
#33052 = CARTESIAN_POINT ( 'NONE',  ( -23.41746825000000243, 13.52499999726880198, -7.608796670333730638 ) ) ;
#33053 = CARTESIAN_POINT ( 'NONE',  ( 33.58253175000000113, 24.37500000273118417, -4.112674001490185761E-15 ) ) ;
#33054 = CARTESIAN_POINT ( 'NONE',  ( 26.29305231718579350, 27.30000000546237260, 19.10302069950537529 ) ) ;
#33055 = CARTESIAN_POINT ( 'NONE',  ( 32.50000000000000000, 67.00000000000000000, -3.980102097228898626E-15 ) ) ;
#33056 = CARTESIAN_POINT ( 'NONE',  ( 20.08610463437158344, 47.20000000546237828, 27.64615127144129403 ) ) ;
#33057 = CARTESIAN_POINT ( 'NONE',  ( -3.054597574617877509, 74.00000000000002842, 13.92607879720974218 ) ) ;
#33058 = CARTESIAN_POINT ( 'NONE',  ( -30.02300923189239512, 15.00781249999999467, 2.654126918244515359E-13 ) ) ;
#33059 = CARTESIAN_POINT ( 'NONE',  ( 33.58253175000000113, 38.47500000273118559, -10.91162601494193751 ) ) ;
#33060 = CARTESIAN_POINT ( 'NONE',  ( 5.779280353836490358E-15, 43.00000000546236834, 32.49999999999999289 ) ) ;
#33061 = CARTESIAN_POINT ( 'NONE',  ( 20.50609665441005092, 27.46875000000000000, 20.50609665440969209 ) ) ;
#33062 = SHAPE_REPRESENTATION_RELATIONSHIP ( 'NONE' , 'NONE' ,  #10290, #18129 ) ;
#33063 = CARTESIAN_POINT ( 'NONE',  ( -1.467220197368425466E-15, 122.0000000000000000, -10.64101615137753676 ) ) ;
#33064 = CARTESIAN_POINT ( 'NONE',  ( -10.04305231718578462, 16.39999999999999858, 30.90933677959249337 ) ) ;
#33065 = CARTESIAN_POINT ( 'NONE',  ( 24.50000000000000000, 15.99999999999998579, 0.000000000000000000 ) ) ;
#33066 = CARTESIAN_POINT ( 'NONE',  ( 26.06988505166722803, 39.20795166574269075, -7.025853678916862854 ) ) ;
#33067 = CARTESIAN_POINT ( 'NONE',  ( -20.75514604977248112, 59.42500000273118843, 28.56700777964554661 ) ) ;
#33068 = CARTESIAN_POINT ( 'NONE',  ( -33.58253175000000113, 59.47500000273118559, 10.91162601494193929 ) ) ;
#33069 = CARTESIAN_POINT ( 'NONE',  ( 10.37757302488624767, 45.97500000273119269, 31.93888565452638417 ) ) ;
#33070 = CARTESIAN_POINT ( 'NONE',  ( -1.778240108872766143E-15, 45.49999999999999289, -32.49999999999999289 ) ) ;
#33071 = LINE ( 'NONE', #11813, #20526 ) ;
#33072 = CARTESIAN_POINT ( 'NONE',  ( -20.08610463437156923, 50.30000000000001137, 27.64615127144130113 ) ) ;
#33073 = CARTESIAN_POINT ( 'NONE',  ( -19.06425588902591173, 44.37538166759063785, -19.11951029504763611 ) ) ;
#33074 = CARTESIAN_POINT ( 'NONE',  ( -3.880418787951142701, 5.198745712990781698, 24.49999999999999645 ) ) ;
#33075 = CARTESIAN_POINT ( 'NONE',  ( -1.778240108872766143E-15, 71.50000000000001421, -32.49999999999999289 ) ) ;
#33076 = CARTESIAN_POINT ( 'NONE',  ( -10.37757302488623701, 23.52500000273117919, 31.93888565452638417 ) ) ;
#33077 = CARTESIAN_POINT ( 'NONE',  ( 32.50000000000000000, 67.00000000000000000, -3.980102097228898626E-15 ) ) ;
#33078 = CARTESIAN_POINT ( 'NONE',  ( -19.79898987322349768, 11.99999999999999645, -19.79898987322315307 ) ) ;
#33079 = AXIS2_PLACEMENT_3D ( 'NONE', #15177, #22894, #32992 ) ;
#33080 = VECTOR ( 'NONE', #2453, 1000.000000000000114 ) ;
#33081 = DIRECTION ( 'NONE',  ( -0.000000000000000000, -1.000000000000000000, -0.000000000000000000 ) ) ;
#33082 = CARTESIAN_POINT ( 'NONE',  ( -28.02196122052058413, 61.83815999907601935, -7.468012846824272799 ) ) ;
#33083 = CARTESIAN_POINT ( 'NONE',  ( -2.092463501923844636E-15, 42.00000000546236834, -34.17252228774368916 ) ) ;
#33084 = CARTESIAN_POINT ( 'NONE',  ( 1.093617666956751375E-13, 60.00000000546237544, -32.50000000000000711 ) ) ;
#33085 = CARTESIAN_POINT ( 'NONE',  ( -20.75514604977248112, 33.42500000273120264, 28.56700777964554661 ) ) ;
#33086 = CARTESIAN_POINT ( 'NONE',  ( -20.75514604977248112, 65.67500000273116711, 28.56700777964554661 ) ) ;
#33087 = CARTESIAN_POINT ( 'NONE',  ( -19.09188309203694445, 36.06250000000000000, -19.09188309203661049 ) ) ;
#33088 = ORIENTED_EDGE ( 'NONE', *, *, #21276, .T. ) ;
#33089 = CARTESIAN_POINT ( 'NONE',  ( -33.58253175000000113, 71.22500000273117848, 10.91162601494193929 ) ) ;
#33090 = CARTESIAN_POINT ( 'NONE',  ( -20.50609665440969209, 38.64062500000000000, 20.50609665441005092 ) ) ;
#33091 = CARTESIAN_POINT ( 'NONE',  ( 24.50000000000000000, -29.78157438140398128, 3.000384657911015469E-15 ) ) ;
#33092 = EDGE_LOOP ( 'NONE', ( #19727, #13632, #21167, #30049, #24460, #32379, #7018, #32338, #4272, #4787, #25208, #22057, #22680, #16703, #32132, #7314, #30387, #22900, #25105, #4528, #28974, #26988, #15099, #14123, #22730, #30568, #4149, #24998, #9286, #28803, #32126, #4698, #33957, #6766, #5041, #29934, #4783, #3940, #30389, #6557, #14289, #33919, #33113, #5468, #31296, #8793, #4, #32837, #2857, #8789, #28588, #26408, #11191, #3073, #3113, #9288, #14605, #17223, #21866, #6238, #4739, #20373, #28424, #23286, #27133, #8962, #24558, #9509, #30863, #2854, #3023, #18857, #5761, #32169, #13451, #28870, #6347, #8708, #15909, #24003, #31212, #5477 ) ) ;
#33093 = CARTESIAN_POINT ( 'NONE',  ( -30.02300923189239867, 57.69569416759065206, -0.04044903254991731589 ) ) ;
#33094 = CARTESIAN_POINT ( 'NONE',  ( 14.01125832528286352, 62.27902750092396644, -24.18731323226246843 ) ) ;
#33095 = CARTESIAN_POINT ( 'NONE',  ( 33.58253175000000113, 10.22500000273118914, -10.91162601494193751 ) ) ;
#33096 = CARTESIAN_POINT ( 'NONE',  ( -15.04653450569338524, 17.58034749907602290, -25.98046417659831775 ) ) ;
#33097 = CARTESIAN_POINT ( 'NONE',  ( 5.779280353836490358E-15, 43.00000000546236834, 32.49999999999999289 ) ) ;
#33098 = CARTESIAN_POINT ( 'NONE',  ( 10.37757302488624056, 42.77500000273118275, -31.93888565452638417 ) ) ;
#33099 = CARTESIAN_POINT ( 'NONE',  ( -10.04305231718579172, 44.10000000546238397, -30.90933677959248982 ) ) ;
#33100 = CARTESIAN_POINT ( 'NONE',  ( 11.25946833292375793, 72.17500000273119554, 8.180482586598731842 ) ) ;
#33101 = CARTESIAN_POINT ( 'NONE',  ( 33.58253175000000823, 32.02500000273118275, 10.91162601494192863 ) ) ;
#33102 = CARTESIAN_POINT ( 'NONE',  ( 20.75514604977248467, 52.67500000273116711, -28.56700777964554305 ) ) ;
#33103 = CARTESIAN_POINT ( 'NONE',  ( 6.277390505771533514E-15, 36.49999999999997868, 34.17252228774368916 ) ) ;
#33104 = CARTESIAN_POINT ( 'NONE',  ( -32.50000000000000000, 32.00000000000000000, 0.000000000000000000 ) ) ;
#33105 = CARTESIAN_POINT ( 'NONE',  ( -23.41746825000000598, 15.72499999726882081, 7.608796670333726198 ) ) ;
#33106 = ADVANCED_FACE ( 'NONE', ( #6797 ), #6967, .T. ) ;
#33107 =( BOUNDED_CURVE ( )  B_SPLINE_CURVE ( 2, ( #10785, #8199, #124, #10279, #23833, #21262, #18352, #298, #31030, #31707, #18690, #23492, #18520 ),
 .UNSPECIFIED., .F., .T. ) 
 B_SPLINE_CURVE_WITH_KNOTS ( ( 3, 2, 2, 2, 2, 2, 3 ),
 ( 0.5064102564102563875, 0.5076923076923076650, 0.5102564102564102200, 0.5128205128205127750, 0.5153846153846153300, 0.5179487179487179960, 0.5192307692307692735 ),
 .UNSPECIFIED. ) 
 CURVE ( )  GEOMETRIC_REPRESENTATION_ITEM ( )  RATIONAL_B_SPLINE_CURVE ( ( 0.9755282581475768211, 0.9755282581475768211, 1.000000000000000000, 0.9510565162951535312, 1.000000000000000000, 0.9510565162951535312, 1.000000000000000000, 0.9510565162951535312, 1.000000000000000000, 0.9510565162951535312, 1.000000000000000000, 0.9755282581475768211, 0.9755282581475768211 ) ) 
 REPRESENTATION_ITEM ( '' )  );
#33108 = CARTESIAN_POINT ( 'NONE',  ( 20.75514604977249178, 77.82500000273120122, 28.56700777964553950 ) ) ;
#33109 = CARTESIAN_POINT ( 'NONE',  ( 32.50000000000000000, 62.99999999999998579, -3.980102097228898626E-15 ) ) ;
#33110 = CARTESIAN_POINT ( 'NONE',  ( 11.25946833292375793, 74.57500000273120122, -8.180482586598735395 ) ) ;
#33111 = CARTESIAN_POINT ( 'NONE',  ( 33.58253175000000823, 68.27500000273120406, 10.91162601494192685 ) ) ;
#33112 = CARTESIAN_POINT ( 'NONE',  ( 15.00000000000000355, 79.15000000546235981, 4.873795443493592394 ) ) ;
#33113 = ORIENTED_EDGE ( 'NONE', *, *, #33267, .T. ) ;
#33114 = CARTESIAN_POINT ( 'NONE',  ( -2.162160676586881955E-15, 16.62500000273120548, -35.31076352940723240 ) ) ;
#33115 = CARTESIAN_POINT ( 'NONE',  ( -7.570916362186210335, 10.34999999453761710, -23.30088464923126779 ) ) ;
#33116 = CARTESIAN_POINT ( 'NONE',  ( 0.04044903254993986036, 20.74256916759064495, -27.95245687107223986 ) ) ;
#33117 = CARTESIAN_POINT ( 'NONE',  ( -12.13525491562421088, 74.05000000546240813, -8.816778784387096835 ) ) ;
#33118 = CARTESIAN_POINT ( 'NONE',  ( 27.16883889988624290, 39.92500000273118133, 19.73931689729373673 ) ) ;
#33119 = CARTESIAN_POINT ( 'NONE',  ( -20.75514604977248112, 1.675000002731184434, 28.56700777964554661 ) ) ;
#33120 = CARTESIAN_POINT ( 'NONE',  ( 33.58253175000000823, 58.27500000273116854, 10.91162601494192685 ) ) ;
#33121 = CARTESIAN_POINT ( 'NONE',  ( -14.97647472619946285, 44.51861083425730214, -26.02091320914851025 ) ) ;
#33122 = CARTESIAN_POINT ( 'NONE',  ( -20.47846945139866648, 40.64024333240936215, 20.53372385742108008 ) ) ;
#33123 = CARTESIAN_POINT ( 'NONE',  ( -20.08610463437157989, 58.20000000546238539, -27.64615127144129758 ) ) ;
#33124 = CARTESIAN_POINT ( 'NONE',  ( 4.300734207923761154, 75.47500000273116427, 13.23629886949340495 ) ) ;
#33125 = CARTESIAN_POINT ( 'NONE',  ( 0.04044903255044120238, 60.83555583240935505, 27.95245687107223276 ) ) ;
#33126 = DIRECTION ( 'NONE',  ( 0.000000000000000000, 0.000000000000000000, 1.000000000000000000 ) ) ;
#33127 = CARTESIAN_POINT ( 'NONE',  ( -10.04305231718579172, 78.10000000546237686, -30.90933677959248982 ) ) ;
#33128 = CARTESIAN_POINT ( 'NONE',  ( 26.00068869287367335, 17.01302083333332504, 15.01150461594596308 ) ) ;
#33129 = CARTESIAN_POINT ( 'NONE',  ( -27.16883889988623935, 41.57500000273119412, 19.73931689729374739 ) ) ;
#33130 = CARTESIAN_POINT ( 'NONE',  ( 18.94512977948576093, 9.324999997268824004, -13.76444248337722875 ) ) ;
#33131 = VERTEX_POINT ( 'NONE', #7136 ) ;
#33132 = CARTESIAN_POINT ( 'NONE',  ( 6.486482029760649416E-15, 71.87500000273116996, 35.31076352940723240 ) ) ;
#33133 = MANIFOLD_SOLID_BREP ( 'Revolve-Thin1', #210 ) ;
#33134 = CARTESIAN_POINT ( 'NONE',  ( 26.29305231718578995, 27.70000000546236762, -19.10302069950538240 ) ) ;
#33135 = ORIENTED_EDGE ( 'NONE', *, *, #9342, .F. ) ;
#33136 = CARTESIAN_POINT ( 'NONE',  ( -30.02300923189239512, 32.19531250000000000, 2.654126918244515359E-13 ) ) ;
#33137 = CARTESIAN_POINT ( 'NONE',  ( 26.29305231718579350, 65.30000000546237970, 19.10302069950537529 ) ) ;
#33138 = VERTEX_POINT ( 'NONE', #33037 ) ;
#33139 = CARTESIAN_POINT ( 'NONE',  ( -10.04305231718578462, 74.90000000546237402, 30.90933677959249337 ) ) ;
#33140 = CARTESIAN_POINT ( 'NONE',  ( 6.486482029760649416E-15, 45.62500000273118417, 35.31076352940723240 ) ) ;
#33141 = CARTESIAN_POINT ( 'NONE',  ( 2.205017735002230837E-13, 56.00000000546238255, -32.50000000000000000 ) ) ;
#33142 = CARTESIAN_POINT ( 'NONE',  ( -26.29305231718579350, 6.300000005462380592, -19.10302069950537884 ) ) ;
#33143 = CARTESIAN_POINT ( 'NONE',  ( -20.75514604977248823, 66.82500000273118701, -28.56700777964554305 ) ) ;
#33144 = CARTESIAN_POINT ( 'NONE',  ( 14.47279130897151767, 18.82499999726880802, 19.92008829642072953 ) ) ;
#33145 = PRESENTATION_LAYER_ASSIGNMENT (  '', '', ( #5249 ) ) ;
#33146 = CARTESIAN_POINT ( 'NONE',  ( 26.29305231718578995, 53.19999999999999574, -19.10302069950538240 ) ) ;
#33147 = ADVANCED_FACE ( 'NONE', ( #33390 ), #30296, .T. ) ;
#33148 = CARTESIAN_POINT ( 'NONE',  ( 5.779280353836490358E-15, 14.50000000000000178, 32.49999999999999289 ) ) ;
#33149 = CARTESIAN_POINT ( 'NONE',  ( -2.162160676586881955E-15, 18.87500000273119483, -35.31076352940723240 ) ) ;
#33150 = DIRECTION ( 'NONE',  ( 0.000000000000000000, -1.000000000000000000, 0.000000000000000000 ) ) ;
#33151 = CARTESIAN_POINT ( 'NONE',  ( 13.94119854578893580, 25.02826416574268720, -24.22776226481265383 ) ) ;
#33152 = CARTESIAN_POINT ( 'NONE',  ( -13.91746824999999532, 74.77500000273117564, -4.522059556121115875 ) ) ;
#33153 = CYLINDRICAL_SURFACE ( 'NONE', #24984, 32.50000000000000000 ) ;
#33154 = CARTESIAN_POINT ( 'NONE',  ( 12.90513655866702081, 52.00000000000000711, 31.00393344628893288 ) ) ;
#33155 = ADVANCED_FACE ( 'NONE', ( #9196 ), #10689, .T. ) ;
#33156 = CARTESIAN_POINT ( 'NONE',  ( 20.08610463437158344, 6.699999999999991296, 27.64615127144129403 ) ) ;
#33157 = ORIENTED_EDGE ( 'NONE', *, *, #5600, .T. ) ;
#33158 = CARTESIAN_POINT ( 'NONE',  ( 14.47279130897151767, 15.42499999726879878, -19.92008829642072598 ) ) ;
#33159 = DIRECTION ( 'NONE',  ( -1.000000000000000000, 0.000000000000000000, 0.000000000000000000 ) ) ;
#33160 = CARTESIAN_POINT ( 'NONE',  ( -26.07999730980490583, 52.96354166666666430, -6.988114217767815717 ) ) ;
#33161 = CARTESIAN_POINT ( 'NONE',  ( 10.37757302488624767, 61.72500000273119269, 31.93888565452638417 ) ) ;
#33162 = CARTESIAN_POINT ( 'NONE',  ( 20.75514604977248467, 24.67500000273118843, -28.56700777964554305 ) ) ;
#33163 = CARTESIAN_POINT ( 'NONE',  ( -27.16883889988624290, 9.175000002731179549, -19.73931689729374028 ) ) ;
#33164 = CARTESIAN_POINT ( 'NONE',  ( 33.58253175000000113, 2.375000002731192161, -4.112674001490185761E-15 ) ) ;
#33165 = CARTESIAN_POINT ( 'NONE',  ( -7.468012846824771955, 20.59934000092397355, -28.02196122052045624 ) ) ;
#33166 = CARTESIAN_POINT ( 'NONE',  ( -7.505752307972844761, 62.41666666666666430, 28.01184896238304134 ) ) ;
#33167 = CARTESIAN_POINT ( 'NONE',  ( 26.29305231718578995, 77.70000000546238539, -19.10302069950538240 ) ) ;
#33168 = CARTESIAN_POINT ( 'NONE',  ( -13.91746824999999532, 73.47500000273119269, 4.522059556121122093 ) ) ;
#33169 = CARTESIAN_POINT ( 'NONE',  ( -32.50000000000000000, 39.99999999999999289, 0.000000000000000000 ) ) ;
#33170 = CARTESIAN_POINT ( 'NONE',  ( -27.16883889988623935, 43.32500000273120833, 19.73931689729374739 ) ) ;
#33171 = CARTESIAN_POINT ( 'NONE',  ( -18.94512977948576093, 18.32499999726880446, 13.76444248337722698 ) ) ;
#33172 = CARTESIAN_POINT ( 'NONE',  ( 26.29305231718579350, 21.30000000546239391, 19.10302069950537529 ) ) ;
#33173 =( GEOMETRIC_REPRESENTATION_CONTEXT ( 3 ) GLOBAL_UNCERTAINTY_ASSIGNED_CONTEXT ( ( #5032 ) ) GLOBAL_UNIT_ASSIGNED_CONTEXT ( ( #17682, #2220, #15109 ) ) REPRESENTATION_CONTEXT ( 'NONE', 'WORKASPACE' ) );
#33174 = VERTEX_POINT ( 'NONE', #8878 ) ;
#33175 = CARTESIAN_POINT ( 'NONE',  ( -20.75514604977248823, 63.07500000273119412, -28.56700777964554305 ) ) ;
#33176 = FACE_OUTER_BOUND ( 'NONE', #19436, .T. ) ;
#33177 = CARTESIAN_POINT ( 'NONE',  ( 7.236395654485760609, 13.02499999726880375, -22.27133577429736633 ) ) ;
#33178 = CARTESIAN_POINT ( 'NONE',  ( -14.01125832528285109, 29.62277750092397355, 24.18731323226248264 ) ) ;
#33179 = ORIENTED_EDGE ( 'NONE', *, *, #8518, .F. ) ;
#33180 = CARTESIAN_POINT ( 'NONE',  ( -27.16883889988624290, 30.92500000273119909, -19.73931689729374028 ) ) ;
#33181 = CARTESIAN_POINT ( 'NONE',  ( -20.08610463437156923, 34.80000000546238681, 27.64615127144130113 ) ) ;
#33182 = ORIENTED_EDGE ( 'NONE', *, *, #29912, .F. ) ;
#33183 = AXIS2_PLACEMENT_3D ( 'NONE', #17179, #19246, #29522 ) ;
#33184 = PLANE ( 'NONE',  #3437 ) ;
#33185 = CARTESIAN_POINT ( 'NONE',  ( 33.58253175000000113, 66.22500000273120691, -10.91162601494193751 ) ) ;
#33186 = CARTESIAN_POINT ( 'NONE',  ( -7.505752307973343918, 43.22395833333332860, -28.01184896238290989 ) ) ;
#33187 = CARTESIAN_POINT ( 'NONE',  ( 24.50000000000000355, 13.89999999999999858, 7.960532557706212486 ) ) ;
#33188 = CARTESIAN_POINT ( 'NONE',  ( -7.236395654485757944, 1.724999997268800156, -22.27133577429736988 ) ) ;
#33189 = CARTESIAN_POINT ( 'NONE',  ( 10.37757302488624767, 9.725000002731187365, 31.93888565452638417 ) ) ;
#33190 = CARTESIAN_POINT ( 'NONE',  ( 10.04305231718578817, 29.40000000000000924, -30.90933677959249337 ) ) ;
#33191 = CARTESIAN_POINT ( 'NONE',  ( -30.02300923189239867, 54.81993083240935505, 0.04044903255044988294 ) ) ;
#33192 = CARTESIAN_POINT ( 'NONE',  ( 26.29305231718579350, 36.79999999999999716, 19.10302069950537529 ) ) ;
#33193 = CARTESIAN_POINT ( 'NONE',  ( 7.505752307973351023, 58.69270833333332860, 28.01184896238290278 ) ) ;
#33194 = CARTESIAN_POINT ( 'NONE',  ( 0.000000000000000000, 80.00000000000001421, 0.000000000000000000 ) ) ;
#33195 = CARTESIAN_POINT ( 'NONE',  ( 2.445080149700053643E-15, 74.75000000546236834, 15.00000000000000000 ) ) ;
#33196 = CARTESIAN_POINT ( 'NONE',  ( 7.570916362186213000, 6.149999994537635573, -23.30088464923126423 ) ) ;
#33197 = CARTESIAN_POINT ( 'NONE',  ( -12.13525491562420910, 74.45000000546237118, 8.816778784387098611 ) ) ;
#33198 = CARTESIAN_POINT ( 'NONE',  ( 13.97622843553633665, 27.61197916666666430, 24.20753774853730889 ) ) ;
#33199 = CARTESIAN_POINT ( 'NONE',  ( 20.75514604977249178, 39.82500000273116569, 28.56700777964553950 ) ) ;
#33200 = CARTESIAN_POINT ( 'NONE',  ( -27.16883889988623935, 77.32500000273120122, 19.73931689729374739 ) ) ;
#33201 = CARTESIAN_POINT ( 'NONE',  ( -27.16883889988623935, 43.57500000273119412, 19.73931689729374739 ) ) ;
#33202 = CARTESIAN_POINT ( 'NONE',  ( -20.75514604977248823, 19.07500000273118701, -28.56700777964554305 ) ) ;
#33203 = CARTESIAN_POINT ( 'NONE',  ( -8.761981113183991350E-16, -15.84529946162075298, 0.000000000000000000 ) ) ;
#33204 = CARTESIAN_POINT ( 'NONE',  ( 24.50000000000000000, 1.899999999999998135, 7.960532557706212486 ) ) ;
#33205 = CARTESIAN_POINT ( 'NONE',  ( 5.779280353836490358E-15, 13.00000000546238077, 32.49999999999999289 ) ) ;
#33206 = CARTESIAN_POINT ( 'NONE',  ( 6.277390505771533514E-15, 60.49999999999997868, 34.17252228774368916 ) ) ;
#33207 = CARTESIAN_POINT ( 'NONE',  ( 23.41746824999999887, 12.62499999726882116, 0.000000000000000000 ) ) ;
#33208 = CARTESIAN_POINT ( 'NONE',  ( -20.75514604977248112, 61.42500000273118133, 28.56700777964554661 ) ) ;
#33209 =( BOUNDED_CURVE ( )  B_SPLINE_CURVE ( 2, ( #19153, #773, #599, #11254, #8834, #8670, #29095, #29759, #3030, #8332, #29592, #16575, #27030 ),
 .UNSPECIFIED., .F., .T. ) 
 B_SPLINE_CURVE_WITH_KNOTS ( ( 3, 2, 2, 2, 2, 2, 3 ),
 ( 0.1217948717948718063, 0.1230769230769230838, 0.1256410256410256387, 0.1282051282051281937, 0.1307692307692307765, 0.1333333333333333315, 0.1346153846153846090 ),
 .UNSPECIFIED. ) 
 CURVE ( )  GEOMETRIC_REPRESENTATION_ITEM ( )  RATIONAL_B_SPLINE_CURVE ( ( 0.9755282581475767101, 0.9755282581475768211, 1.000000000000000000, 0.9510565162951535312, 1.000000000000000000, 0.9510565162951535312, 1.000000000000000000, 0.9510565162951535312, 1.000000000000000000, 0.9510565162951535312, 1.000000000000000000, 0.9755282581475768211, 0.9755282581475768211 ) ) 
 REPRESENTATION_ITEM ( '' )  );
#33210 = CARTESIAN_POINT ( 'NONE',  ( 14.47279130897151767, 5.424999997268823648, -19.92008829642072598 ) ) ;
#33211 = CARTESIAN_POINT ( 'NONE',  ( 26.09010956794244507, 36.05690999907600514, 6.950374756619249084 ) ) ;
#33212 = EDGE_CURVE ( 'NONE', #1686, #3077, #16212, .T. ) ;
#33213 =( LENGTH_UNIT ( ) NAMED_UNIT ( * ) SI_UNIT ( .MILLI., .METRE. ) );
#33214 =( BOUNDED_CURVE ( )  B_SPLINE_CURVE ( 2, ( #4557, #15036, #15207, #7298, #25671, #9353, #30117, #30288, #28411, #25838, #28576, #10396, #10233 ),
 .UNSPECIFIED., .F., .F. ) 
 B_SPLINE_CURVE_WITH_KNOTS ( ( 3, 2, 2, 2, 2, 2, 3 ),
 ( 0.1474358974358974395, 0.1487179487179487170, 0.1512820512820512719, 0.1538461538461538547, 0.1564102564102564097, 0.1589743589743589647, 0.1602564102564102699 ),
 .UNSPECIFIED. ) 
 CURVE ( )  GEOMETRIC_REPRESENTATION_ITEM ( )  RATIONAL_B_SPLINE_CURVE ( ( 0.9755282581475768211, 0.9755282581475768211, 1.000000000000000000, 0.9510565162951535312, 1.000000000000000000, 0.9510565162951535312, 1.000000000000000000, 0.9510565162951535312, 1.000000000000000000, 0.9510565162951535312, 1.000000000000000000, 0.9755282581475764880, 0.9755282581475768211 ) ) 
 REPRESENTATION_ITEM ( '' )  );
#33215 = CARTESIAN_POINT ( 'NONE',  ( -27.16883889988624290, 10.92500000273119376, -19.73931689729374028 ) ) ;
#33216 = CARTESIAN_POINT ( 'NONE',  ( 23.41746824999999887, 11.12499999726881938, 0.000000000000000000 ) ) ;
#33217 = CARTESIAN_POINT ( 'NONE',  ( -19.09188309203694445, 60.12500000000000000, -19.09188309203661049 ) ) ;
#33218 = ORIENTED_EDGE ( 'NONE', *, *, #20072, .F. ) ;
#33219 = CARTESIAN_POINT ( 'NONE',  ( 10.37757302488624056, 48.52500000273117564, -31.93888565452638417 ) ) ;
#33220 = CARTESIAN_POINT ( 'NONE',  ( 27.16883889988623935, 24.57500000273120477, -19.73931689729374384 ) ) ;
#33221 = ORIENTED_EDGE ( 'NONE', *, *, #9334, .T. ) ;
#33222 = CARTESIAN_POINT ( 'NONE',  ( -7.505752307973343918, 29.47395833333332860, -28.01184896238290989 ) ) ;
#33223 = CARTESIAN_POINT ( 'NONE',  ( -28.00173670424549499, 33.77642333425730214, -7.543491769121417612 ) ) ;
#33224 = CYLINDRICAL_SURFACE ( 'NONE', #7299, 32.50000000000000000 ) ;
#33225 = CARTESIAN_POINT ( 'NONE',  ( -10.04305231718579172, 72.10000000546237686, -30.90933677959248982 ) ) ;
#33226 = CARTESIAN_POINT ( 'NONE',  ( -18.94512977948575738, 5.924999997268809437, -13.76444248337723231 ) ) ;
#33227 = CARTESIAN_POINT ( 'NONE',  ( 7.236395654485760609, 9.024999997268800200, -22.27133577429736633 ) ) ;
#33228 = CARTESIAN_POINT ( 'NONE',  ( 20.75514604977249178, 22.07500000273117990, 28.56700777964553950 ) ) ;
#33229 = CARTESIAN_POINT ( 'NONE',  ( -10.04305231718579172, 22.10000000546236265, -30.90933677959248982 ) ) ;
#33230 = CARTESIAN_POINT ( 'NONE',  ( -26.29305231718578995, 64.20000000000000284, 19.10302069950538595 ) ) ;
#33231 = CARTESIAN_POINT ( 'NONE',  ( -24.50000000000000000, 5.000000000000004441, -3.000384657911015469E-15 ) ) ;
#33232 = CARTESIAN_POINT ( 'NONE',  ( -12.49601229055796914, 74.00000000000005684, 7.815062094324783715 ) ) ;
#33233 = CARTESIAN_POINT ( 'NONE',  ( -14.97647472619946285, 61.70611083425731636, -26.02091320914851025 ) ) ;
#33234 = CARTESIAN_POINT ( 'NONE',  ( -10.37757302488623701, 35.77500000273120406, 31.93888565452638417 ) ) ;
#33235 = CARTESIAN_POINT ( 'NONE',  ( -20.08610463437156923, 32.80000000546237260, 27.64615127144130113 ) ) ;
#33236 = CARTESIAN_POINT ( 'NONE',  ( -2.584737979205442066E-13, 33.05468750000000000, -30.02300923189239867 ) ) ;
#33237 = DIRECTION ( 'NONE',  ( 1.000000000000000000, 0.000000000000000000, 0.000000000000000000 ) ) ;
#33238 = AXIS2_PLACEMENT_3D ( 'NONE', #21246, #25868, #13003 ) ;
#33239 = CARTESIAN_POINT ( 'NONE',  ( -14.47279130897151589, 13.82499999726882045, -19.92008829642072598 ) ) ;
#33240 = CARTESIAN_POINT ( 'NONE',  ( 32.50000000000000000, 11.00000000000001066, -3.980102097228898626E-15 ) ) ;
#33241 = CARTESIAN_POINT ( 'NONE',  ( 10.04305231718579705, 9.100000005462376862, 30.90933677959248982 ) ) ;
#33242 = CARTESIAN_POINT ( 'NONE',  ( -7.025853678916861966, 55.53607666574269075, -26.06988505166722803 ) ) ;
#33243 = CARTESIAN_POINT ( 'NONE',  ( 10.37757302488624767, 57.72500000273117848, 31.93888565452638417 ) ) ;
#33244 = CARTESIAN_POINT ( 'NONE',  ( -10.37757302488624411, 58.97500000273119269, -31.93888565452638417 ) ) ;
#33245 = CARTESIAN_POINT ( 'NONE',  ( 27.16883889988624290, 44.17500000273119554, 19.73931689729373673 ) ) ;
#33246 = CARTESIAN_POINT ( 'NONE',  ( 18.94512977948575738, 16.42499999726882010, 13.76444248337723408 ) ) ;
#33247 = EDGE_CURVE ( 'NONE', #20845, #17411, #8547, .T. ) ;
#33248 = CIRCLE ( 'NONE', #17364, 15.31593959127081384 ) ;
#33249 = LINE ( 'NONE', #9745, #9521 ) ;
#33250 = LINE ( 'NONE', #25367, #32751 ) ;
#33251 = CARTESIAN_POINT ( 'NONE',  ( -0.04044903254992426173, 46.52381916759065206, 27.95245687107223276 ) ) ;
#33252 = CARTESIAN_POINT ( 'NONE',  ( -19.35449145663587700, 16.99999999999998934, -14.56863439756531342 ) ) ;
#33253 = FACE_OUTER_BOUND ( 'NONE', #23968, .T. ) ;
#33254 = CARTESIAN_POINT ( 'NONE',  ( -2.162160676586881955E-15, 24.62500000273118772, -35.31076352940723240 ) ) ;
#33255 = CARTESIAN_POINT ( 'NONE',  ( 20.08610463437157279, 67.29999999999998295, -27.64615127144129758 ) ) ;
#33256 = FACE_OUTER_BOUND ( 'NONE', #2562, .T. ) ;
#33257 = EDGE_CURVE ( 'NONE', #927, #25651, #33738, .T. ) ;
#33258 = CARTESIAN_POINT ( 'NONE',  ( -11.54700538379251995, 86.00000000000001421, -19.99999999999999645 ) ) ;
#33259 = EDGE_CURVE ( 'NONE', #27857, #31472, #9047, .T. ) ;
#33260 = CARTESIAN_POINT ( 'NONE',  ( -7.543491769121917656, 62.41107666574269075, -28.00173670424536354 ) ) ;
#33261 = CARTESIAN_POINT ( 'NONE',  ( -26.29305231718579350, 42.30000000546237260, -19.10302069950537884 ) ) ;
#33262 = CARTESIAN_POINT ( 'NONE',  ( -20.08610463437156923, 60.80000000546238681, 27.64615127144130113 ) ) ;
#33263 = CARTESIAN_POINT ( 'NONE',  ( 33.58253175000000113, 30.12500000273118772, -4.112674001490185761E-15 ) ) ;
#33264 = CARTESIAN_POINT ( 'NONE',  ( 10.37757302488624056, 64.77500000273117564, -31.93888565452638417 ) ) ;
#33265 = CARTESIAN_POINT ( 'NONE',  ( 13.97622843553633665, 31.04947916666666075, 24.20753774853730889 ) ) ;
#33266 = ORIENTED_EDGE ( 'NONE', *, *, #2764, .T. ) ;
#33267 = EDGE_CURVE ( 'NONE', #30543, #29467, #28220, .T. ) ;
#33268 = CARTESIAN_POINT ( 'NONE',  ( -33.58253175000000113, 69.12500000273118417, 0.000000000000000000 ) ) ;
#33269 = CARTESIAN_POINT ( 'NONE',  ( 20.50609665440969565, 40.35937499999999289, -20.50609665441004736 ) ) ;
#33270 = CYLINDRICAL_SURFACE ( 'NONE', #5556, 24.50000000000000000 ) ;
#33271 = ORIENTED_EDGE ( 'NONE', *, *, #24474, .T. ) ;
#33272 = CARTESIAN_POINT ( 'NONE',  ( 30.02300923189239867, 59.41444416759064495, 0.04044903254992252006 ) ) ;
#33273 = CARTESIAN_POINT ( 'NONE',  ( -24.22776226481240514, 57.40923583425731636, 13.94119854578937812 ) ) ;
#33274 = CARTESIAN_POINT ( 'NONE',  ( -33.58253175000000113, 13.02500000273118985, -10.91162601494193218 ) ) ;
#33275 = CARTESIAN_POINT ( 'NONE',  ( 7.543491769121922985, 16.00482666574268720, 28.00173670424535644 ) ) ;
#33276 = FACE_BOUND ( 'NONE', #7867, .T. ) ;
#33277 = CARTESIAN_POINT ( 'NONE',  ( 27.16883889988624290, 38.17500000273118843, 19.73931689729373673 ) ) ;
#33278 = CARTESIAN_POINT ( 'NONE',  ( 26.29305231718578995, 43.70000000546237118, -19.10302069950538240 ) ) ;
#33279 = CARTESIAN_POINT ( 'NONE',  ( 12.13525491562421088, 78.80000000000003979, 8.816778784387095058 ) ) ;
#33280 = CARTESIAN_POINT ( 'NONE',  ( 10.37757302488624767, 31.72500000273117848, 31.93888565452638417 ) ) ;
#33281 = CARTESIAN_POINT ( 'NONE',  ( 24.50000000000000000, 13.74999999453763166, 0.000000000000000000 ) ) ;
#33282 = CARTESIAN_POINT ( 'NONE',  ( -2.162160676586881955E-15, 52.87500000273119838, -35.31076352940723240 ) ) ;
#33283 =( NAMED_UNIT ( * ) PLANE_ANGLE_UNIT ( ) SI_UNIT ( $, .RADIAN. ) );
#33284 = CARTESIAN_POINT ( 'NONE',  ( -32.50000000000000000, 32.10000000000000142, 10.55989012756946366 ) ) ;
#33285 = CARTESIAN_POINT ( 'NONE',  ( 32.50000000000000711, 26.89999999999999147, 10.55989012756945122 ) ) ;
#33286 = CARTESIAN_POINT ( 'NONE',  ( 7.236395654485760609, 15.02499999726880731, -22.27133577429736633 ) ) ;
#33287 = CARTESIAN_POINT ( 'NONE',  ( 33.58253175000000113, 74.12500000273119838, -4.112674001490185761E-15 ) ) ;
#33288 = CARTESIAN_POINT ( 'NONE',  ( -5.485892052525789174E-07, 66.99999999999998579, 32.49999999999999289 ) ) ;
#33289 = CARTESIAN_POINT ( 'NONE',  ( 8.601468415847516980, 74.67500000273120975, -11.83890561707634603 ) ) ;
#33290 = CARTESIAN_POINT ( 'NONE',  ( 10.37757302488624767, 61.97500000273120691, 31.93888565452638417 ) ) ;
#33291 = CARTESIAN_POINT ( 'NONE',  ( -9.270509831248425314, 77.95000000546239960, -12.75976212528059861 ) ) ;
#33292 = DIRECTION ( 'NONE',  ( -0.000000000000000000, -1.000000000000000000, -0.000000000000000000 ) ) ;
#33293 = CARTESIAN_POINT ( 'NONE',  ( 6.486482029760649416E-15, 19.62500000273116996, 35.31076352940723240 ) ) ;
#33294 = CARTESIAN_POINT ( 'NONE',  ( -15.14183272437241889, 12.44999999453762918, -20.84094480462497856 ) ) ;
#33295 = CARTESIAN_POINT ( 'NONE',  ( -7.025853678916393008, 19.16704833425730570, 26.06988505166735592 ) ) ;
#33296 = CARTESIAN_POINT ( 'NONE',  ( -26.29305231718578995, 26.20000000000000284, 19.10302069950538595 ) ) ;
#33297 = CARTESIAN_POINT ( 'NONE',  ( 10.37757302488624767, 41.72500000273119980, 31.93888565452638417 ) ) ;
#33298 = CARTESIAN_POINT ( 'NONE',  ( 20.75514604977248467, 6.675000002731186655, -28.56700777964554305 ) ) ;
#33299 = CARTESIAN_POINT ( 'NONE',  ( 33.58253175000000113, 58.37500000273119838, -4.112674001490185761E-15 ) ) ;
#33300 = CARTESIAN_POINT ( 'NONE',  ( 20.47846945139902530, 49.53163166759063785, 20.53372385742071771 ) ) ;
#33301 = DIRECTION ( 'NONE',  ( -1.000000000000000000, 0.000000000000000000, 0.000000000000000000 ) ) ;
#33302 = CARTESIAN_POINT ( 'NONE',  ( -7.468012846824272799, 36.91628499907601224, 28.02196122052058413 ) ) ;
#33303 = CARTESIAN_POINT ( 'NONE',  ( -26.29305231718579350, 62.30000000546238681, -19.10302069950537884 ) ) ;
#33304 = AXIS2_PLACEMENT_3D ( 'NONE', #16111, #26562, #464 ) ;
#33305 = CARTESIAN_POINT ( 'NONE',  ( 8.601468415847516980, 80.67500000273118133, -11.83890561707634781 ) ) ;
#33306 = CARTESIAN_POINT ( 'NONE',  ( 6.950374756619257965, 62.69753499907601224, -26.09010956794244507 ) ) ;
#33307 = CARTESIAN_POINT ( 'NONE',  ( -14.47279130897151589, 1.824999997268821339, -19.92008829642072598 ) ) ;
#33308 = CARTESIAN_POINT ( 'NONE',  ( -32.50000000000000000, 74.40000000546234560, -10.55989012756945478 ) ) ;
#33309 = CARTESIAN_POINT ( 'NONE',  ( 15.00000000000000000, 79.00000000000001421, -1.836970198721029589E-15 ) ) ;
#33310 = CARTESIAN_POINT ( 'NONE',  ( -20.75514604977248112, 35.67500000273118843, 28.56700777964554661 ) ) ;
#33311 = CARTESIAN_POINT ( 'NONE',  ( -4.523095164977117273E-15, 10.62499999726880517, 24.62258325217400312 ) ) ;
#33312 = ORIENTED_EDGE ( 'NONE', *, *, #11586, .F. ) ;
#33313 = CARTESIAN_POINT ( 'NONE',  ( -27.16883889988623935, 77.57500000273121543, 19.73931689729374739 ) ) ;
#33314 = CARTESIAN_POINT ( 'NONE',  ( 10.04305231718578817, 23.90000000546237047, -30.90933677959249337 ) ) ;
#33315 = CARTESIAN_POINT ( 'NONE',  ( -26.00068869287340334, 45.65885416666666430, 15.01150461594643382 ) ) ;
#33316 = CARTESIAN_POINT ( 'NONE',  ( 6.277390505771533514E-15, 65.00000000546236834, 34.17252228774368916 ) ) ;
#33317 = ORIENTED_EDGE ( 'NONE', *, *, #20647, .T. ) ;
#33318 =( BOUNDED_CURVE ( )  B_SPLINE_CURVE ( 2, ( #31690, #19457, #8975, #7847, #2707, #3663, #8184, #31355, #6235, #14138, #13168, #18335, #29904 ),
 .UNSPECIFIED., .F., .T. ) 
 B_SPLINE_CURVE_WITH_KNOTS ( ( 3, 2, 2, 2, 2, 2, 3 ),
 ( 0.8611111111111111605, 0.8666666666666666963, 0.8777777777777777679, 0.8888888888888888395, 0.9000000000000000222, 0.9111111111111110938, 0.9166666666666666297 ),
 .UNSPECIFIED. ) 
 CURVE ( )  GEOMETRIC_REPRESENTATION_ITEM ( )  RATIONAL_B_SPLINE_CURVE ( ( 0.9755282581475768211, 0.9755282581475770431, 1.000000000000000000, 0.9510565162951535312, 1.000000000000000000, 0.9510565162951535312, 1.000000000000000000, 0.9510565162951535312, 1.000000000000000000, 0.9510565162951535312, 1.000000000000000000, 0.9755282581475770431, 0.9755282581475768211 ) ) 
 REPRESENTATION_ITEM ( '' )  );
#33319 = CARTESIAN_POINT ( 'NONE',  ( 5.779280353836490358E-15, 73.00000000546236834, 32.49999999999999289 ) ) ;
#33320 = CARTESIAN_POINT ( 'NONE',  ( -33.58253175000000113, 49.22500000273119269, 10.91162601494193929 ) ) ;
#33321 = CARTESIAN_POINT ( 'NONE',  ( -18.94512977948576093, 17.82499999726880446, 13.76444248337722698 ) ) ;
#33322 = CARTESIAN_POINT ( 'NONE',  ( 32.50000000000000000, 5.500000005462357677, -3.980102097228898626E-15 ) ) ;
#33323 = CARTESIAN_POINT ( 'NONE',  ( -32.50000000000000000, 7.900000000000012790, -10.55989012756945300 ) ) ;
#33324 = CARTESIAN_POINT ( 'NONE',  ( 15.01150461594596486, 16.15364583333333215, -26.00068869287367690 ) ) ;
#33325 = VECTOR ( 'NONE', #4359, 1000.000000000000000 ) ;
#33326 = CARTESIAN_POINT ( 'NONE',  ( 10.04305231718578817, 55.40000000000000568, -30.90933677959249337 ) ) ;
#33327 = DIRECTION ( 'NONE',  ( 1.000000000000000000, 0.000000000000000000, 1.224646799147353454E-16 ) ) ;
#33328 = CARTESIAN_POINT ( 'NONE',  ( -10.37757302488623701, 19.77500000273118985, 31.93888565452638417 ) ) ;
#33329 = CARTESIAN_POINT ( 'NONE',  ( 23.95873412499999944, 0.3124999986344190184, 0.000000000000000000 ) ) ;
#33330 = CARTESIAN_POINT ( 'NONE',  ( 19.11951029504797006, 26.03086833240935860, 19.06425588902558133 ) ) ;
#33331 = CARTESIAN_POINT ( 'NONE',  ( 11.25946833292375793, 76.57500000273120122, -8.180482586598735395 ) ) ;
#33332 = CARTESIAN_POINT ( 'NONE',  ( -10.04305231718579172, 55.59999999999999432, -30.90933677959248982 ) ) ;
#33333 = CARTESIAN_POINT ( 'NONE',  ( 5.779280353836490358E-15, 53.00000000546238255, 32.49999999999999289 ) ) ;
#33334 = CARTESIAN_POINT ( 'NONE',  ( -10.04305231718578462, 2.399999999999999467, 30.90933677959249337 ) ) ;
#33335 = ORIENTED_EDGE ( 'NONE', *, *, #25184, .F. ) ;
#33336 = CARTESIAN_POINT ( 'NONE',  ( -18.94512977948576093, 14.32499999726880091, 13.76444248337722698 ) ) ;
#33337 = DIRECTION ( 'NONE',  ( 0.8660254037844388186, -0.000000000000000000, 0.4999999999999997780 ) ) ;
#33338 = CARTESIAN_POINT ( 'NONE',  ( -19.09188309203660694, 52.39062499999999289, 19.09188309203694800 ) ) ;
#33339 = CARTESIAN_POINT ( 'NONE',  ( 33.58253175000000113, 62.12500000273117706, -4.112674001490185761E-15 ) ) ;
#33340 = CARTESIAN_POINT ( 'NONE',  ( -10.37757302488623701, 21.77500000273117919, 31.93888565452638417 ) ) ;
#33341 = CARTESIAN_POINT ( 'NONE',  ( -10.37757302488624411, 10.97500000273120335, -31.93888565452638417 ) ) ;
#33342 = CARTESIAN_POINT ( 'NONE',  ( -24.20753774853730889, 28.47135416666666430, 13.97622843553634020 ) ) ;
#33343 = CARTESIAN_POINT ( 'NONE',  ( -20.75514604977248112, 3.675000002731179105, 28.56700777964554661 ) ) ;
#33344 = CARTESIAN_POINT ( 'NONE',  ( 15.04653450569292872, 24.46652750092397355, -25.98046417659857710 ) ) ;
#33345 = CARTESIAN_POINT ( 'NONE',  ( -20.50609665441004736, 60.12500000000000000, -20.50609665440969565 ) ) ;
#33346 = CARTESIAN_POINT ( 'NONE',  ( 10.37757302488624767, 3.725000002731182480, 31.93888565452638417 ) ) ;
#33347 = CARTESIAN_POINT ( 'NONE',  ( 5.779280353836490358E-15, 2.500000000000005329, 32.49999999999999289 ) ) ;
#33348 = CARTESIAN_POINT ( 'NONE',  ( -20.08610463437156923, 40.30000000000001137, 27.64615127144130113 ) ) ;
#33349 = CARTESIAN_POINT ( 'NONE',  ( 20.75514604977248467, 42.42500000273117422, -28.56700777964554305 ) ) ;
#33350 = CARTESIAN_POINT ( 'NONE',  ( -18.94512977948576093, 3.824999997268818674, 13.76444248337722698 ) ) ;
#33351 = FACE_BOUND ( 'NONE', #10367, .T. ) ;
#33352 = ORIENTED_EDGE ( 'NONE', *, *, #32630, .F. ) ;
#33353 = EDGE_CURVE ( 'NONE', #27958, #21102, #9356, .T. ) ;
#33354 = CARTESIAN_POINT ( 'NONE',  ( 20.75514604977248467, 52.67500000273116711, -28.56700777964554305 ) ) ;
#33355 = CARTESIAN_POINT ( 'NONE',  ( 20.08610463437157279, 59.80000000546235839, -27.64615127144129758 ) ) ;
#33356 = CARTESIAN_POINT ( 'NONE',  ( -19.11951029504763611, 33.20350666759063074, 19.06425588902592239 ) ) ;
#33357 = CARTESIAN_POINT ( 'NONE',  ( -10.37757302488624411, 74.97500000273119269, -31.93888565452638417 ) ) ;
#33358 = EDGE_CURVE ( 'NONE', #27962, #14241, #6960, .T. ) ;
#33359 = ORIENTED_EDGE ( 'NONE', *, *, #29363, .T. ) ;
#33360 = CARTESIAN_POINT ( 'NONE',  ( 33.58253175000000823, 30.02500000273118985, 10.91162601494192863 ) ) ;
#33361 = CARTESIAN_POINT ( 'NONE',  ( -4.223320258572821363E-15, 80.50000000000001421, 15.00000000000000355 ) ) ;
#33362 = VERTEX_POINT ( 'NONE', #4237 ) ;
#33363 = CARTESIAN_POINT ( 'NONE',  ( 23.41746824999999887, 1.124999997268810725, 0.000000000000000000 ) ) ;
#33364 = CARTESIAN_POINT ( 'NONE',  ( -20.75514604977248112, 65.42500000273118133, 28.56700777964554661 ) ) ;
#33365 = CARTESIAN_POINT ( 'NONE',  ( -28.01184896238304134, 42.65104166666666430, -7.505752307972844761 ) ) ;
#33366 = CARTESIAN_POINT ( 'NONE',  ( 19.82091636218621389, 14.19999999999999041, -14.40073868116559197 ) ) ;
#33367 = CARTESIAN_POINT ( 'NONE',  ( 18.94512977948576093, 5.324999997268820451, -13.76444248337722875 ) ) ;
#33368 = CARTESIAN_POINT ( 'NONE',  ( 33.58253175000000823, 12.02500000273117742, 10.91162601494192863 ) ) ;
#33369 = DIRECTION ( 'NONE',  ( -1.224646799147353454E-16, 1.000000000000000000, -0.000000000000000000 ) ) ;
#33370 = CARTESIAN_POINT ( 'NONE',  ( -26.02091320914878025, 55.10638916574269786, -14.97647472619899389 ) ) ;
#33371 = CARTESIAN_POINT ( 'NONE',  ( 4.635254915624212657, 72.59999999999999432, 14.26584774442730286 ) ) ;
#33372 = CARTESIAN_POINT ( 'NONE',  ( 15.01150461594596486, 64.27864583333332860, -26.00068869287367690 ) ) ;
#33373 = CARTESIAN_POINT ( 'NONE',  ( 26.29305231718578995, 55.20000000000000995, -19.10302069950538240 ) ) ;
#33374 = CARTESIAN_POINT ( 'NONE',  ( 26.29305231718578995, 23.19999999999999929, -19.10302069950538240 ) ) ;
#33375 = CARTESIAN_POINT ( 'NONE',  ( 24.50000000000000000, 13.74999999453763166, 0.000000000000000000 ) ) ;
#33376 = CARTESIAN_POINT ( 'NONE',  ( -9.270509831248421762, 78.55000000546236549, 12.75976212528060039 ) ) ;
#33377 = CARTESIAN_POINT ( 'NONE',  ( -24.20753774853730889, 21.59635416666666785, 13.97622843553633842 ) ) ;
#33378 = CARTESIAN_POINT ( 'NONE',  ( 10.37757302488624056, 28.52500000273120051, -31.93888565452638417 ) ) ;
#33379 = CARTESIAN_POINT ( 'NONE',  ( 2.375766604868046361, 74.55125428154681799, 14.99999999999999822 ) ) ;
#33380 = CARTESIAN_POINT ( 'NONE',  ( 20.75514604977249178, 42.07500000273117990, 28.56700777964553950 ) ) ;
#33381 = CARTESIAN_POINT ( 'NONE',  ( 27.16883889988624290, 20.17500000273120264, 19.73931689729373673 ) ) ;
#33382 = DIRECTION ( 'NONE',  ( -0.000000000000000000, -1.000000000000000000, -0.000000000000000000 ) ) ;
#33383 = CARTESIAN_POINT ( 'NONE',  ( 20.75514604977248467, 74.42500000273119554, -28.56700777964554305 ) ) ;
#33384 = CARTESIAN_POINT ( 'NONE',  ( -26.29305231718578995, 66.19999999999997442, 19.10302069950538595 ) ) ;
#33385 = CARTESIAN_POINT ( 'NONE',  ( 20.08610463437157279, 57.29999999999999005, -27.64615127144129758 ) ) ;
#33386 = CARTESIAN_POINT ( 'NONE',  ( -14.47279130897152299, 15.92499999726881121, 19.92008829642072243 ) ) ;
#33387 = CARTESIAN_POINT ( 'NONE',  ( -33.58253175000000113, 63.12500000273119127, 0.000000000000000000 ) ) ;
#33388 = CARTESIAN_POINT ( 'NONE',  ( 7.236395654485755280, 2.724999997268801266, 22.27133577429736988 ) ) ;
#33389 = CARTESIAN_POINT ( 'NONE',  ( 24.22776226481265383, 39.63763916574268364, 13.94119854578893580 ) ) ;
#33390 = FACE_OUTER_BOUND ( 'NONE', #11702, .T. ) ;
#33391 = CARTESIAN_POINT ( 'NONE',  ( 33.58253175000000113, 4.125000002731193938, -4.112674001490185761E-15 ) ) ;
#33392 = CARTESIAN_POINT ( 'NONE',  ( 18.94512977948576093, 11.32499999726882578, -13.76444248337722875 ) ) ;
#33393 = CARTESIAN_POINT ( 'NONE',  ( -19.09188309203660694, 66.14062500000000000, 19.09188309203694800 ) ) ;
#33394 = EDGE_LOOP ( 'NONE', ( #15269, #17035, #20124, #25080 ) ) ;
#33395 = CARTESIAN_POINT ( 'NONE',  ( -33.58253175000000113, 51.12500000273119127, 0.000000000000000000 ) ) ;
#33396 = CARTESIAN_POINT ( 'NONE',  ( -10.37757302488623701, 23.77500000273117919, 31.93888565452638417 ) ) ;
#33397 = EDGE_CURVE ( 'NONE', #28001, #16741, #6760, .T. ) ;
#33398 = ADVANCED_FACE ( 'NONE', ( #22427 ), #20210, .F. ) ;
#33399 = ORIENTED_EDGE ( 'NONE', *, *, #4186, .F. ) ;
#33400 = CARTESIAN_POINT ( 'NONE',  ( 28.01184896238304134, 34.05729166666666430, 7.505752307972846538 ) ) ;
#33401 = CARTESIAN_POINT ( 'NONE',  ( 20.47846945139902530, 28.90663166759063785, 20.53372385742071771 ) ) ;
#33402 = CARTESIAN_POINT ( 'NONE',  ( 24.50000000000000000, 9.900000000000007461, 7.960532557706212486 ) ) ;
#33403 = CARTESIAN_POINT ( 'NONE',  ( -15.14183272437242778, 9.049999994537618164, 20.84094480462497856 ) ) ;
#33404 = CARTESIAN_POINT ( 'NONE',  ( 23.41746824999999887, 7.124999997268815832, 0.000000000000000000 ) ) ;
#33405 = CARTESIAN_POINT ( 'NONE',  ( -14.47279130897151589, 9.324999997268816898, -19.92008829642072598 ) ) ;
#33406 = CARTESIAN_POINT ( 'NONE',  ( -33.58253175000000113, 17.47500000273117848, 10.91162601494193929 ) ) ;
#33407 = CARTESIAN_POINT ( 'NONE',  ( -2.092463501923844636E-15, 22.00000000546238965, -34.17252228774368916 ) ) ;
#33408 = CARTESIAN_POINT ( 'NONE',  ( -10.04305231718578462, 68.40000000000001990, 30.90933677959249337 ) ) ;
#33409 = CARTESIAN_POINT ( 'NONE',  ( 0.000000000000000000, 111.9999999999999858, 11.32050807568876749 ) ) ;
#33410 = CARTESIAN_POINT ( 'NONE',  ( 4.250625530119172879, 74.00000000000000000, 13.31398618829670788 ) ) ;
#33411 = CARTESIAN_POINT ( 'NONE',  ( -15.01150461594595775, 14.43489583333332682, 26.00068869287368756 ) ) ;
#33412 = CARTESIAN_POINT ( 'NONE',  ( 6.486482029760649416E-15, 31.87500000273119127, 35.31076352940723240 ) ) ;
#33413 = CARTESIAN_POINT ( 'NONE',  ( 32.50000000000000711, 43.40000000546238113, 10.55989012756945122 ) ) ;
#33414 = CARTESIAN_POINT ( 'NONE',  ( 28.01184896238304134, 44.36979166666666430, 7.505752307972846538 ) ) ;
#33415 = CARTESIAN_POINT ( 'NONE',  ( 0.000000000000000000, 0.000000000000000000, 0.000000000000000000 ) ) ;
#33416 = CARTESIAN_POINT ( 'NONE',  ( 1.507698388325705758E-15, 15.62499999726882116, -24.62258325217400312 ) ) ;
#33417 = CARTESIAN_POINT ( 'NONE',  ( -32.50000000000000000, 10.10000000000000142, 10.55989012756946366 ) ) ;
#33418 = CARTESIAN_POINT ( 'NONE',  ( -11.54700538379251817, 86.00000000000001421, 19.99999999999999645 ) ) ;
#33419 = CARTESIAN_POINT ( 'NONE',  ( -26.09010956794245217, 51.52565999907602645, -6.950374756619243755 ) ) ;
#33420 = CARTESIAN_POINT ( 'NONE',  ( 10.37757302488624767, 47.72500000273119269, 31.93888565452638417 ) ) ;
#33421 = CARTESIAN_POINT ( 'NONE',  ( -20.75514604977248823, 63.07500000273119412, -28.56700777964554305 ) ) ;
#33422 = CARTESIAN_POINT ( 'NONE',  ( 33.58253175000000823, 40.27500000273118985, 10.91162601494192685 ) ) ;
#33423 =( BOUNDED_CURVE ( )  B_SPLINE_CURVE ( 2, ( #29028, #24067, #23727, #26298, #3293, #3129, #13602, #367, #16343, #8101, #533, #28696, #11020 ),
 .UNSPECIFIED., .F., .F. ) 
 B_SPLINE_CURVE_WITH_KNOTS ( ( 3, 2, 2, 2, 2, 2, 3 ),
 ( 0.5448717948717948234, 0.5461538461538461009, 0.5487179487179487669, 0.5512820512820513219, 0.5538461538461538769, 0.5564102564102564319, 0.5576923076923077094 ),
 .UNSPECIFIED. ) 
 CURVE ( )  GEOMETRIC_REPRESENTATION_ITEM ( )  RATIONAL_B_SPLINE_CURVE ( ( 0.9755282581475768211, 0.9755282581475768211, 1.000000000000000000, 0.9510565162951535312, 1.000000000000000000, 0.9510565162951535312, 1.000000000000000000, 0.9510565162951535312, 1.000000000000000000, 0.9510565162951535312, 1.000000000000000000, 0.9755282581475768211, 0.9755282581475768211 ) ) 
 REPRESENTATION_ITEM ( '' )  );
#33424 = CARTESIAN_POINT ( 'NONE',  ( 7.236395654485755280, 16.22499999726881370, 22.27133577429736988 ) ) ;
#33425 = CARTESIAN_POINT ( 'NONE',  ( 26.07999730980490227, 13.43229166666666607, 6.988114217767821046 ) ) ;
#33426 = CARTESIAN_POINT ( 'NONE',  ( 6.486482029760649416E-15, 1.625000002731185944, 35.31076352940723240 ) ) ;
#33427 = CARTESIAN_POINT ( 'NONE',  ( -24.46341963991828550, 16.99999999999998579, -0.9880410939973442996 ) ) ;
#33428 = CARTESIAN_POINT ( 'NONE',  ( 20.08610463437157279, 77.30000000000001137, -27.64615127144129758 ) ) ;
#33429 = CARTESIAN_POINT ( 'NONE',  ( -27.16883889988624290, 24.92500000273119198, -19.73931689729374028 ) ) ;
#33430 = CARTESIAN_POINT ( 'NONE',  ( -10.04305231718579172, 62.10000000546239818, -30.90933677959248982 ) ) ;
#33431 = DIRECTION ( 'NONE',  ( 0.000000000000000000, -0.000000000000000000, -1.000000000000000000 ) ) ;
#33432 = CYLINDRICAL_SURFACE ( 'NONE', #27530, 32.50000000000000000 ) ;
#33433 = CARTESIAN_POINT ( 'NONE',  ( 20.53372385742108008, 67.28086833240935505, 20.47846945139866648 ) ) ;
#33434 = CARTESIAN_POINT ( 'NONE',  ( 10.04305231718579705, 41.10000000546236265, 30.90933677959248982 ) ) ;
#33435 = DIRECTION ( 'NONE',  ( 0.000000000000000000, 1.000000000000000000, 0.000000000000000000 ) ) ;
#33436 = CARTESIAN_POINT ( 'NONE',  ( -10.37757302488623701, 33.52500000273117564, 31.93888565452638417 ) ) ;
#33437 = CARTESIAN_POINT ( 'NONE',  ( -10.37757302488623701, 65.77500000273117564, 31.93888565452638417 ) ) ;
#33438 = CARTESIAN_POINT ( 'NONE',  ( 6.988114217768294445, 38.06770833333332860, 26.07999730980477437 ) ) ;
#33439 = EDGE_LOOP ( 'NONE', ( #11615, #28082 ) ) ;
#33440 = CARTESIAN_POINT ( 'NONE',  ( 6.486482029760649416E-15, 71.62500000273119838, 35.31076352940723240 ) ) ;
#33441 = CARTESIAN_POINT ( 'NONE',  ( 26.00068869287340334, 40.50260416666666430, -15.01150461594642316 ) ) ;
#33442 = DIRECTION ( 'NONE',  ( 1.000000000000000000, 0.000000000000000000, 0.000000000000000000 ) ) ;
#33443 = ORIENTED_EDGE ( 'NONE', *, *, #31596, .F. ) ;
#33444 = CARTESIAN_POINT ( 'NONE',  ( -25.98046417659859486, 54.54465250092398776, -15.04653450569291628 ) ) ;
#33445 = CARTESIAN_POINT ( 'NONE',  ( -24.18731323226248264, 61.41965250092398776, -14.01125832528284931 ) ) ;
#33446 = CARTESIAN_POINT ( 'NONE',  ( 27.16883889988624290, 13.92500000273118310, 19.73931689729373673 ) ) ;
#33447 = CARTESIAN_POINT ( 'NONE',  ( 11.54700538379251817, 96.00000000000002842, 19.99999999999999645 ) ) ;
#33448 = CARTESIAN_POINT ( 'NONE',  ( -30.02300923189239867, 20.44493083240935150, 0.04044903255044988294 ) ) ;
#33449 = CARTESIAN_POINT ( 'NONE',  ( 4.635254915624212657, 78.85000000546239107, 14.26584774442730286 ) ) ;
#33450 = CARTESIAN_POINT ( 'NONE',  ( -20.75514604977248823, 35.07500000273120833, -28.56700777964554305 ) ) ;
#33451 = CARTESIAN_POINT ( 'NONE',  ( -32.50000000000000000, 42.50000000546238965, 0.000000000000000000 ) ) ;
#33452 = CARTESIAN_POINT ( 'NONE',  ( -9.270509831248421762, 76.30000000000003979, 12.75976212528060039 ) ) ;
#33453 = CARTESIAN_POINT ( 'NONE',  ( 27.16883889988623935, 22.32500000273118701, -19.73931689729374384 ) ) ;
#33454 = CARTESIAN_POINT ( 'NONE',  ( 5.147494310547426899, 31.94874572391553258, -32.50000000000000000 ) ) ;
#33455 = CARTESIAN_POINT ( 'NONE',  ( 20.75514604977248467, 48.67500000273117422, -28.56700777964554305 ) ) ;
#33456 = CARTESIAN_POINT ( 'NONE',  ( -20.08610463437156923, 30.30000000000000426, 27.64615127144130113 ) ) ;
#33457 = CARTESIAN_POINT ( 'NONE',  ( 32.50000000000000000, 28.99999999999999645, -3.980102097228898626E-15 ) ) ;
#33458 = CARTESIAN_POINT ( 'NONE',  ( 23.41746825000000243, 14.72499999726881903, -7.608796670333727974 ) ) ;
#33459 = CARTESIAN_POINT ( 'NONE',  ( 10.37757302488624056, 74.52500000273118985, -31.93888565452638417 ) ) ;
#33460 = CARTESIAN_POINT ( 'NONE',  ( 20.08610463437158344, 62.69999999999998863, 27.64615127144129403 ) ) ;
#33461 = CARTESIAN_POINT ( 'NONE',  ( 7.313012447739250820E-14, 15.50000000000000178, 24.50000000000000000 ) ) ;
#33462 = CARTESIAN_POINT ( 'NONE',  ( 33.58253175000000823, 58.27500000273116854, 10.91162601494192685 ) ) ;
#33463 = CARTESIAN_POINT ( 'NONE',  ( -15.00000000000000000, 74.35000000546239107, 4.873795443493597723 ) ) ;
#33464 = CARTESIAN_POINT ( 'NONE',  ( 23.09401076758502569, 86.00000000000001421, -6.857326241137392698E-15 ) ) ;
#33465 = CARTESIAN_POINT ( 'NONE',  ( -10.37757302488623701, 21.52500000273119340, 31.93888565452638417 ) ) ;
#33466 = CARTESIAN_POINT ( 'NONE',  ( -7.570916362186215665, 11.14999999453764090, 23.30088464923126423 ) ) ;
#33467 = CARTESIAN_POINT ( 'NONE',  ( -6.950374756619716266, 24.03684000092397000, -26.09010956794232428 ) ) ;
#33468 = CARTESIAN_POINT ( 'NONE',  ( -20.08610463437156923, 26.29999999999998295, 27.64615127144130113 ) ) ;
#33469 = CARTESIAN_POINT ( 'NONE',  ( 10.37757302488624056, 42.52500000273119696, -31.93888565452638417 ) ) ;
#33470 = DIRECTION ( 'NONE',  ( 0.000000000000000000, 0.000000000000000000, -1.000000000000000000 ) ) ;
#33471 = CARTESIAN_POINT ( 'NONE',  ( -10.37757302488624411, 58.97500000273119269, -31.93888565452638417 ) ) ;
#33472 = CARTESIAN_POINT ( 'NONE',  ( 25.98046417659858420, 45.95090250092398065, 15.04653450569292872 ) ) ;
#33473 = LINE ( 'NONE', #8990, #31912 ) ;
#33474 = CARTESIAN_POINT ( 'NONE',  ( -25.98046417659831420, 33.90847249907601935, 15.04653450569339945 ) ) ;
#33475 = CARTESIAN_POINT ( 'NONE',  ( 20.08610463437157279, 61.80000000546237970, -27.64615127144129758 ) ) ;
#33476 = CARTESIAN_POINT ( 'NONE',  ( -8.601468415847518756, 81.07500000273115859, -11.83890561707634781 ) ) ;
#33477 = CARTESIAN_POINT ( 'NONE',  ( 3.778760231354629433E-15, 2.249999994537632553, -24.50000000000000355 ) ) ;
#33478 = CARTESIAN_POINT ( 'NONE',  ( 27.95245687107223276, 63.41368083240934794, -0.04044903255042905932 ) ) ;
#33479 = CARTESIAN_POINT ( 'NONE',  ( 32.50000000000000000, 63.50000000546238255, -3.980102097228898626E-15 ) ) ;
#33480 = CARTESIAN_POINT ( 'NONE',  ( 26.29305231718579350, 77.30000000546239391, 19.10302069950537529 ) ) ;
#33481 = CARTESIAN_POINT ( 'NONE',  ( -20.50609665441004736, 11.99999999999999645, -20.50609665440969565 ) ) ;
#33482 = VECTOR ( 'NONE', #33301, 1000.000000000000000 ) ;
#33483 = EDGE_CURVE ( 'NONE', #2126, #15317, #27922, .T. ) ;
#33484 = CARTESIAN_POINT ( 'NONE',  ( 10.37757302488624767, 33.97500000273119269, 31.93888565452638417 ) ) ;
#33485 = CARTESIAN_POINT ( 'NONE',  ( 1.507698388325705758E-15, 5.624999997268818497, -24.62258325217400312 ) ) ;
#33486 = VERTEX_POINT ( 'NONE', #22945 ) ;
#33487 = CARTESIAN_POINT ( 'NONE',  ( -33.58253175000000113, 75.27500000273118985, -10.91162601494193218 ) ) ;
#33488 = CARTESIAN_POINT ( 'NONE',  ( 6.277390505771533514E-15, 23.00000000546238610, 34.17252228774368916 ) ) ;
#33489 = CARTESIAN_POINT ( 'NONE',  ( -28.01184896238304134, 42.65104166666666430, -7.505752307972844761 ) ) ;
#33490 = CARTESIAN_POINT ( 'NONE',  ( -32.50000000000000000, 64.60000000546237686, 10.55989012756946366 ) ) ;
#33491 = ORIENTED_EDGE ( 'NONE', *, *, #7267, .F. ) ;
#33492 = CARTESIAN_POINT ( 'NONE',  ( -32.50000000000000000, 10.60000000546237153, 10.55989012756946366 ) ) ;
#33493 = AXIS2_PLACEMENT_3D ( 'NONE', #14215, #21940, #19200 ) ;
#33494 = CARTESIAN_POINT ( 'NONE',  ( 33.58253175000000113, 40.12500000273119838, -4.112674001490185761E-15 ) ) ;
#33495 = CARTESIAN_POINT ( 'NONE',  ( 32.50000000000000000, 55.60000000546237686, -10.55989012756945833 ) ) ;
#33496 = CARTESIAN_POINT ( 'NONE',  ( 6.277390505771533514E-15, 5.000000005462374553, 34.17252228774368916 ) ) ;
#33497 = CARTESIAN_POINT ( 'NONE',  ( -10.37757302488624411, 66.72500000273116427, -31.93888565452638417 ) ) ;
#33498 = CARTESIAN_POINT ( 'NONE',  ( 30.02300923189239867, 16.72656249999999645, -2.619432448724978208E-13 ) ) ;
#33499 = CARTESIAN_POINT ( 'NONE',  ( -32.50000000000000000, 49.89999999999999147, -10.55989012756945478 ) ) ;
#33500 = CARTESIAN_POINT ( 'NONE',  ( -26.29305231718578995, 14.19999999999999041, 19.10302069950538595 ) ) ;
#33501 = CARTESIAN_POINT ( 'NONE',  ( 27.16883889988623935, 16.57500000273118346, -19.73931689729374384 ) ) ;
#33502 = CARTESIAN_POINT ( 'NONE',  ( -10.04305231718578462, 74.40000000000001990, 30.90933677959249337 ) ) ;
#33503 = CARTESIAN_POINT ( 'NONE',  ( -26.09010956794245217, 27.46315999907601935, -6.950374756619243755 ) ) ;
#33504 = CARTESIAN_POINT ( 'NONE',  ( 2.688165632520823219E-15, 77.87500000273118417, 14.63369212191046387 ) ) ;
#33505 = CARTESIAN_POINT ( 'NONE',  ( 10.37757302488624056, 78.77500000273118985, -31.93888565452638417 ) ) ;
#33506 = CARTESIAN_POINT ( 'NONE',  ( 10.04305231718578817, 53.90000000546238113, -30.90933677959249337 ) ) ;
#33507 = CARTESIAN_POINT ( 'NONE',  ( -33.58253175000000113, 73.47500000273117848, 10.91162601494193929 ) ) ;
#33508 = VERTEX_POINT ( 'NONE', #23113 ) ;
#33509 = CARTESIAN_POINT ( 'NONE',  ( -4.523095164977116484E-15, 14.62499999726882649, 24.62258325217400312 ) ) ;
#33510 = CARTESIAN_POINT ( 'NONE',  ( -14.47279130897151767, 7.324999997268822227, -19.92008829642072598 ) ) ;
#33511 = CARTESIAN_POINT ( 'NONE',  ( -24.20753774853756823, 53.10677083333331439, -13.97622843553588723 ) ) ;
#33512 = CARTESIAN_POINT ( 'NONE',  ( 33.58253175000000113, 60.22500000273119980, -10.91162601494193751 ) ) ;
#33513 = CARTESIAN_POINT ( 'NONE',  ( -10.37757302488624411, 20.97500000273118559, -31.93888565452638417 ) ) ;
#33514 = CARTESIAN_POINT ( 'NONE',  ( 27.16883889988623935, 12.57500000273119234, -19.73931689729374384 ) ) ;
#33515 = CARTESIAN_POINT ( 'NONE',  ( -6.988114217768288228, 32.91145833333332860, -26.07999730980477437 ) ) ;
#33516 = UNCERTAINTY_MEASURE_WITH_UNIT (LENGTH_MEASURE( 1.000000000000000082E-05 ), #16877, 'distance_accuracy_value', 'NONE');
#33517 = CARTESIAN_POINT ( 'NONE',  ( 0.04044903254992426173, 17.30506916759064140, -30.02300923189239867 ) ) ;
#33518 = CARTESIAN_POINT ( 'NONE',  ( -28.01184896238304134, 66.71354166666665719, -7.505752307972844761 ) ) ;
#33519 = CARTESIAN_POINT ( 'NONE',  ( 10.37757302488624056, 2.525000002731189852, -31.93888565452638417 ) ) ;
#33520 = CARTESIAN_POINT ( 'NONE',  ( 2.688165632520823219E-15, 71.87500000273121259, 14.63369212191046209 ) ) ;
#33521 = CARTESIAN_POINT ( 'NONE',  ( -2.092463501923844636E-15, 43.49999999999999289, -34.17252228774368916 ) ) ;
#33522 = CIRCLE ( 'NONE', #2294, 30.50000000000000000 ) ;
#33523 = CARTESIAN_POINT ( 'NONE',  ( 33.58253175000000113, 46.12500000273117706, -4.112674001490185761E-15 ) ) ;
#33524 = CARTESIAN_POINT ( 'NONE',  ( 23.41746825000000243, 8.524999997268812635, 7.608796670333735079 ) ) ;
#33525 = CARTESIAN_POINT ( 'NONE',  ( 5.147494310547434893, 21.05125428700922185, 32.49999999999999289 ) ) ;
#33526 = VERTEX_POINT ( 'NONE', #7147 ) ;
#33527 = CARTESIAN_POINT ( 'NONE',  ( 20.75514604977248467, 54.67500000273119554, -28.56700777964554305 ) ) ;
#33528 =( BOUNDED_CURVE ( )  B_SPLINE_CURVE ( 2, ( #26604, #16814, #13731, #2927, #23868, #10821, #3102, #21301, #31741, #26772, #5998, #8232, #29335 ),
 .UNSPECIFIED., .F., .T. ) 
 B_SPLINE_CURVE_WITH_KNOTS ( ( 3, 2, 2, 2, 2, 2, 3 ),
 ( 0.7628205128205127750, 0.7641025641025640525, 0.7666666666666667185, 0.7692307692307692735, 0.7717948717948718285, 0.7743589743589743835, 0.7756410256410256610 ),
 .UNSPECIFIED. ) 
 CURVE ( )  GEOMETRIC_REPRESENTATION_ITEM ( )  RATIONAL_B_SPLINE_CURVE ( ( 0.9755282581475768211, 0.9755282581475768211, 1.000000000000000000, 0.9510565162951535312, 1.000000000000000000, 0.9510565162951535312, 1.000000000000000000, 0.9510565162951535312, 1.000000000000000000, 0.9510565162951535312, 1.000000000000000000, 0.9755282581475768211, 0.9755282581475768211 ) ) 
 REPRESENTATION_ITEM ( '' )  );
#33529 = CYLINDRICAL_SURFACE ( 'NONE', #2578, 15.00000000000000000 ) ;
#33530 = CARTESIAN_POINT ( 'NONE',  ( 0.04044903254993986036, 41.36756916759064495, -27.95245687107223986 ) ) ;
#33531 = CARTESIAN_POINT ( 'NONE',  ( 27.16883889988623935, 74.57500000273120122, -19.73931689729374384 ) ) ;
#33532 = EDGE_LOOP ( 'NONE', ( #33705, #22263, #11551, #20288 ) ) ;
#33533 = CARTESIAN_POINT ( 'NONE',  ( -2.162160676586881955E-15, 24.62500000273118772, -35.31076352940723240 ) ) ;
#33534 = CARTESIAN_POINT ( 'NONE',  ( -15.01150461594595775, 14.43489583333332682, 26.00068869287368756 ) ) ;
#33535 = ORIENTED_EDGE ( 'NONE', *, *, #7163, .T. ) ;
#33536 = DIRECTION ( 'NONE',  ( 0.000000000000000000, 0.000000000000000000, -1.000000000000000000 ) ) ;
#33537 = CARTESIAN_POINT ( 'NONE',  ( -27.16883889988623935, 65.32500000273117280, 19.73931689729374739 ) ) ;
#33538 = CARTESIAN_POINT ( 'NONE',  ( -26.00068869287368756, 42.79427083333331439, -15.01150461594595775 ) ) ;
#33539 = CARTESIAN_POINT ( 'NONE',  ( -7.570916362186210335, 14.60000000000000142, -23.30088464923126779 ) ) ;
#33540 = LINE ( 'NONE', #23079, #2929 ) ;
#33541 = CARTESIAN_POINT ( 'NONE',  ( -10.37757302488624411, 8.725000002731187365, -31.93888565452638417 ) ) ;
#33542 = PRESENTATION_STYLE_ASSIGNMENT (( #7632 ) ) ;
#33543 = CARTESIAN_POINT ( 'NONE',  ( -14.97647472619899389, 50.80951416574269075, 26.02091320914878025 ) ) ;
#33544 = CARTESIAN_POINT ( 'NONE',  ( 15.00000000000000000, 75.09999999999999432, -4.873795443493596835 ) ) ;
#33545 = CARTESIAN_POINT ( 'NONE',  ( 0.000000000000000000, 111.9999999999999858, 0.000000000000000000 ) ) ;
#33546 = CARTESIAN_POINT ( 'NONE',  ( -19.82091636218621389, 14.94999999453763806, 14.40073868116558842 ) ) ;
#33547 = DIRECTION ( 'NONE',  ( 0.000000000000000000, -0.000000000000000000, 1.000000000000000000 ) ) ;
#33548 = CARTESIAN_POINT ( 'NONE',  ( -24.50000000000000000, 12.74999999453763166, -3.000384657911015469E-15 ) ) ;
#33549 = CARTESIAN_POINT ( 'NONE',  ( 9.270509831248423538, 71.55000000546239391, -12.75976212528059861 ) ) ;
#33550 = CARTESIAN_POINT ( 'NONE',  ( -24.20753774853756823, 18.73177083333332149, -13.97622843553588723 ) ) ;
#33551 = EDGE_CURVE ( 'NONE', #2770, #19648, #12124, .T. ) ;
#33552 = CARTESIAN_POINT ( 'NONE',  ( 33.58253175000000823, 28.02500000273119340, 10.91162601494192863 ) ) ;
#33553 = CARTESIAN_POINT ( 'NONE',  ( -10.37757302488623701, 77.52500000273120406, 31.93888565452638417 ) ) ;
#33554 = CARTESIAN_POINT ( 'NONE',  ( 6.486482029760649416E-15, 45.87500000273117706, 35.31076352940723240 ) ) ;
#33555 = CARTESIAN_POINT ( 'NONE',  ( -20.75514604977248823, 25.07500000273120122, -28.56700777964554305 ) ) ;
#33556 = CARTESIAN_POINT ( 'NONE',  ( -3.880418787951104953, 17.19874571299077104, 24.50000000000000711 ) ) ;
#33557 = ADVANCED_FACE ( 'NONE', ( #14882 ), #25521, .T. ) ;
#33558 = CARTESIAN_POINT ( 'NONE',  ( 10.37757302488624056, 78.52500000273118985, -31.93888565452638417 ) ) ;
#33559 = CARTESIAN_POINT ( 'NONE',  ( 1.093617666956751375E-13, 60.00000000546237544, -32.50000000000000711 ) ) ;
#33560 = CARTESIAN_POINT ( 'NONE',  ( -20.08610463437156923, 60.29999999999998295, 27.64615127144130113 ) ) ;
#33561 = VECTOR ( 'NONE', #27779, 1000.000000000000000 ) ;
#33562 = CARTESIAN_POINT ( 'NONE',  ( 23.41746824999999887, 16.52499999726882152, 7.608796670333735079 ) ) ;
#33563 = CARTESIAN_POINT ( 'NONE',  ( -10.37757302488624411, 66.72500000273117848, -31.93888565452638417 ) ) ;
#33564 = VECTOR ( 'NONE', #2963, 1000.000000000000000 ) ;
#33565 = CARTESIAN_POINT ( 'NONE',  ( -14.47279130897152122, 6.424999997268821872, 19.92008829642072243 ) ) ;
#33566 = CARTESIAN_POINT ( 'NONE',  ( 27.16883889988624290, 70.17500000273118133, 19.73931689729373673 ) ) ;
#33567 = CARTESIAN_POINT ( 'NONE',  ( -33.58253175000000113, 9.025000002731184523, -10.91162601494193041 ) ) ;
#33568 = CARTESIAN_POINT ( 'NONE',  ( 18.94512977948576093, 13.32499999726882756, -13.76444248337722875 ) ) ;
#33569 = CARTESIAN_POINT ( 'NONE',  ( -26.06988505166735237, 16.58892333425730570, -7.025853678916388567 ) ) ;
#33570 = VERTEX_POINT ( 'NONE', #12300 ) ;
#33571 = CARTESIAN_POINT ( 'NONE',  ( -20.75514604977248823, 44.82500000273117990, -28.56700777964554305 ) ) ;
#33572 = VERTEX_POINT ( 'NONE', #10074 ) ;
#33573 = CARTESIAN_POINT ( 'NONE',  ( 26.00068869287340334, 33.62760416666665719, -15.01150461594642316 ) ) ;
#33574 = CARTESIAN_POINT ( 'NONE',  ( 0.000000000000000000, 111.9999999999999858, 0.000000000000000000 ) ) ;
#33575 = CARTESIAN_POINT ( 'NONE',  ( -20.08610463437157989, 6.200000005462380948, -27.64615127144129758 ) ) ;
#33576 = DIRECTION ( 'NONE',  ( 0.000000000000000000, 0.000000000000000000, -1.000000000000000000 ) ) ;
#33577 = CARTESIAN_POINT ( 'NONE',  ( 24.50000000000000000, 19.74999999453763877, 0.000000000000000000 ) ) ;
#33578 = CARTESIAN_POINT ( 'NONE',  ( 23.41746825000000243, 14.52499999726880020, 7.608796670333735079 ) ) ;
#33579 = CARTESIAN_POINT ( 'NONE',  ( 33.58253175000000113, 16.37500000273117706, -4.112674001490185761E-15 ) ) ;
#33580 = CARTESIAN_POINT ( 'NONE',  ( 32.50000000000000000, 15.50000000546236656, -3.980102097228898626E-15 ) ) ;
#33581 = AXIS2_PLACEMENT_3D ( 'NONE', #13217, #21126, #31569 ) ;
#33582 = CARTESIAN_POINT ( 'NONE',  ( 32.50000000000000000, 69.00000000000000000, -3.980102097228898626E-15 ) ) ;
#33583 = CARTESIAN_POINT ( 'NONE',  ( 10.04305231718578817, 57.90000000546238823, -30.90933677959249337 ) ) ;
#33584 = CARTESIAN_POINT ( 'NONE',  ( 15.01150461594596308, 16.15364583333333215, -26.00068869287367335 ) ) ;
#33585 = CARTESIAN_POINT ( 'NONE',  ( -33.58253175000000113, 33.27500000273120406, -10.91162601494193218 ) ) ;
#33586 = FACE_OUTER_BOUND ( 'NONE', #7228, .T. ) ;
#33587 = CARTESIAN_POINT ( 'NONE',  ( 15.01150461594643382, 41.36197916666665719, 26.00068869287340334 ) ) ;
#33588 = DIRECTION ( 'NONE',  ( 0.000000000000000000, 0.000000000000000000, 1.000000000000000000 ) ) ;
#33589 = AXIS2_PLACEMENT_3D ( 'NONE', #15367, #2135, #18111 ) ;
#33590 = CARTESIAN_POINT ( 'NONE',  ( 18.94512977948576093, 15.32499999726882933, -13.76444248337722875 ) ) ;
#33591 = CARTESIAN_POINT ( 'NONE',  ( 10.04305231718579705, 10.59999999999999787, 30.90933677959248982 ) ) ;
#33592 = CARTESIAN_POINT ( 'NONE',  ( 10.04305231718578817, 17.90000000546238113, -30.90933677959249337 ) ) ;
#33593 = EDGE_CURVE ( 'NONE', #23106, #33921, #27135, .T. ) ;
#33594 = CARTESIAN_POINT ( 'NONE',  ( 24.22776226481265383, 56.82513916574268364, 13.94119854578893580 ) ) ;
#33595 = CARTESIAN_POINT ( 'NONE',  ( -20.75514604977248823, 52.82500000273116569, -28.56700777964554305 ) ) ;
#33596 = CARTESIAN_POINT ( 'NONE',  ( 10.37757302488624056, 64.77500000273118985, -31.93888565452638417 ) ) ;
#33597 = CARTESIAN_POINT ( 'NONE',  ( 20.75514604977249178, 40.07500000273118701, 28.56700777964553950 ) ) ;
#33598 = CARTESIAN_POINT ( 'NONE',  ( -14.47279130897152299, 13.92499999726881654, 19.92008829642072243 ) ) ;
#33599 = CARTESIAN_POINT ( 'NONE',  ( 13.97622843553589966, 12.71614583333333037, -24.20753774853756113 ) ) ;
#33600 = AXIS2_PLACEMENT_3D ( 'NONE', #28959, #10270, #7854 ) ;
#33601 = CARTESIAN_POINT ( 'NONE',  ( -10.04305231718579172, 61.59999999999998721, -30.90933677959248982 ) ) ;
#33602 = CYLINDRICAL_SURFACE ( 'NONE', #1390, 30.50000000000000000 ) ;
#33603 = CARTESIAN_POINT ( 'NONE',  ( 32.50000000000000000, 77.09999999999998010, -10.55989012756945833 ) ) ;
#33604 = CARTESIAN_POINT ( 'NONE',  ( -33.58253175000000113, 13.12500000273118772, 0.000000000000000000 ) ) ;
#33605 = CARTESIAN_POINT ( 'NONE',  ( 26.29305231718578995, 7.199999999999984190, -19.10302069950538240 ) ) ;
#33606 = LINE ( 'NONE', #19885, #24262 ) ;
#33607 = CARTESIAN_POINT ( 'NONE',  ( -27.95245687107223986, 20.44493083240935150, 0.04044903255043252877 ) ) ;
#33608 = CARTESIAN_POINT ( 'NONE',  ( 26.29305231718578995, 41.70000000546237828, -19.10302069950538240 ) ) ;
#33609 = CARTESIAN_POINT ( 'NONE',  ( 19.82091636218621034, 17.54999999453762882, 14.40073868116559730 ) ) ;
#33610 = CARTESIAN_POINT ( 'NONE',  ( 20.75514604977249178, 25.82500000273117990, 28.56700777964553950 ) ) ;
#33611 = CARTESIAN_POINT ( 'NONE',  ( 2.584737979205441561E-13, 34.77343750000000000, 27.95245687107222921 ) ) ;
#33612 = VECTOR ( 'NONE', #16181, 1000.000000000000000 ) ;
#33613 = EDGE_LOOP ( 'NONE', ( #28678, #10372, #2898, #21386 ) ) ;
#33614 = CARTESIAN_POINT ( 'NONE',  ( 33.58253175000000823, 68.02500000273117564, 10.91162601494192863 ) ) ;
#33615 = CARTESIAN_POINT ( 'NONE',  ( -28.01184896238290278, 49.23958333333332860, 7.505752307973363457 ) ) ;
#33616 = CARTESIAN_POINT ( 'NONE',  ( 5.779280353836490358E-15, 17.00000000546237899, 32.49999999999999289 ) ) ;
#33617 = EDGE_LOOP ( 'NONE', ( #16284, #21723, #29093, #28466 ) ) ;
#33618 = CARTESIAN_POINT ( 'NONE',  ( -14.97647472619946285, 61.70611083425731636, -26.02091320914851025 ) ) ;
#33619 = CARTESIAN_POINT ( 'NONE',  ( 6.950374756619721595, 56.69309000092396644, 26.09010956794232428 ) ) ;
#33620 = ORIENTED_EDGE ( 'NONE', *, *, #14403, .F. ) ;
#33621 = CARTESIAN_POINT ( 'NONE',  ( -27.16883889988624290, 8.925000002731206195, -19.73931689729374028 ) ) ;
#33622 = CARTESIAN_POINT ( 'NONE',  ( 0.04044903255045854962, 19.58555583240935860, 30.02300923189239867 ) ) ;
#33623 = CARTESIAN_POINT ( 'NONE',  ( 15.00000000000000000, 79.25000000546239676, -1.836970198721029589E-15 ) ) ;
#33624 = CARTESIAN_POINT ( 'NONE',  ( 10.37757302488624767, 33.97500000273117848, 31.93888565452638417 ) ) ;
#33625 = CARTESIAN_POINT ( 'NONE',  ( 20.08610463437158344, 43.20000000546235697, 27.64615127144129403 ) ) ;
#33626 = CARTESIAN_POINT ( 'NONE',  ( 2.897257156509938333E-15, 76.50000000000002842, 15.77193336357400710 ) ) ;
#33627 = CARTESIAN_POINT ( 'NONE',  ( -30.02300923189239512, 66.57031250000000000, 2.654126918244515359E-13 ) ) ;
#33628 = CARTESIAN_POINT ( 'NONE',  ( 10.37757302488624056, 22.52500000273119340, -31.93888565452638417 ) ) ;
#33629 = CARTESIAN_POINT ( 'NONE',  ( -5.147494043133895580, 52.05125428434654822, -32.50000008688792263 ) ) ;
#33630 = CARTESIAN_POINT ( 'NONE',  ( -2.162160676586881955E-15, 50.87500000273119838, -35.31076352940723240 ) ) ;
#33631 =( BOUNDED_CURVE ( )  B_SPLINE_CURVE ( 2, ( #30601, #18096, #23243, #7097, #33704, #30950, #10203, #28041, #25642, #15525, #1597, #17752, #12424 ),
 .UNSPECIFIED., .F., .T. ) 
 B_SPLINE_CURVE_WITH_KNOTS ( ( 3, 2, 2, 2, 2, 2, 3 ),
 ( 0.2500000000000000000, 0.2600000000000000089, 0.2800000000000000266, 0.2999999999999999889, 0.3200000000000000067, 0.3400000000000000244, 0.3500000000000000333 ),
 .UNSPECIFIED. ) 
 CURVE ( )  GEOMETRIC_REPRESENTATION_ITEM ( )  RATIONAL_B_SPLINE_CURVE ( ( 0.9755282581475768211, 0.9755282581475768211, 1.000000000000000000, 0.9510565162951535312, 1.000000000000000000, 0.9510565162951535312, 1.000000000000000000, 0.9510565162951535312, 1.000000000000000000, 0.9510565162951535312, 1.000000000000000000, 0.9755282581475767101, 0.9755282581475768211 ) ) 
 REPRESENTATION_ITEM ( '' )  );
#33632 = CARTESIAN_POINT ( 'NONE',  ( -26.29305231718578995, 30.19999999999999218, 19.10302069950538595 ) ) ;
#33633 = CARTESIAN_POINT ( 'NONE',  ( 32.50000000000000000, 24.99999999999999289, -3.980102097228898626E-15 ) ) ;
#33634 = CARTESIAN_POINT ( 'NONE',  ( -4.732186688966233175E-15, 1.500000000000010880, 25.76082449383753925 ) ) ;
#33635 = CARTESIAN_POINT ( 'NONE',  ( 27.16883889988623935, 70.32500000273117280, -19.73931689729374384 ) ) ;
#33636 = CARTESIAN_POINT ( 'NONE',  ( 10.04305231718578817, 63.39999999999999858, -30.90933677959249337 ) ) ;
#33637 = CARTESIAN_POINT ( 'NONE',  ( 0.000000000000000000, -12.99999999999999822, 0.000000000000000000 ) ) ;
#33638 = CARTESIAN_POINT ( 'NONE',  ( -27.16883889988623935, 59.57500000273119412, 19.73931689729374739 ) ) ;
#33639 = CARTESIAN_POINT ( 'NONE',  ( 12.13525491562421088, 73.05000000546240813, 8.816778784387095058 ) ) ;
#33640 = AXIS2_PLACEMENT_3D ( 'NONE', #5670, #2239, #15981 ) ;
#33641 = CARTESIAN_POINT ( 'NONE',  ( 32.50000000000000000, 73.00000000000001421, -3.980102097228898626E-15 ) ) ;
#33642 = CARTESIAN_POINT ( 'NONE',  ( 27.16883889988624290, 13.92500000273116889, 19.73931689729373673 ) ) ;
#33643 = CARTESIAN_POINT ( 'NONE',  ( 1.577395562988744260E-15, 12.24999999453763522, -25.76082449383753925 ) ) ;
#33644 = CARTESIAN_POINT ( 'NONE',  ( 24.18731323226247554, 25.32590250092397710, 14.01125832528285997 ) ) ;
#33645 = CARTESIAN_POINT ( 'NONE',  ( 23.31009017153205320, 66.99999999999998579, -23.30172593756741506 ) ) ;
#33646 = CARTESIAN_POINT ( 'NONE',  ( -20.75514604977248112, 39.42500000273118843, 28.56700777964554661 ) ) ;
#33647 = CARTESIAN_POINT ( 'NONE',  ( -1.137977401836464321E-14, 52.00000000000000711, 46.18802153517007270 ) ) ;
#33648 = CARTESIAN_POINT ( 'NONE',  ( -4.000000000000003553, 30.00000000000008171, -8.673617379884035472E-16 ) ) ;
#33649 = CARTESIAN_POINT ( 'NONE',  ( -9.270509831248423538, 81.69999999999997442, -12.75976212528059861 ) ) ;
#33650 = CARTESIAN_POINT ( 'NONE',  ( 14.97647472619900455, 35.34076416574268364, -26.02091320914876960 ) ) ;
#33651 = CARTESIAN_POINT ( 'NONE',  ( -2.092463501923844636E-15, 62.00000000546238255, -34.17252228774368916 ) ) ;
#33652 = CARTESIAN_POINT ( 'NONE',  ( -13.91746824999999532, 75.47500000273116427, 4.522059556121122093 ) ) ;
#33653 = CARTESIAN_POINT ( 'NONE',  ( 5.147494310547426899, 63.44874571845315359, -32.50000000000000000 ) ) ;
#33654 = CARTESIAN_POINT ( 'NONE',  ( -26.06988505166722803, 64.98920166574268364, 7.025853678916877953 ) ) ;
#33655 = CARTESIAN_POINT ( 'NONE',  ( -1.778240108872766143E-15, 64.00000000546238255, -32.49999999999999289 ) ) ;
#33656 = CARTESIAN_POINT ( 'NONE',  ( 26.29305231718579350, 73.30000000546237970, 19.10302069950537529 ) ) ;
#33657 = CARTESIAN_POINT ( 'NONE',  ( -28.01184896238290278, 14.86458333333333037, 7.505752307973363457 ) ) ;
#33658 = CARTESIAN_POINT ( 'NONE',  ( 20.75514604977248467, 32.67500000273118843, -28.56700777964554305 ) ) ;
#33659 = CARTESIAN_POINT ( 'NONE',  ( -18.94512977948575738, 5.924999997268809437, -13.76444248337723231 ) ) ;
#33660 = ORIENTED_EDGE ( 'NONE', *, *, #27184, .T. ) ;
#33661 = CARTESIAN_POINT ( 'NONE',  ( 20.75514604977249178, 76.07500000273118701, 28.56700777964553950 ) ) ;
#33662 = AXIS2_PLACEMENT_3D ( 'NONE', #16201, #21182, #3150 ) ;
#33663 = CARTESIAN_POINT ( 'NONE',  ( -32.50000000000000000, 22.60000000546236976, 10.55989012756946366 ) ) ;
#33664 = CARTESIAN_POINT ( 'NONE',  ( -20.50609665441004736, 39.49999999999999289, -20.50609665440969565 ) ) ;
#33665 = CARTESIAN_POINT ( 'NONE',  ( -2.584737979205441561E-13, 63.99218749999997868, -30.02300923189239512 ) ) ;
#33666 = CARTESIAN_POINT ( 'NONE',  ( -10.37757302488623701, 51.77500000273118985, 31.93888565452638417 ) ) ;
#33667 = CARTESIAN_POINT ( 'NONE',  ( -32.50000000000000000, 60.50000000546237544, 0.000000000000000000 ) ) ;
#33668 = ORIENTED_EDGE ( 'NONE', *, *, #18935, .F. ) ;
#33669 = CARTESIAN_POINT ( 'NONE',  ( -10.04305231718578462, 10.90000000546237402, 30.90933677959249337 ) ) ;
#33670 = CARTESIAN_POINT ( 'NONE',  ( -27.16883889988623935, 43.32500000273120833, 19.73931689729374739 ) ) ;
#33671 = CARTESIAN_POINT ( 'NONE',  ( -7.236395654485757944, 17.22499999726881370, -22.27133577429736988 ) ) ;
#33672 = CARTESIAN_POINT ( 'NONE',  ( -20.75514604977248112, 65.67500000273118133, 28.56700777964554661 ) ) ;
#33673 = CARTESIAN_POINT ( 'NONE',  ( -32.50000000000000000, 4.600000005462387520, 10.55989012756946366 ) ) ;
#33674 = CARTESIAN_POINT ( 'NONE',  ( 10.37757302488624767, 59.72500000273119269, 31.93888565452638417 ) ) ;
#33675 = CARTESIAN_POINT ( 'NONE',  ( 28.01184896238290278, 13.14583333333332860, -7.505752307973347470 ) ) ;
#33676 = CARTESIAN_POINT ( 'NONE',  ( 20.08610463437157279, 47.29999999999999005, -27.64615127144129758 ) ) ;
#33677 = CARTESIAN_POINT ( 'NONE',  ( 40.00000000000000000, 52.00000000000000711, -23.09401076758505766 ) ) ;
#33678 = CARTESIAN_POINT ( 'NONE',  ( -33.58253175000000113, 11.37500000273117351, 0.000000000000000000 ) ) ;
#33679 = CARTESIAN_POINT ( 'NONE',  ( 0.000000000000000000, 82.00000000000001421, -15.00000000000000000 ) ) ;
#33680 = CARTESIAN_POINT ( 'NONE',  ( -7.025853678916861966, 31.47357666574268364, -26.06988505166722803 ) ) ;
#33681 = CARTESIAN_POINT ( 'NONE',  ( 13.91746824999999532, 80.47500000273119269, -4.522059556121118540 ) ) ;
#33682 = CARTESIAN_POINT ( 'NONE',  ( -2.162160676586882350E-15, 76.87500000273115575, -35.31076352940722529 ) ) ;
#33683 = FACE_OUTER_BOUND ( 'NONE', #15871, .T. ) ;
#33684 = CARTESIAN_POINT ( 'NONE',  ( 6.486482029760649416E-15, 71.87500000273116996, 35.31076352940723240 ) ) ;
#33685 = ORIENTED_EDGE ( 'NONE', *, *, #11771, .T. ) ;
#33686 = CARTESIAN_POINT ( 'NONE',  ( 14.47279130897151767, 13.42499999726880411, -19.92008829642072598 ) ) ;
#33687 = CARTESIAN_POINT ( 'NONE',  ( -18.94512977948575738, 5.424999997268809437, -13.76444248337723231 ) ) ;
#33688 = AXIS2_PLACEMENT_3D ( 'NONE', #4079, #17816, #20222 ) ;
#33689 = CARTESIAN_POINT ( 'NONE',  ( 24.20753774853756113, 47.95052083333331439, 13.97622843553589789 ) ) ;
#33690 = CARTESIAN_POINT ( 'NONE',  ( -27.16883889988623935, 57.32500000273120833, 19.73931689729374739 ) ) ;
#33691 = CARTESIAN_POINT ( 'NONE',  ( 20.75514604977248467, 16.67500000273117777, -28.56700777964554305 ) ) ;
#33692 = CARTESIAN_POINT ( 'NONE',  ( -2.162160676586881955E-15, 8.875000002731189497, -35.31076352940723240 ) ) ;
#33693 = CARTESIAN_POINT ( 'NONE',  ( 6.988114217767829928, 33.19791666666665719, -26.07999730980489872 ) ) ;
#33694 = CARTESIAN_POINT ( 'NONE',  ( -20.47846945139902175, 23.75038166759064140, -20.53372385742072481 ) ) ;
#33695 = EDGE_CURVE ( 'NONE', #33138, #27031, #12475, .T. ) ;
#33696 = CARTESIAN_POINT ( 'NONE',  ( -26.00068869287340334, 62.84635416666667851, 15.01150461594643382 ) ) ;
#33697 = CARTESIAN_POINT ( 'NONE',  ( -10.37757302488623701, 1.525000002731188964, 31.93888565452638417 ) ) ;
#33698 = CARTESIAN_POINT ( 'NONE',  ( 30.82792611048020603, 52.00000000000000711, -12.22707559850320891 ) ) ;
#33699 = CARTESIAN_POINT ( 'NONE',  ( 32.50000000000000000, 43.10000000000000853, -10.55989012756945833 ) ) ;
#33700 = CARTESIAN_POINT ( 'NONE',  ( -20.75514604977248112, 45.42500000273118843, 28.56700777964554661 ) ) ;
#33701 = CARTESIAN_POINT ( 'NONE',  ( -4.523095164977116484E-15, 8.124999997268826490, 24.62258325217400312 ) ) ;
#33702 = EDGE_CURVE ( 'NONE', #3731, #1393, #1232, .T. ) ;
#33703 = EDGE_CURVE ( 'NONE', #32341, #16033, #25503, .T. ) ;
#33704 = CARTESIAN_POINT ( 'NONE',  ( 12.13525491562420910, 79.19999999999998863, -8.816778784387098611 ) ) ;
#33705 = ORIENTED_EDGE ( 'NONE', *, *, #6564, .F. ) ;
#33706 = CARTESIAN_POINT ( 'NONE',  ( -33.58253175000000113, 51.37500000273119127, 0.000000000000000000 ) ) ;
#33707 = CARTESIAN_POINT ( 'NONE',  ( 10.04305231718578817, 59.90000000546237402, -30.90933677959249337 ) ) ;
#33708 = CARTESIAN_POINT ( 'NONE',  ( 13.94119854578937812, 46.23736083425730925, 24.22776226481240514 ) ) ;
#33709 = CARTESIAN_POINT ( 'NONE',  ( -10.37757302488623701, 75.77500000273118985, 31.93888565452638417 ) ) ;
#33710 = VERTEX_POINT ( 'NONE', #21235 ) ;
#33711 = CARTESIAN_POINT ( 'NONE',  ( -33.58253175000000113, 27.02500000273119696, -10.91162601494193218 ) ) ;
#33712 = EDGE_CURVE ( 'NONE', #3815, #22014, #25856, .T. ) ;
#33713 = CARTESIAN_POINT ( 'NONE',  ( -28.01184896238290278, 14.86458333333333037, 7.505752307973363457 ) ) ;
#33714 = AXIS2_PLACEMENT_3D ( 'NONE', #12891, #3108, #18392 ) ;
#33715 = ORIENTED_EDGE ( 'NONE', *, *, #2822, .F. ) ;
#33716 = CARTESIAN_POINT ( 'NONE',  ( -20.08610463437157989, 57.70000000000000995, -27.64615127144129758 ) ) ;
#33717 = CARTESIAN_POINT ( 'NONE',  ( -10.37757302488624411, 60.72500000273117848, -31.93888565452638417 ) ) ;
#33718 = CARTESIAN_POINT ( 'NONE',  ( -2.584737979205441561E-13, 39.92968750000000000, -30.02300923189239512 ) ) ;
#33719 = CARTESIAN_POINT ( 'NONE',  ( -19.09188309203694445, 11.99999999999999645, -19.09188309203661049 ) ) ;
#33720 = CARTESIAN_POINT ( 'NONE',  ( 18.94512977948576093, 3.324999997268818230, -13.76444248337722875 ) ) ;
#33721 = CARTESIAN_POINT ( 'NONE',  ( 10.37757302488624767, 3.725000002731182480, 31.93888565452638417 ) ) ;
#33722 = CARTESIAN_POINT ( 'NONE',  ( -15.14183272437242778, 7.049999994537622605, 20.84094480462497856 ) ) ;
#33723 = CARTESIAN_POINT ( 'NONE',  ( 26.02091320914876960, 56.82513916574268364, 14.97647472619900455 ) ) ;
#33724 = CARTESIAN_POINT ( 'NONE',  ( -15.00000000000000000, 74.00000000000001421, 0.000000000000000000 ) ) ;
#33725 = DIRECTION ( 'NONE',  ( -0.000000000000000000, -1.000000000000000000, -0.000000000000000000 ) ) ;
#33726 = CARTESIAN_POINT ( 'NONE',  ( -7.570916362186210335, 14.34999999453762065, -23.30088464923126779 ) ) ;
#33727 = CARTESIAN_POINT ( 'NONE',  ( -10.04305231718578462, 14.40000000000000924, 30.90933677959249337 ) ) ;
#33728 = CARTESIAN_POINT ( 'NONE',  ( -15.14183272437242600, 11.04999999453761284, 20.84094480462497856 ) ) ;
#33729 = CARTESIAN_POINT ( 'NONE',  ( 11.25946833292375793, 80.07500000273121543, -8.180482586598735395 ) ) ;
#33730 = CARTESIAN_POINT ( 'NONE',  ( 26.07999730980490227, 20.30729166666666430, 6.988114217767821046 ) ) ;
#33731 = CARTESIAN_POINT ( 'NONE',  ( 6.486482029760649416E-15, 33.62500000273119127, 35.31076352940723240 ) ) ;
#33732 = AXIS2_PLACEMENT_3D ( 'NONE', #31362, #18513, #29291 ) ;
#33733 = CARTESIAN_POINT ( 'NONE',  ( 13.91746824999999887, 71.87500000273122680, -1.704398294459741270E-15 ) ) ;
#33734 = CARTESIAN_POINT ( 'NONE',  ( 33.58253175000000113, 34.47500000273119980, -10.91162601494193751 ) ) ;
#33735 = CARTESIAN_POINT ( 'NONE',  ( 20.75514604977249178, 24.07500000273120477, 28.56700777964553950 ) ) ;
#33736 = CARTESIAN_POINT ( 'NONE',  ( -26.29305231718578995, 64.20000000000000284, 19.10302069950538595 ) ) ;
#33737 = CARTESIAN_POINT ( 'NONE',  ( -2.162160676586882350E-15, 78.62500000273116996, -35.31076352940722529 ) ) ;
#33738 = CIRCLE ( 'NONE', #11794, 32.50000000000000000 ) ;
#33739 = DIRECTION ( 'NONE',  ( -0.000000000000000000, -1.000000000000000000, -0.000000000000000000 ) ) ;
#33740 = SHAPE_REPRESENTATION ( 'connector', ( #1376 ), #33173 ) ;
#33741 = CARTESIAN_POINT ( 'NONE',  ( -2.092463501923844636E-15, 61.50000000000000000, -34.17252228774368916 ) ) ;
#33742 = CARTESIAN_POINT ( 'NONE',  ( 7.236395654485755280, 18.22499999726881370, 22.27133577429736988 ) ) ;
#33743 = CARTESIAN_POINT ( 'NONE',  ( 20.75514604977249178, 61.82500000273117280, 28.56700777964553950 ) ) ;
#33744 = CARTESIAN_POINT ( 'NONE',  ( 7.236395654485760609, 11.52499999726880375, -22.27133577429736633 ) ) ;
#33745 = CARTESIAN_POINT ( 'NONE',  ( -27.16883889988623935, 71.57500000273118701, 19.73931689729374739 ) ) ;
#33746 = CARTESIAN_POINT ( 'NONE',  ( -27.16883889988623935, 7.325000002731174575, 19.73931689729374739 ) ) ;
#33747 = VECTOR ( 'NONE', #19782, 1000.000000000000000 ) ;
#33748 = CARTESIAN_POINT ( 'NONE',  ( 7.236395654485755280, 16.72499999726881370, 22.27133577429736988 ) ) ;
#33749 = CARTESIAN_POINT ( 'NONE',  ( 24.18731323226247554, 18.45090250092397355, 14.01125832528285997 ) ) ;
#33750 = CIRCLE ( 'NONE', #26443, 13.32050807568876927 ) ;
#33751 = VERTEX_POINT ( 'NONE', #10924 ) ;
#33752 = CARTESIAN_POINT ( 'NONE',  ( -33.58253175000000113, 41.22500000273118559, 10.91162601494193929 ) ) ;
#33753 = EDGE_LOOP ( 'NONE', ( #30015, #12468, #19440, #7871, #10833, #17521, #8244, #7210, #12605, #10208, #28765, #7792, #3151, #33135 ) ) ;
#33754 = EDGE_CURVE ( 'NONE', #18447, #1729, #13156, .T. ) ;
#33755 = VERTEX_POINT ( 'NONE', #23971 ) ;
#33756 = CARTESIAN_POINT ( 'NONE',  ( -7.505752307973343918, 39.78645833333332860, -28.01184896238290989 ) ) ;
#33757 = CARTESIAN_POINT ( 'NONE',  ( 24.50000000000000000, 10.00000000000000888, 0.000000000000000000 ) ) ;
#33758 = CARTESIAN_POINT ( 'NONE',  ( 32.50000000000000711, 1.400000005462371799, 10.55989012756945122 ) ) ;
#33759 = CARTESIAN_POINT ( 'NONE',  ( 10.37757302488624056, 78.52500000273118985, -31.93888565452638417 ) ) ;
#33760 = CARTESIAN_POINT ( 'NONE',  ( -4.523095164977116484E-15, 2.624999997268825158, 24.62258325217400312 ) ) ;
#33761 = CARTESIAN_POINT ( 'NONE',  ( 19.82091636218621389, 2.200000000000007283, -14.40073868116559197 ) ) ;
#33762 = CARTESIAN_POINT ( 'NONE',  ( 33.58253175000000113, 18.47500000273117848, -10.91162601494193751 ) ) ;
#33763 = CARTESIAN_POINT ( 'NONE',  ( -26.29305231718579350, 18.30000000546239036, -19.10302069950537884 ) ) ;
#33764 = CARTESIAN_POINT ( 'NONE',  ( 32.50000000000000000, 63.00000000000000000, -3.980102097228898626E-15 ) ) ;
#33765 = CARTESIAN_POINT ( 'NONE',  ( 3.445340210940985210E-14, 5.499999999999997335, 24.50000000000000000 ) ) ;
#33766 = CARTESIAN_POINT ( 'NONE',  ( 0.000000000000000000, 0.000000000000000000, 0.000000000000000000 ) ) ;
#33767 = CARTESIAN_POINT ( 'NONE',  ( -28.00173670424549499, 61.27642333425730925, -7.543491769121417612 ) ) ;
#33768 = CARTESIAN_POINT ( 'NONE',  ( 4.300734207923757602, 80.77500000273118985, -13.23629886949340673 ) ) ;
#33769 = CARTESIAN_POINT ( 'NONE',  ( 2.740863092043355209E-13, 38.21093750000000000, 30.02300923189239867 ) ) ;
#33770 = APPLICATION_PROTOCOL_DEFINITION ( 'draft international standard', 'automotive_design', 1998, #4386 ) ;
#33771 = DIRECTION ( 'NONE',  ( 0.000000000000000000, 0.000000000000000000, -1.000000000000000000 ) ) ;
#33772 = CARTESIAN_POINT ( 'NONE',  ( -7.236395654485763274, 18.52499999726881086, 22.27133577429736633 ) ) ;
#33773 = CARTESIAN_POINT ( 'NONE',  ( -32.50000000000000000, 5.899999999999987921, -10.55989012756945478 ) ) ;
#33774 = DIRECTION ( 'NONE',  ( -1.000000000000000000, 0.000000000000000000, 0.000000000000000000 ) ) ;
#33775 = CARTESIAN_POINT ( 'NONE',  ( 24.22776226481265383, 53.38763916574269786, 13.94119854578893580 ) ) ;
#33776 = CARTESIAN_POINT ( 'NONE',  ( 10.37757302488624056, 52.52500000273118985, -31.93888565452638417 ) ) ;
#33777 = CARTESIAN_POINT ( 'NONE',  ( -33.58253175000000113, 65.27500000273117564, -10.91162601494193218 ) ) ;
#33778 = CARTESIAN_POINT ( 'NONE',  ( 20.75514604977249178, 42.07500000273118701, 28.56700777964553950 ) ) ;
#33779 = PLANE ( 'NONE',  #33732 ) ;
#33780 = CARTESIAN_POINT ( 'NONE',  ( 24.20753774853731244, 13.00260416666666430, -13.97622843553633132 ) ) ;
#33781 = DIRECTION ( 'NONE',  ( 0.000000000000000000, 1.000000000000000000, 0.000000000000000000 ) ) ;
#33782 = CARTESIAN_POINT ( 'NONE',  ( 0.000000000000000000, 16.99999999999998579, 0.000000000000000000 ) ) ;
#33783 = CARTESIAN_POINT ( 'NONE',  ( -32.50000000000000000, 77.90000000000001990, -10.55989012756945478 ) ) ;
#33784 = CARTESIAN_POINT ( 'NONE',  ( -2.162160676586881955E-15, 16.62500000273120548, -35.31076352940723240 ) ) ;
#33785 = CARTESIAN_POINT ( 'NONE',  ( -32.50000000000000000, 62.40000000546236691, -10.55989012756945300 ) ) ;
#33786 = CARTESIAN_POINT ( 'NONE',  ( 0.000000000000000000, 16.99999999999998579, 0.000000000000000000 ) ) ;
#33787 = CARTESIAN_POINT ( 'NONE',  ( 3.000384657911015469E-15, 16.99999999999998579, 24.50000000000000000 ) ) ;
#33788 = CARTESIAN_POINT ( 'NONE',  ( -24.22776226481266448, 17.29388916574268720, -13.94119854578892514 ) ) ;
#33789 = CARTESIAN_POINT ( 'NONE',  ( -32.50000000000000000, 34.50000000546236834, 0.000000000000000000 ) ) ;
#33790 = CARTESIAN_POINT ( 'NONE',  ( -5.147494310547430452, 11.55125428154683753, -32.49999999999999289 ) ) ;
#33791 = CARTESIAN_POINT ( 'NONE',  ( 27.16883889988624290, 27.92500000273118133, 19.73931689729373673 ) ) ;
#33792 = CARTESIAN_POINT ( 'NONE',  ( -24.20753774853730889, 45.65885416666666430, 13.97622843553633842 ) ) ;
#33793 = ORIENTED_EDGE ( 'NONE', *, *, #20502, .T. ) ;
#33794 = CARTESIAN_POINT ( 'NONE',  ( 10.37757302488624767, 61.72500000273119269, 31.93888565452638417 ) ) ;
#33795 = CARTESIAN_POINT ( 'NONE',  ( 7.505752307972854531, 46.94791666666666430, -28.01184896238303423 ) ) ;
#33796 = ORIENTED_EDGE ( 'NONE', *, *, #4955, .F. ) ;
#33797 = CARTESIAN_POINT ( 'NONE',  ( -28.01184896238304134, 15.15104166666666252, -7.505752307972844761 ) ) ;
#33798 = CARTESIAN_POINT ( 'NONE',  ( -26.02091320914849959, 12.72173583425731458, 14.97647472619947528 ) ) ;
#33799 = CARTESIAN_POINT ( 'NONE',  ( -2.162160676586881955E-15, 8.625000002731180615, -35.31076352940723240 ) ) ;
#33800 = EDGE_CURVE ( 'NONE', #25557, #29691, #8337, .T. ) ;
#33801 = DIRECTION ( 'NONE',  ( 0.000000000000000000, -1.000000000000000000, 0.000000000000000000 ) ) ;
#33802 = AXIS2_PLACEMENT_3D ( 'NONE', #6502, #833, #8899 ) ;
#33803 = CARTESIAN_POINT ( 'NONE',  ( -2.162160676586881955E-15, 34.87500000273117706, -35.31076352940723240 ) ) ;
#33804 = CARTESIAN_POINT ( 'NONE',  ( 20.08610463437157279, 39.80000000546238681, -27.64615127144129758 ) ) ;
#33805 = CARTESIAN_POINT ( 'NONE',  ( 4.635254915624212657, 78.60000000000000853, 14.26584774442730286 ) ) ;
#33806 = CARTESIAN_POINT ( 'NONE',  ( -33.58253175000000113, 21.12500000273118062, 0.000000000000000000 ) ) ;
#33807 = CARTESIAN_POINT ( 'NONE',  ( -10.04305231718579172, 52.10000000546237686, -30.90933677959248982 ) ) ;
#33808 = CARTESIAN_POINT ( 'NONE',  ( -27.16883889988624290, 51.17500000273117422, -19.73931689729374028 ) ) ;
#33809 =( NAMED_UNIT ( * ) SI_UNIT ( $, .STERADIAN. ) SOLID_ANGLE_UNIT ( ) );
#33810 = CARTESIAN_POINT ( 'NONE',  ( -20.08610463437157989, 31.69999999999998508, -27.64615127144129758 ) ) ;
#33811 = CARTESIAN_POINT ( 'NONE',  ( 20.08610463437158344, 26.70000000000000284, 27.64615127144129403 ) ) ;
#33812 = CARTESIAN_POINT ( 'NONE',  ( 7.570916362186213000, 6.399999999999988809, -23.30088464923126423 ) ) ;
#33813 = CARTESIAN_POINT ( 'NONE',  ( 10.37757302488624767, 69.72500000273117848, 31.93888565452638417 ) ) ;
#33814 = CARTESIAN_POINT ( 'NONE',  ( -33.29860495311159951, 66.99999999999998579, 1.751800823569703791 ) ) ;
#33815 = CARTESIAN_POINT ( 'NONE',  ( 1.555960095263670572E-15, 14.50000000000000178, -24.50000000000000000 ) ) ;
#33816 = CARTESIAN_POINT ( 'NONE',  ( 20.75514604977248467, 60.67500000273118133, -28.56700777964554305 ) ) ;
#33817 = CARTESIAN_POINT ( 'NONE',  ( -33.58253175000000113, 11.12500000273120015, 0.000000000000000000 ) ) ;
#33818 = CARTESIAN_POINT ( 'NONE',  ( -0.04044903254992426173, 25.89881916759064140, 27.95245687107223276 ) ) ;
#33819 = CARTESIAN_POINT ( 'NONE',  ( 29.96643421716999356, 66.99999999999997158, -13.17858490638464986 ) ) ;
#33820 = CARTESIAN_POINT ( 'NONE',  ( -10.37757302488623701, 33.52500000273118985, 31.93888565452638417 ) ) ;
#33821 = CARTESIAN_POINT ( 'NONE',  ( 2.205017735002230837E-13, 57.49999999999998579, -32.50000000000000000 ) ) ;
#33822 = FACE_OUTER_BOUND ( 'NONE', #4706, .T. ) ;
#33823 = CARTESIAN_POINT ( 'NONE',  ( -4.300734207923755825, 75.27500000273118985, 13.23629886949340673 ) ) ;
#33824 = CARTESIAN_POINT ( 'NONE',  ( 15.04653450569339945, 50.23659749907603356, 25.98046417659831775 ) ) ;
#33825 = CARTESIAN_POINT ( 'NONE',  ( 26.29305231718578995, 53.70000000546236407, -19.10302069950538240 ) ) ;
#33826 = CARTESIAN_POINT ( 'NONE',  ( -13.91746824999999887, 77.37500000273116996, 0.000000000000000000 ) ) ;
#33827 = CARTESIAN_POINT ( 'NONE',  ( 19.09188309203694800, 17.15624999999999645, 19.09188309203660694 ) ) ;
#33828 = FACE_OUTER_BOUND ( 'NONE', #17915, .T. ) ;
#33829 = VECTOR ( 'NONE', #17413, 1000.000000000000000 ) ;
#33830 = CARTESIAN_POINT ( 'NONE',  ( -32.50000000000000000, 66.60000000546236265, 10.55989012756946366 ) ) ;
#33831 = CARTESIAN_POINT ( 'NONE',  ( -15.01150461594642138, 19.01822916666666785, -26.00068869287340334 ) ) ;
#33832 = CARTESIAN_POINT ( 'NONE',  ( -10.37757302488624411, 36.97500000273119980, -31.93888565452638417 ) ) ;
#33833 = CARTESIAN_POINT ( 'NONE',  ( -23.41746824999999887, 10.02499999726882507, -7.608796670333730638 ) ) ;
#33834 = ORIENTED_EDGE ( 'NONE', *, *, #8918, .F. ) ;
#33835 = CARTESIAN_POINT ( 'NONE',  ( -20.75514604977248823, 75.07500000273118701, -28.56700777964554305 ) ) ;
#33836 = CARTESIAN_POINT ( 'NONE',  ( 10.04305231718578817, 25.90000000546237402, -30.90933677959249337 ) ) ;
#33837 = CARTESIAN_POINT ( 'NONE',  ( -26.00068869287368756, 46.23177083333331439, -15.01150461594595775 ) ) ;
#33838 = CARTESIAN_POINT ( 'NONE',  ( -2.584737979205441561E-13, 57.11718750000000711, -30.02300923189239512 ) ) ;
#33839 = EDGE_CURVE ( 'NONE', #25478, #20831, #19897, .T. ) ;
#33840 = CARTESIAN_POINT ( 'NONE',  ( 33.58253175000000823, 54.27500000273118275, 10.91162601494192863 ) ) ;
#33841 = EDGE_CURVE ( 'NONE', #29096, #12812, #4561, .T. ) ;
#33842 = CARTESIAN_POINT ( 'NONE',  ( 32.50000000000000000, 57.60000000546237686, -10.55989012756945833 ) ) ;
#33843 = DIRECTION ( 'NONE',  ( -0.000000000000000000, 1.000000000000000000, -0.000000000000000000 ) ) ;
#33844 = CARTESIAN_POINT ( 'NONE',  ( 10.37757302488624767, 41.72500000273118559, 31.93888565452638417 ) ) ;
#33845 = CARTESIAN_POINT ( 'NONE',  ( -15.00000000000000000, 72.09999999999999432, 4.873795443493597723 ) ) ;
#33846 = CARTESIAN_POINT ( 'NONE',  ( 27.16883889988623935, 66.57500000273120122, -19.73931689729374384 ) ) ;
#33847 = CARTESIAN_POINT ( 'NONE',  ( -32.50000000000000000, 8.400000005462384678, -10.55989012756945478 ) ) ;
#33848 = CARTESIAN_POINT ( 'NONE',  ( 33.58253175000000113, 64.22500000273117848, -10.91162601494193574 ) ) ;
#33849 = CARTESIAN_POINT ( 'NONE',  ( 7.505752307973351023, 14.00520833333333215, 28.01184896238290278 ) ) ;
#33850 = CARTESIAN_POINT ( 'NONE',  ( 10.04305231718578817, 47.39999999999999858, -30.90933677959249337 ) ) ;
#33851 = CARTESIAN_POINT ( 'NONE',  ( -23.41746824999999887, 5.624999997268814944, -2.867812753649727150E-15 ) ) ;
#33852 = CARTESIAN_POINT ( 'NONE',  ( 33.58253175000000113, 12.37500000273117351, -4.112674001490185761E-15 ) ) ;
#33853 = FACE_OUTER_BOUND ( 'NONE', #22051, .T. ) ;
#33854 = CARTESIAN_POINT ( 'NONE',  ( -24.22776226481266448, 34.48138916574268364, -13.94119854578892514 ) ) ;
#33855 = CARTESIAN_POINT ( 'NONE',  ( -11.25946833292375793, 77.17500000273119554, -8.180482586598733619 ) ) ;
#33856 = FACE_OUTER_BOUND ( 'NONE', #22420, .T. ) ;
#33857 = VECTOR ( 'NONE', #25765, 1000.000000000000114 ) ;
#33858 = CARTESIAN_POINT ( 'NONE',  ( 6.486482029760649416E-15, 77.87500000273118417, 35.31076352940723240 ) ) ;
#33859 = ORIENTED_EDGE ( 'NONE', *, *, #741, .T. ) ;
#33860 = CARTESIAN_POINT ( 'NONE',  ( -7.236395654485757944, 15.72499999726881192, -22.27133577429736988 ) ) ;
#33861 = CARTESIAN_POINT ( 'NONE',  ( -26.07999730980490583, 59.83854166666666430, -6.988114217767815717 ) ) ;
#33862 = ADVANCED_FACE ( 'NONE', ( #5265 ), #32610, .F. ) ;
#33863 = CARTESIAN_POINT ( 'NONE',  ( -20.75514604977248112, 51.42500000273118133, 28.56700777964554661 ) ) ;
#33864 = CARTESIAN_POINT ( 'NONE',  ( 10.37757302488624767, 19.97500000273118204, 31.93888565452638417 ) ) ;
#33865 = CARTESIAN_POINT ( 'NONE',  ( -20.75514604977248112, 3.675000002731193316, 28.56700777964554661 ) ) ;
#33866 = CARTESIAN_POINT ( 'NONE',  ( -6.988114217767819270, 45.22916666666665719, 26.07999730980490583 ) ) ;
#33867 = CARTESIAN_POINT ( 'NONE',  ( 25.98046417659858420, 25.32590250092397710, 15.04653450569292872 ) ) ;
#33868 = CARTESIAN_POINT ( 'NONE',  ( 25.98046417659831775, 21.87722249907602290, -15.04653450569338879 ) ) ;
#33869 = CARTESIAN_POINT ( 'NONE',  ( 20.75514604977249178, 5.825000002731183457, 28.56700777964553950 ) ) ;
#33870 = CARTESIAN_POINT ( 'NONE',  ( 0.000000000000000000, 80.00000000000001421, 0.000000000000000000 ) ) ;
#33871 = CARTESIAN_POINT ( 'NONE',  ( 10.37757302488624767, 45.72500000273119269, 31.93888565452638417 ) ) ;
#33872 = CARTESIAN_POINT ( 'NONE',  ( -18.94512977948575738, 9.424999997268812990, -13.76444248337723231 ) ) ;
#33873 = CARTESIAN_POINT ( 'NONE',  ( 0.000000000000000000, -10.99999999999999645, -33.00000000000000000 ) ) ;
#33874 = VERTEX_POINT ( 'NONE', #16173 ) ;
#33875 = CARTESIAN_POINT ( 'NONE',  ( -2.162160676586881955E-15, 52.87500000273119838, -35.31076352940723240 ) ) ;
#33876 = CARTESIAN_POINT ( 'NONE',  ( -11.54700538379251995, 96.00000000000002842, -19.99999999999999645 ) ) ;
#33877 = CARTESIAN_POINT ( 'NONE',  ( 24.22776226481241224, 38.50298583425730925, -13.94119854578936923 ) ) ;
#33878 = CARTESIAN_POINT ( 'NONE',  ( -2.162160676586881955E-15, 76.87500000273115575, -35.31076352940723240 ) ) ;
#33879 = VERTEX_POINT ( 'NONE', #18243 ) ;
#33880 = CARTESIAN_POINT ( 'NONE',  ( -2.162160676586881955E-15, 22.62500000273119127, -35.31076352940723240 ) ) ;
#33881 = DIRECTION ( 'NONE',  ( 1.000000000000000000, 0.000000000000000000, 0.000000000000000000 ) ) ;
#33882 = AXIS2_PLACEMENT_3D ( 'NONE', #27500, #15150, #25614 ) ;
#33883 = EDGE_LOOP ( 'NONE', ( #30777, #13030, #28724, #3235 ) ) ;
#33884 = CARTESIAN_POINT ( 'NONE',  ( -32.50000000000000000, 14.60000000546239107, 10.55989012756946366 ) ) ;
#33885 = CARTESIAN_POINT ( 'NONE',  ( -33.58253175000000113, 63.12500000273119127, 0.000000000000000000 ) ) ;
#33886 = CARTESIAN_POINT ( 'NONE',  ( -26.00068869287368756, 46.23177083333331439, -15.01150461594595775 ) ) ;
#33887 = CARTESIAN_POINT ( 'NONE',  ( 24.50000000000000000, 18.00000000000001421, 0.000000000000000000 ) ) ;
#33888 = CARTESIAN_POINT ( 'NONE',  ( -23.41746824999999887, 2.124999997268811391, -2.867812753649727150E-15 ) ) ;
#33889 = CARTESIAN_POINT ( 'NONE',  ( 20.75514604977248467, 2.425000002731189763, -28.56700777964554305 ) ) ;
#33890 = FILL_AREA_STYLE_COLOUR ( '', #8312 ) ;
#33891 = CARTESIAN_POINT ( 'NONE',  ( -0.04044903255044120238, 62.55430583240935505, -30.02300923189239867 ) ) ;
#33892 = CARTESIAN_POINT ( 'NONE',  ( 27.16883889988623935, 78.57500000273121543, -19.73931689729374384 ) ) ;
#33893 = CARTESIAN_POINT ( 'NONE',  ( 20.50609665440969565, 64.42187499999998579, -20.50609665441004736 ) ) ;
#33894 = CARTESIAN_POINT ( 'NONE',  ( 5.147494310547434893, 8.551254281546841085, 32.49999999999999289 ) ) ;
#33895 = ADVANCED_FACE ( 'NONE', ( #26629 ), #27697, .T. ) ;
#33896 = CARTESIAN_POINT ( 'NONE',  ( 10.04305231718578817, 17.40000000000001279, -30.90933677959249337 ) ) ;
#33897 = CARTESIAN_POINT ( 'NONE',  ( 13.97622843553589966, 64.27864583333332860, -24.20753774853756113 ) ) ;
#33898 = CARTESIAN_POINT ( 'NONE',  ( -15.14183272437241889, 14.44999999453762207, -20.84094480462497856 ) ) ;
#33899 = CARTESIAN_POINT ( 'NONE',  ( -13.91746824999999887, 80.87500000273118417, 0.000000000000000000 ) ) ;
#33900 = CARTESIAN_POINT ( 'NONE',  ( -19.09188309203694445, 29.18749999999999645, -19.09188309203661049 ) ) ;
#33901 = CARTESIAN_POINT ( 'NONE',  ( -33.58253175000000113, 31.22500000273118559, 10.91162601494193929 ) ) ;
#33902 = CARTESIAN_POINT ( 'NONE',  ( 6.486482029760649416E-15, 73.62500000273118417, 35.31076352940723240 ) ) ;
#33903 = CARTESIAN_POINT ( 'NONE',  ( 6.486482029760649416E-15, 33.87500000273118417, 35.31076352940723240 ) ) ;
#33904 = CARTESIAN_POINT ( 'NONE',  ( -33.58253175000000113, 13.47500000273118914, 10.91162601494193929 ) ) ;
#33905 = CARTESIAN_POINT ( 'NONE',  ( -2.165007332552593587E-13, 52.50000000000000711, 32.50000000000000000 ) ) ;
#33906 = CARTESIAN_POINT ( 'NONE',  ( 27.95245687107223986, 45.66444416759065916, 0.04044903254993640479 ) ) ;
#33907 = ADVANCED_FACE ( 'NONE', ( #18748 ), #5355, .F. ) ;
#33908 = CARTESIAN_POINT ( 'NONE',  ( -33.58253175000000113, 75.12500000273119838, 0.000000000000000000 ) ) ;
#33909 = CARTESIAN_POINT ( 'NONE',  ( -10.04305231718578462, 66.40000000000001990, 30.90933677959249337 ) ) ;
#33910 = CARTESIAN_POINT ( 'NONE',  ( -10.04305231718578462, 58.39999999999999147, 30.90933677959249337 ) ) ;
#33911 = CARTESIAN_POINT ( 'NONE',  ( 3.980102097228898626E-15, 80.00000000000001421, 32.50000000000000000 ) ) ;
#33912 = CARTESIAN_POINT ( 'NONE',  ( 10.37757302488624767, 61.72500000273117848, 31.93888565452638417 ) ) ;
#33913 = EDGE_CURVE ( 'NONE', #16375, #26497, #10765, .T. ) ;
#33914 = CARTESIAN_POINT ( 'NONE',  ( 23.41746824999999887, 7.124999997268815832, 0.000000000000000000 ) ) ;
#33915 = CARTESIAN_POINT ( 'NONE',  ( -27.16883889988624290, 73.17500000273118133, -19.73931689729374028 ) ) ;
#33916 = CARTESIAN_POINT ( 'NONE',  ( -33.58253175000000113, 5.125000002731194826, 0.000000000000000000 ) ) ;
#33917 = CARTESIAN_POINT ( 'NONE',  ( 23.41746824999999887, 2.624999997268812280, 0.000000000000000000 ) ) ;
#33918 = CARTESIAN_POINT ( 'NONE',  ( -14.01125832528285109, 19.31027750092397710, 24.18731323226248264 ) ) ;
#33919 = ORIENTED_EDGE ( 'NONE', *, *, #19161, .T. ) ;
#33920 = CARTESIAN_POINT ( 'NONE',  ( -2.162160676586881955E-15, 44.62500000273119838, -35.31076352940723240 ) ) ;
#33921 = VERTEX_POINT ( 'NONE', #28689 ) ;
#33922 = CARTESIAN_POINT ( 'NONE',  ( 7.505752307973351023, 44.94270833333332860, 28.01184896238290278 ) ) ;
#33923 = DIRECTION ( 'NONE',  ( -1.000000000000000000, 0.000000000000000000, 0.000000000000000000 ) ) ;
#33924 = CARTESIAN_POINT ( 'NONE',  ( -20.08610463437157989, 2.200000005462375618, -27.64615127144129758 ) ) ;
#33925 = CARTESIAN_POINT ( 'NONE',  ( 10.37757302488624767, 77.72500000273119269, 31.93888565452638417 ) ) ;
#33926 = CARTESIAN_POINT ( 'NONE',  ( 1.507698388325705758E-15, 5.624999997268818497, -24.62258325217400312 ) ) ;
#33927 = CARTESIAN_POINT ( 'NONE',  ( -14.47279130897152122, 15.92499999726881121, 19.92008829642072243 ) ) ;
#33928 = CARTESIAN_POINT ( 'NONE',  ( -27.16883889988624290, 13.17500000273119554, -19.73931689729374028 ) ) ;
#33929 = CARTESIAN_POINT ( 'NONE',  ( 32.50000000000000000, 61.09999999999998721, -10.55989012756945833 ) ) ;
#33930 = CARTESIAN_POINT ( 'NONE',  ( 9.270509831248425314, 76.95000000546239960, 12.75976212528059683 ) ) ;
#33931 = CARTESIAN_POINT ( 'NONE',  ( -26.29305231718579350, 29.79999999999999361, -19.10302069950537884 ) ) ;
#33932 = CARTESIAN_POINT ( 'NONE',  ( 25.98046417659831775, 35.62722249907602645, -15.04653450569338879 ) ) ;
#33933 = CARTESIAN_POINT ( 'NONE',  ( -4.300734207923755825, 75.77500000273118985, 13.23629886949340673 ) ) ;
#33934 = CARTESIAN_POINT ( 'NONE',  ( 15.01150461594596486, 43.65364583333332860, -26.00068869287367690 ) ) ;
#33935 = APPLICATION_PROTOCOL_DEFINITION ( 'draft international standard', 'automotive_design', 1998, #27191 ) ;
#33936 = FACE_OUTER_BOUND ( 'NONE', #28978, .T. ) ;
#33937 = CARTESIAN_POINT ( 'NONE',  ( 10.04305231718579705, 64.59999999999999432, 30.90933677959248982 ) ) ;
#33938 = CARTESIAN_POINT ( 'NONE',  ( 26.29305231718579350, 10.80000000000000426, 19.10302069950537529 ) ) ;
#33939 = CARTESIAN_POINT ( 'NONE',  ( -9.270509831248423538, 73.70000000000000284, -12.75976212528059861 ) ) ;
#33940 = CARTESIAN_POINT ( 'NONE',  ( -7.025853678916861966, 52.09857666574269075, -26.06988505166722803 ) ) ;
#33941 =( BOUNDED_CURVE ( )  B_SPLINE_CURVE ( 2, ( #6673, #7010, #27782, #22976, #4099, #28292, #25033, #14573, #14742, #1513, #12335, #9932, #4437 ),
 .UNSPECIFIED., .F., .T. ) 
 B_SPLINE_CURVE_WITH_KNOTS ( ( 3, 2, 2, 2, 2, 2, 3 ),
 ( 0.8499999999999999778, 0.8599999999999999867, 0.8800000000000000044, 0.9000000000000000222, 0.9200000000000000400, 0.9399999999999999467, 0.9499999999999999556 ),
 .UNSPECIFIED. ) 
 CURVE ( )  GEOMETRIC_REPRESENTATION_ITEM ( )  RATIONAL_B_SPLINE_CURVE ( ( 0.9755282581475768211, 0.9755282581475768211, 1.000000000000000000, 0.9510565162951535312, 1.000000000000000000, 0.9510565162951535312, 1.000000000000000000, 0.9510565162951535312, 1.000000000000000000, 0.9510565162951535312, 1.000000000000000000, 0.9755282581475768211, 0.9755282581475768211 ) ) 
 REPRESENTATION_ITEM ( '' )  );
#33942 = CARTESIAN_POINT ( 'NONE',  ( 20.75514604977248467, 52.42500000273118133, -28.56700777964554305 ) ) ;
#33943 = CARTESIAN_POINT ( 'NONE',  ( -27.16883889988624290, 53.17500000273118843, -19.73931689729374028 ) ) ;
#33944 = CARTESIAN_POINT ( 'NONE',  ( 10.37757302488624767, 43.97500000273119269, 31.93888565452638417 ) ) ;
#33945 = CARTESIAN_POINT ( 'NONE',  ( -24.20753774853756823, 15.29427083333332860, -13.97622843553588723 ) ) ;
#33946 = CARTESIAN_POINT ( 'NONE',  ( -1.778240108872766143E-15, 5.500000000000003553, -32.49999999999999289 ) ) ;
#33947 = CARTESIAN_POINT ( 'NONE',  ( 5.749481115774131901, 16.99999999999999289, -22.78789490266839834 ) ) ;
#33948 = CARTESIAN_POINT ( 'NONE',  ( 20.08610463437157279, 79.30000000000001137, -27.64615127144129758 ) ) ;
#33949 = CARTESIAN_POINT ( 'NONE',  ( 33.58253175000000823, 16.02500000273119340, 10.91162601494192863 ) ) ;
#33950 = CARTESIAN_POINT ( 'NONE',  ( 3.000384657911015469E-15, -20.99999999999998934, 24.50000000000000000 ) ) ;
#33951 = DIRECTION ( 'NONE',  ( 0.000000000000000000, 0.000000000000000000, -1.000000000000000000 ) ) ;
#33952 = CARTESIAN_POINT ( 'NONE',  ( -26.06988505166722803, 16.86420166574268720, 7.025853678916877953 ) ) ;
#33953 = CARTESIAN_POINT ( 'NONE',  ( 26.29305231718579350, 35.30000000546239391, 19.10302069950537529 ) ) ;
#33954 = CARTESIAN_POINT ( 'NONE',  ( -15.14183272437242778, 11.04999999453761284, 20.84094480462497856 ) ) ;
#33955 = CARTESIAN_POINT ( 'NONE',  ( -33.58253175000000113, 25.02500000273117564, -10.91162601494193041 ) ) ;
#33956 = CARTESIAN_POINT ( 'NONE',  ( 24.20753774853756113, 44.51302083333331439, 13.97622843553589789 ) ) ;
#33957 = ORIENTED_EDGE ( 'NONE', *, *, #14925, .T. ) ;
#33958 = CARTESIAN_POINT ( 'NONE',  ( 10.37757302488624056, 62.52500000273118985, -31.93888565452638417 ) ) ;
#33959 = CARTESIAN_POINT ( 'NONE',  ( 30.02300923189239512, 47.66406249999998579, -2.619432448724977703E-13 ) ) ;
#33960 = VERTEX_POINT ( 'NONE', #695 ) ;
#33961 = CARTESIAN_POINT ( 'NONE',  ( -0.04044903254990864921, 63.71131916759064495, 30.02300923189239867 ) ) ;
#33962 = CARTESIAN_POINT ( 'NONE',  ( 30.02300923189239867, 14.72694416759064318, 0.04044903254992252006 ) ) ;
#33963 = VERTEX_POINT ( 'NONE', #18411 ) ;
#33964 = CARTESIAN_POINT ( 'NONE',  ( 33.58253175000000113, 2.225000002731181592, -10.91162601494193751 ) ) ;
#33965 = DIRECTION ( 'NONE',  ( 0.000000000000000000, 0.000000000000000000, -1.000000000000000000 ) ) ;
#33966 = CARTESIAN_POINT ( 'NONE',  ( -33.58253175000000113, 35.47500000273118559, 10.91162601494193929 ) ) ;
#33967 = CARTESIAN_POINT ( 'NONE',  ( -26.29305231718578995, 36.70000000546236407, 19.10302069950538595 ) ) ;
#33968 = CARTESIAN_POINT ( 'NONE',  ( -15.00000000000000000, 74.09999999999999432, 4.873795443493597723 ) ) ;
#33969 = DIRECTION ( 'NONE',  ( -1.224646799147353454E-16, 1.000000000000000000, -0.000000000000000000 ) ) ;
#33970 = CARTESIAN_POINT ( 'NONE',  ( -2.162160676586881955E-15, 20.62500000273119483, -35.31076352940723240 ) ) ;
#33971 = LINE ( 'NONE', #31392, #19791 ) ;
#33972 = CARTESIAN_POINT ( 'NONE',  ( -20.75514604977248112, 47.67500000273118843, 28.56700777964554661 ) ) ;
#33973 =( NAMED_UNIT ( * ) PLANE_ANGLE_UNIT ( ) SI_UNIT ( $, .RADIAN. ) );
#33974 = CARTESIAN_POINT ( 'NONE',  ( -32.50000000000000000, 28.10000000000001208, 10.55989012756946366 ) ) ;
#33975 = CARTESIAN_POINT ( 'NONE',  ( -26.29305231718579350, 25.79999999999999005, -19.10302069950537884 ) ) ;
#33976 = CARTESIAN_POINT ( 'NONE',  ( -7.570916362186210335, 6.599999999999994316, -23.30088464923126779 ) ) ;
#33977 = CARTESIAN_POINT ( 'NONE',  ( 10.37757302488624056, 70.52500000273120406, -31.93888565452638417 ) ) ;
#33978 = CARTESIAN_POINT ( 'NONE',  ( -15.14183272437241889, 2.449999994537622960, -20.84094480462497856 ) ) ;
#33979 = CARTESIAN_POINT ( 'NONE',  ( -6.668671393434016714, 74.00000000000001421, -13.28991759065290168 ) ) ;
#33980 = CARTESIAN_POINT ( 'NONE',  ( -20.75514604977248112, 59.67500000273118133, 28.56700777964554661 ) ) ;
#33981 = CARTESIAN_POINT ( 'NONE',  ( 3.469446951953614189E-15, -57.99999999999999289, 0.000000000000000000 ) ) ;
#33982 = CARTESIAN_POINT ( 'NONE',  ( -27.16883889988623935, 11.32500000273117813, 19.73931689729374739 ) ) ;
#33983 = CARTESIAN_POINT ( 'NONE',  ( -24.18731323226248264, 27.04465250092397000, -14.01125832528284931 ) ) ;
#33984 = EDGE_CURVE ( 'NONE', #7355, #5385, #15835, .T. ) ;
#33985 = CARTESIAN_POINT ( 'NONE',  ( 0.000000000000000000, -20.99999999999998934, -26.50000000000000355 ) ) ;
#33986 = CARTESIAN_POINT ( 'NONE',  ( -27.16883889988623935, 5.575000002731201221, 19.73931689729374739 ) ) ;
#33987 = CARTESIAN_POINT ( 'NONE',  ( 6.486482029760649416E-15, 35.62500000273119127, 35.31076352940723240 ) ) ;
#33988 = CARTESIAN_POINT ( 'NONE',  ( -32.50000000000000000, 64.40000000546238823, -10.55989012756945300 ) ) ;
#33989 = CARTESIAN_POINT ( 'NONE',  ( 20.08610463437158344, 67.20000000546235697, 27.64615127144129403 ) ) ;
#33990 = NEXT_ASSEMBLY_USAGE_OCCURRENCE ( 'NAUO1', ' ', ' ', #5127, #78, $ ) ;
#33991 = NEXT_ASSEMBLY_USAGE_OCCURRENCE ( 'NAUO2', ' ', ' ', #5127, #7646, $ ) ;
#33992 = NEXT_ASSEMBLY_USAGE_OCCURRENCE ( 'NAUO3', ' ', ' ', #5127, #6163, $ ) ;
#33993 = NEXT_ASSEMBLY_USAGE_OCCURRENCE ( 'NAUO4', ' ', ' ', #5127, #16263, $ ) ;
#33994 = NEXT_ASSEMBLY_USAGE_OCCURRENCE ( 'NAUO5', ' ', ' ', #5127, #12245, $ ) ;
#33995 = NEXT_ASSEMBLY_USAGE_OCCURRENCE ( 'NAUO6', ' ', ' ', #5127, #8255, $ ) ;
#33996 = NEXT_ASSEMBLY_USAGE_OCCURRENCE ( 'NAUO7', ' ', ' ', #5127, #18358, $ ) ;
#33997 = NEXT_ASSEMBLY_USAGE_OCCURRENCE ( 'NAUO8', ' ', ' ', #5127, #7646, $ ) ;
#33998 = NEXT_ASSEMBLY_USAGE_OCCURRENCE ( 'NAUO9', ' ', ' ', #5127, #23384, $ ) ;
ENDSEC;
END-ISO-10303-21;
